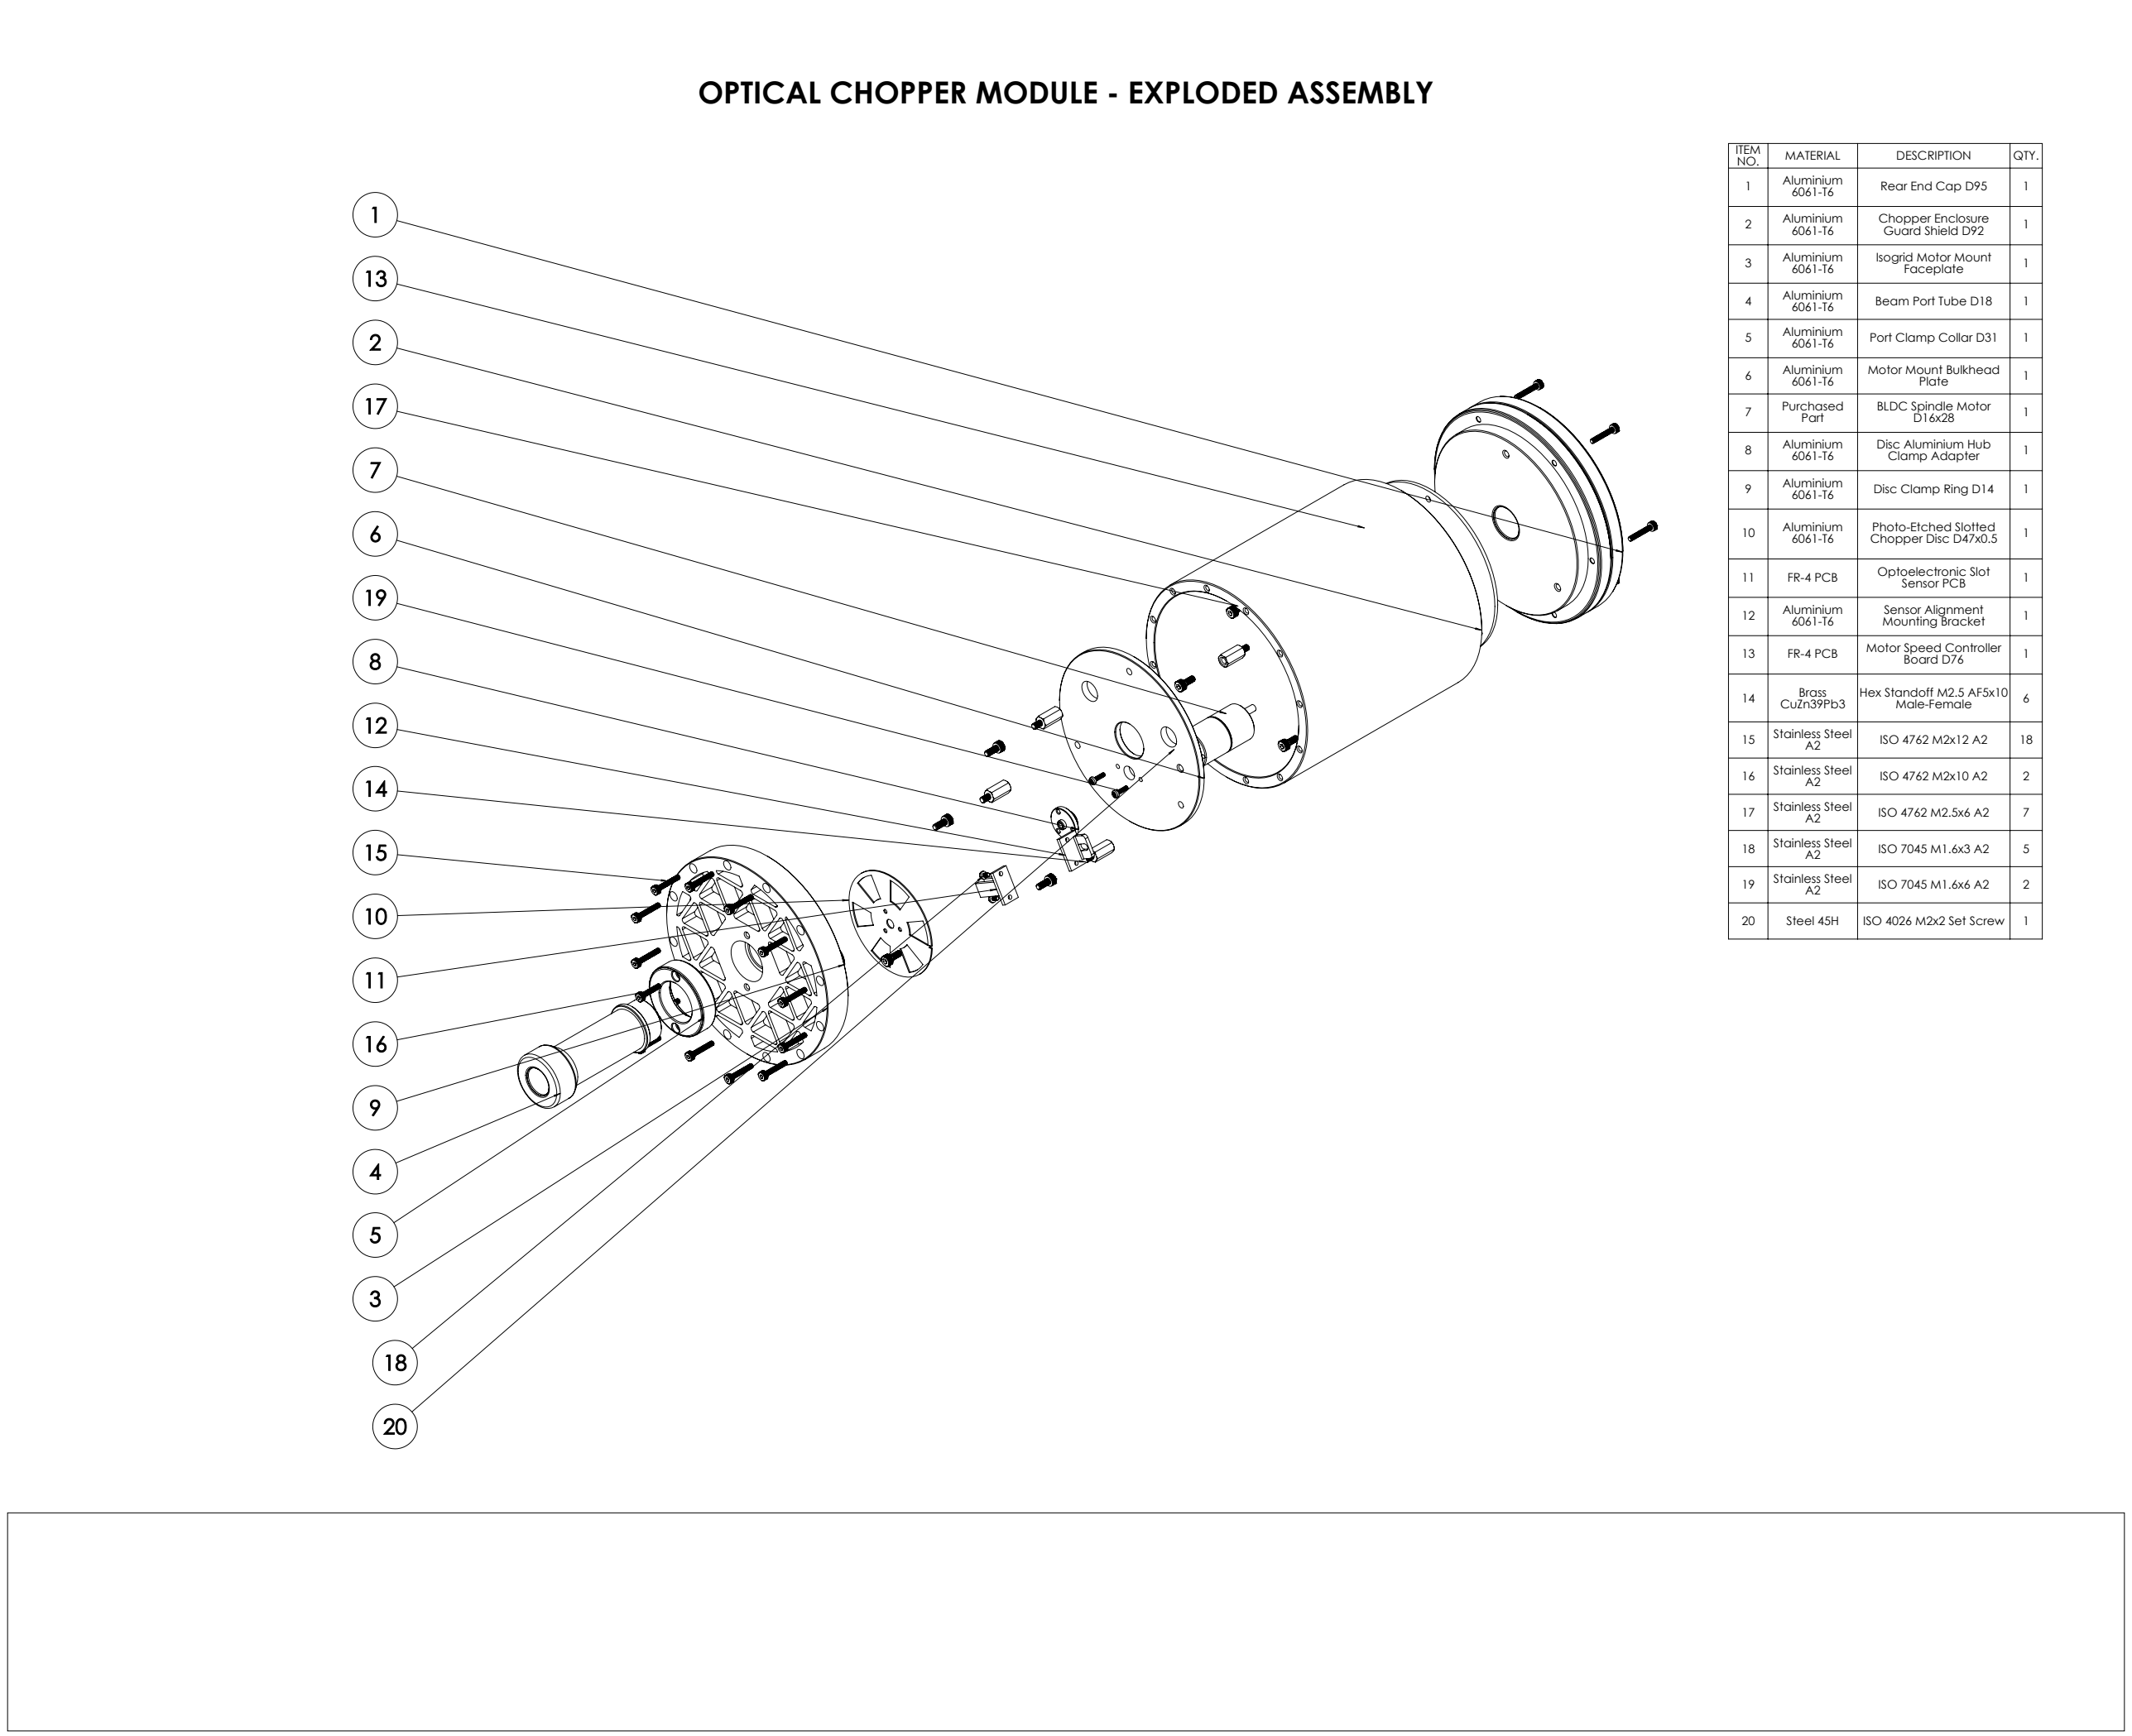
ISO-10303-21;
HEADER;
/* Generated by software containing ST-Developer
 * from STEP Tools, Inc. (www.steptools.com) 
 */

FILE_DESCRIPTION(
/* description */ (''),
/* implementation_level */ '2;1');

FILE_NAME(
/* name */ 'MAS-299',
/* time_stamp */ '2026-10-19T23:00:43-07:00',
/* author */ (''),
/* organization */ (''),
/* preprocessor_version */ 'ST-DEVELOPER v20.2',
/* originating_system */ 'Autodesk Translation Framework v15.15.0.0',
/* authorisation */ '');

FILE_SCHEMA (('AUTOMOTIVE_DESIGN { 1 0 10303 214 3 1 1 }'));
ENDSEC;

DATA;
#10=MECHANICAL_DESIGN_GEOMETRIC_PRESENTATION_REPRESENTATION('',(#996,#997,
#998,#999,#1000,#1001,#1002,#1003,#1004,#1005,#1006,#1007,#1008,#1009,#1010,
#1011,#1012,#1013,#1014,#1015),#55002);
#11=ITEM_DEFINED_TRANSFORMATION($,$,#24771,#27142);
#12=ITEM_DEFINED_TRANSFORMATION($,$,#24929,#27143);
#13=ITEM_DEFINED_TRANSFORMATION($,$,#25058,#27144);
#14=ITEM_DEFINED_TRANSFORMATION($,$,#25631,#27145);
#15=ITEM_DEFINED_TRANSFORMATION($,$,#25681,#27146);
#16=ITEM_DEFINED_TRANSFORMATION($,$,#25749,#27147);
#17=ITEM_DEFINED_TRANSFORMATION($,$,#25799,#27148);
#18=ITEM_DEFINED_TRANSFORMATION($,$,#25845,#27149);
#19=ITEM_DEFINED_TRANSFORMATION($,$,#25906,#27150);
#20=ITEM_DEFINED_TRANSFORMATION($,$,#25953,#27151);
#21=ITEM_DEFINED_TRANSFORMATION($,$,#26022,#27152);
#22=ITEM_DEFINED_TRANSFORMATION($,$,#26062,#27153);
#23=ITEM_DEFINED_TRANSFORMATION($,$,#26099,#27154);
#24=ITEM_DEFINED_TRANSFORMATION($,$,#26185,#27155);
#25=ITEM_DEFINED_TRANSFORMATION($,$,#26252,#27156);
#26=ITEM_DEFINED_TRANSFORMATION($,$,#26524,#27157);
#27=ITEM_DEFINED_TRANSFORMATION($,$,#26786,#27158);
#28=ITEM_DEFINED_TRANSFORMATION($,$,#27025,#27159);
#29=ITEM_DEFINED_TRANSFORMATION($,$,#27074,#27160);
#30=ITEM_DEFINED_TRANSFORMATION($,$,#26151,#27161);
#31=ITEM_DEFINED_TRANSFORMATION($,$,#26185,#27162);
#32=ITEM_DEFINED_TRANSFORMATION($,$,#26185,#27163);
#33=ITEM_DEFINED_TRANSFORMATION($,$,#26185,#27164);
#34=ITEM_DEFINED_TRANSFORMATION($,$,#26185,#27165);
#35=ITEM_DEFINED_TRANSFORMATION($,$,#26185,#27166);
#36=ITEM_DEFINED_TRANSFORMATION($,$,#26252,#27167);
#37=ITEM_DEFINED_TRANSFORMATION($,$,#26252,#27168);
#38=ITEM_DEFINED_TRANSFORMATION($,$,#26252,#27169);
#39=ITEM_DEFINED_TRANSFORMATION($,$,#26252,#27170);
#40=ITEM_DEFINED_TRANSFORMATION($,$,#26252,#27171);
#41=ITEM_DEFINED_TRANSFORMATION($,$,#26252,#27172);
#42=ITEM_DEFINED_TRANSFORMATION($,$,#26252,#27173);
#43=ITEM_DEFINED_TRANSFORMATION($,$,#26252,#27174);
#44=ITEM_DEFINED_TRANSFORMATION($,$,#26252,#27175);
#45=ITEM_DEFINED_TRANSFORMATION($,$,#26252,#27176);
#46=ITEM_DEFINED_TRANSFORMATION($,$,#26252,#27177);
#47=ITEM_DEFINED_TRANSFORMATION($,$,#26252,#27178);
#48=ITEM_DEFINED_TRANSFORMATION($,$,#26252,#27179);
#49=ITEM_DEFINED_TRANSFORMATION($,$,#26252,#27180);
#50=ITEM_DEFINED_TRANSFORMATION($,$,#26252,#27181);
#51=ITEM_DEFINED_TRANSFORMATION($,$,#26252,#27182);
#52=ITEM_DEFINED_TRANSFORMATION($,$,#26252,#27183);
#53=ITEM_DEFINED_TRANSFORMATION($,$,#26524,#27184);
#54=ITEM_DEFINED_TRANSFORMATION($,$,#26786,#27185);
#55=ITEM_DEFINED_TRANSFORMATION($,$,#26786,#27186);
#56=ITEM_DEFINED_TRANSFORMATION($,$,#26786,#27187);
#57=ITEM_DEFINED_TRANSFORMATION($,$,#26786,#27188);
#58=ITEM_DEFINED_TRANSFORMATION($,$,#26786,#27189);
#59=ITEM_DEFINED_TRANSFORMATION($,$,#26786,#27190);
#60=ITEM_DEFINED_TRANSFORMATION($,$,#27025,#27191);
#61=ITEM_DEFINED_TRANSFORMATION($,$,#27025,#27192);
#62=ITEM_DEFINED_TRANSFORMATION($,$,#27025,#27193);
#63=ITEM_DEFINED_TRANSFORMATION($,$,#27025,#27194);
#64=ITEM_DEFINED_TRANSFORMATION($,$,#27074,#27195);
#65=(
REPRESENTATION_RELATIONSHIP($,$,#55104,#55103)
REPRESENTATION_RELATIONSHIP_WITH_TRANSFORMATION(#11)
SHAPE_REPRESENTATION_RELATIONSHIP()
);
#66=(
REPRESENTATION_RELATIONSHIP($,$,#55105,#55103)
REPRESENTATION_RELATIONSHIP_WITH_TRANSFORMATION(#12)
SHAPE_REPRESENTATION_RELATIONSHIP()
);
#67=(
REPRESENTATION_RELATIONSHIP($,$,#55106,#55103)
REPRESENTATION_RELATIONSHIP_WITH_TRANSFORMATION(#13)
SHAPE_REPRESENTATION_RELATIONSHIP()
);
#68=(
REPRESENTATION_RELATIONSHIP($,$,#55107,#55103)
REPRESENTATION_RELATIONSHIP_WITH_TRANSFORMATION(#14)
SHAPE_REPRESENTATION_RELATIONSHIP()
);
#69=(
REPRESENTATION_RELATIONSHIP($,$,#55108,#55103)
REPRESENTATION_RELATIONSHIP_WITH_TRANSFORMATION(#15)
SHAPE_REPRESENTATION_RELATIONSHIP()
);
#70=(
REPRESENTATION_RELATIONSHIP($,$,#55109,#55103)
REPRESENTATION_RELATIONSHIP_WITH_TRANSFORMATION(#16)
SHAPE_REPRESENTATION_RELATIONSHIP()
);
#71=(
REPRESENTATION_RELATIONSHIP($,$,#55110,#55103)
REPRESENTATION_RELATIONSHIP_WITH_TRANSFORMATION(#17)
SHAPE_REPRESENTATION_RELATIONSHIP()
);
#72=(
REPRESENTATION_RELATIONSHIP($,$,#55111,#55103)
REPRESENTATION_RELATIONSHIP_WITH_TRANSFORMATION(#18)
SHAPE_REPRESENTATION_RELATIONSHIP()
);
#73=(
REPRESENTATION_RELATIONSHIP($,$,#55112,#55103)
REPRESENTATION_RELATIONSHIP_WITH_TRANSFORMATION(#19)
SHAPE_REPRESENTATION_RELATIONSHIP()
);
#74=(
REPRESENTATION_RELATIONSHIP($,$,#55113,#55103)
REPRESENTATION_RELATIONSHIP_WITH_TRANSFORMATION(#20)
SHAPE_REPRESENTATION_RELATIONSHIP()
);
#75=(
REPRESENTATION_RELATIONSHIP($,$,#55114,#55103)
REPRESENTATION_RELATIONSHIP_WITH_TRANSFORMATION(#21)
SHAPE_REPRESENTATION_RELATIONSHIP()
);
#76=(
REPRESENTATION_RELATIONSHIP($,$,#55115,#55103)
REPRESENTATION_RELATIONSHIP_WITH_TRANSFORMATION(#22)
SHAPE_REPRESENTATION_RELATIONSHIP()
);
#77=(
REPRESENTATION_RELATIONSHIP($,$,#55116,#55103)
REPRESENTATION_RELATIONSHIP_WITH_TRANSFORMATION(#23)
SHAPE_REPRESENTATION_RELATIONSHIP()
);
#78=(
REPRESENTATION_RELATIONSHIP($,$,#55118,#55103)
REPRESENTATION_RELATIONSHIP_WITH_TRANSFORMATION(#24)
SHAPE_REPRESENTATION_RELATIONSHIP()
);
#79=(
REPRESENTATION_RELATIONSHIP($,$,#55119,#55103)
REPRESENTATION_RELATIONSHIP_WITH_TRANSFORMATION(#25)
SHAPE_REPRESENTATION_RELATIONSHIP()
);
#80=(
REPRESENTATION_RELATIONSHIP($,$,#55120,#55103)
REPRESENTATION_RELATIONSHIP_WITH_TRANSFORMATION(#26)
SHAPE_REPRESENTATION_RELATIONSHIP()
);
#81=(
REPRESENTATION_RELATIONSHIP($,$,#55121,#55103)
REPRESENTATION_RELATIONSHIP_WITH_TRANSFORMATION(#27)
SHAPE_REPRESENTATION_RELATIONSHIP()
);
#82=(
REPRESENTATION_RELATIONSHIP($,$,#55122,#55103)
REPRESENTATION_RELATIONSHIP_WITH_TRANSFORMATION(#28)
SHAPE_REPRESENTATION_RELATIONSHIP()
);
#83=(
REPRESENTATION_RELATIONSHIP($,$,#55123,#55103)
REPRESENTATION_RELATIONSHIP_WITH_TRANSFORMATION(#29)
SHAPE_REPRESENTATION_RELATIONSHIP()
);
#84=(
REPRESENTATION_RELATIONSHIP($,$,#55117,#55103)
REPRESENTATION_RELATIONSHIP_WITH_TRANSFORMATION(#30)
SHAPE_REPRESENTATION_RELATIONSHIP()
);
#85=(
REPRESENTATION_RELATIONSHIP($,$,#55118,#55103)
REPRESENTATION_RELATIONSHIP_WITH_TRANSFORMATION(#31)
SHAPE_REPRESENTATION_RELATIONSHIP()
);
#86=(
REPRESENTATION_RELATIONSHIP($,$,#55118,#55103)
REPRESENTATION_RELATIONSHIP_WITH_TRANSFORMATION(#32)
SHAPE_REPRESENTATION_RELATIONSHIP()
);
#87=(
REPRESENTATION_RELATIONSHIP($,$,#55118,#55103)
REPRESENTATION_RELATIONSHIP_WITH_TRANSFORMATION(#33)
SHAPE_REPRESENTATION_RELATIONSHIP()
);
#88=(
REPRESENTATION_RELATIONSHIP($,$,#55118,#55103)
REPRESENTATION_RELATIONSHIP_WITH_TRANSFORMATION(#34)
SHAPE_REPRESENTATION_RELATIONSHIP()
);
#89=(
REPRESENTATION_RELATIONSHIP($,$,#55118,#55103)
REPRESENTATION_RELATIONSHIP_WITH_TRANSFORMATION(#35)
SHAPE_REPRESENTATION_RELATIONSHIP()
);
#90=(
REPRESENTATION_RELATIONSHIP($,$,#55119,#55103)
REPRESENTATION_RELATIONSHIP_WITH_TRANSFORMATION(#36)
SHAPE_REPRESENTATION_RELATIONSHIP()
);
#91=(
REPRESENTATION_RELATIONSHIP($,$,#55119,#55103)
REPRESENTATION_RELATIONSHIP_WITH_TRANSFORMATION(#37)
SHAPE_REPRESENTATION_RELATIONSHIP()
);
#92=(
REPRESENTATION_RELATIONSHIP($,$,#55119,#55103)
REPRESENTATION_RELATIONSHIP_WITH_TRANSFORMATION(#38)
SHAPE_REPRESENTATION_RELATIONSHIP()
);
#93=(
REPRESENTATION_RELATIONSHIP($,$,#55119,#55103)
REPRESENTATION_RELATIONSHIP_WITH_TRANSFORMATION(#39)
SHAPE_REPRESENTATION_RELATIONSHIP()
);
#94=(
REPRESENTATION_RELATIONSHIP($,$,#55119,#55103)
REPRESENTATION_RELATIONSHIP_WITH_TRANSFORMATION(#40)
SHAPE_REPRESENTATION_RELATIONSHIP()
);
#95=(
REPRESENTATION_RELATIONSHIP($,$,#55119,#55103)
REPRESENTATION_RELATIONSHIP_WITH_TRANSFORMATION(#41)
SHAPE_REPRESENTATION_RELATIONSHIP()
);
#96=(
REPRESENTATION_RELATIONSHIP($,$,#55119,#55103)
REPRESENTATION_RELATIONSHIP_WITH_TRANSFORMATION(#42)
SHAPE_REPRESENTATION_RELATIONSHIP()
);
#97=(
REPRESENTATION_RELATIONSHIP($,$,#55119,#55103)
REPRESENTATION_RELATIONSHIP_WITH_TRANSFORMATION(#43)
SHAPE_REPRESENTATION_RELATIONSHIP()
);
#98=(
REPRESENTATION_RELATIONSHIP($,$,#55119,#55103)
REPRESENTATION_RELATIONSHIP_WITH_TRANSFORMATION(#44)
SHAPE_REPRESENTATION_RELATIONSHIP()
);
#99=(
REPRESENTATION_RELATIONSHIP($,$,#55119,#55103)
REPRESENTATION_RELATIONSHIP_WITH_TRANSFORMATION(#45)
SHAPE_REPRESENTATION_RELATIONSHIP()
);
#100=(
REPRESENTATION_RELATIONSHIP($,$,#55119,#55103)
REPRESENTATION_RELATIONSHIP_WITH_TRANSFORMATION(#46)
SHAPE_REPRESENTATION_RELATIONSHIP()
);
#101=(
REPRESENTATION_RELATIONSHIP($,$,#55119,#55103)
REPRESENTATION_RELATIONSHIP_WITH_TRANSFORMATION(#47)
SHAPE_REPRESENTATION_RELATIONSHIP()
);
#102=(
REPRESENTATION_RELATIONSHIP($,$,#55119,#55103)
REPRESENTATION_RELATIONSHIP_WITH_TRANSFORMATION(#48)
SHAPE_REPRESENTATION_RELATIONSHIP()
);
#103=(
REPRESENTATION_RELATIONSHIP($,$,#55119,#55103)
REPRESENTATION_RELATIONSHIP_WITH_TRANSFORMATION(#49)
SHAPE_REPRESENTATION_RELATIONSHIP()
);
#104=(
REPRESENTATION_RELATIONSHIP($,$,#55119,#55103)
REPRESENTATION_RELATIONSHIP_WITH_TRANSFORMATION(#50)
SHAPE_REPRESENTATION_RELATIONSHIP()
);
#105=(
REPRESENTATION_RELATIONSHIP($,$,#55119,#55103)
REPRESENTATION_RELATIONSHIP_WITH_TRANSFORMATION(#51)
SHAPE_REPRESENTATION_RELATIONSHIP()
);
#106=(
REPRESENTATION_RELATIONSHIP($,$,#55119,#55103)
REPRESENTATION_RELATIONSHIP_WITH_TRANSFORMATION(#52)
SHAPE_REPRESENTATION_RELATIONSHIP()
);
#107=(
REPRESENTATION_RELATIONSHIP($,$,#55120,#55103)
REPRESENTATION_RELATIONSHIP_WITH_TRANSFORMATION(#53)
SHAPE_REPRESENTATION_RELATIONSHIP()
);
#108=(
REPRESENTATION_RELATIONSHIP($,$,#55121,#55103)
REPRESENTATION_RELATIONSHIP_WITH_TRANSFORMATION(#54)
SHAPE_REPRESENTATION_RELATIONSHIP()
);
#109=(
REPRESENTATION_RELATIONSHIP($,$,#55121,#55103)
REPRESENTATION_RELATIONSHIP_WITH_TRANSFORMATION(#55)
SHAPE_REPRESENTATION_RELATIONSHIP()
);
#110=(
REPRESENTATION_RELATIONSHIP($,$,#55121,#55103)
REPRESENTATION_RELATIONSHIP_WITH_TRANSFORMATION(#56)
SHAPE_REPRESENTATION_RELATIONSHIP()
);
#111=(
REPRESENTATION_RELATIONSHIP($,$,#55121,#55103)
REPRESENTATION_RELATIONSHIP_WITH_TRANSFORMATION(#57)
SHAPE_REPRESENTATION_RELATIONSHIP()
);
#112=(
REPRESENTATION_RELATIONSHIP($,$,#55121,#55103)
REPRESENTATION_RELATIONSHIP_WITH_TRANSFORMATION(#58)
SHAPE_REPRESENTATION_RELATIONSHIP()
);
#113=(
REPRESENTATION_RELATIONSHIP($,$,#55121,#55103)
REPRESENTATION_RELATIONSHIP_WITH_TRANSFORMATION(#59)
SHAPE_REPRESENTATION_RELATIONSHIP()
);
#114=(
REPRESENTATION_RELATIONSHIP($,$,#55122,#55103)
REPRESENTATION_RELATIONSHIP_WITH_TRANSFORMATION(#60)
SHAPE_REPRESENTATION_RELATIONSHIP()
);
#115=(
REPRESENTATION_RELATIONSHIP($,$,#55122,#55103)
REPRESENTATION_RELATIONSHIP_WITH_TRANSFORMATION(#61)
SHAPE_REPRESENTATION_RELATIONSHIP()
);
#116=(
REPRESENTATION_RELATIONSHIP($,$,#55122,#55103)
REPRESENTATION_RELATIONSHIP_WITH_TRANSFORMATION(#62)
SHAPE_REPRESENTATION_RELATIONSHIP()
);
#117=(
REPRESENTATION_RELATIONSHIP($,$,#55122,#55103)
REPRESENTATION_RELATIONSHIP_WITH_TRANSFORMATION(#63)
SHAPE_REPRESENTATION_RELATIONSHIP()
);
#118=(
REPRESENTATION_RELATIONSHIP($,$,#55123,#55103)
REPRESENTATION_RELATIONSHIP_WITH_TRANSFORMATION(#64)
SHAPE_REPRESENTATION_RELATIONSHIP()
);
#119=CONTEXT_DEPENDENT_SHAPE_REPRESENTATION(#65,#55049);
#120=CONTEXT_DEPENDENT_SHAPE_REPRESENTATION(#66,#55050);
#121=CONTEXT_DEPENDENT_SHAPE_REPRESENTATION(#67,#55051);
#122=CONTEXT_DEPENDENT_SHAPE_REPRESENTATION(#68,#55052);
#123=CONTEXT_DEPENDENT_SHAPE_REPRESENTATION(#69,#55053);
#124=CONTEXT_DEPENDENT_SHAPE_REPRESENTATION(#70,#55054);
#125=CONTEXT_DEPENDENT_SHAPE_REPRESENTATION(#71,#55055);
#126=CONTEXT_DEPENDENT_SHAPE_REPRESENTATION(#72,#55056);
#127=CONTEXT_DEPENDENT_SHAPE_REPRESENTATION(#73,#55057);
#128=CONTEXT_DEPENDENT_SHAPE_REPRESENTATION(#74,#55058);
#129=CONTEXT_DEPENDENT_SHAPE_REPRESENTATION(#75,#55059);
#130=CONTEXT_DEPENDENT_SHAPE_REPRESENTATION(#76,#55060);
#131=CONTEXT_DEPENDENT_SHAPE_REPRESENTATION(#77,#55061);
#132=CONTEXT_DEPENDENT_SHAPE_REPRESENTATION(#78,#55062);
#133=CONTEXT_DEPENDENT_SHAPE_REPRESENTATION(#79,#55063);
#134=CONTEXT_DEPENDENT_SHAPE_REPRESENTATION(#80,#55064);
#135=CONTEXT_DEPENDENT_SHAPE_REPRESENTATION(#81,#55065);
#136=CONTEXT_DEPENDENT_SHAPE_REPRESENTATION(#82,#55066);
#137=CONTEXT_DEPENDENT_SHAPE_REPRESENTATION(#83,#55067);
#138=CONTEXT_DEPENDENT_SHAPE_REPRESENTATION(#84,#55068);
#139=CONTEXT_DEPENDENT_SHAPE_REPRESENTATION(#85,#55069);
#140=CONTEXT_DEPENDENT_SHAPE_REPRESENTATION(#86,#55070);
#141=CONTEXT_DEPENDENT_SHAPE_REPRESENTATION(#87,#55071);
#142=CONTEXT_DEPENDENT_SHAPE_REPRESENTATION(#88,#55072);
#143=CONTEXT_DEPENDENT_SHAPE_REPRESENTATION(#89,#55073);
#144=CONTEXT_DEPENDENT_SHAPE_REPRESENTATION(#90,#55074);
#145=CONTEXT_DEPENDENT_SHAPE_REPRESENTATION(#91,#55075);
#146=CONTEXT_DEPENDENT_SHAPE_REPRESENTATION(#92,#55076);
#147=CONTEXT_DEPENDENT_SHAPE_REPRESENTATION(#93,#55077);
#148=CONTEXT_DEPENDENT_SHAPE_REPRESENTATION(#94,#55078);
#149=CONTEXT_DEPENDENT_SHAPE_REPRESENTATION(#95,#55079);
#150=CONTEXT_DEPENDENT_SHAPE_REPRESENTATION(#96,#55080);
#151=CONTEXT_DEPENDENT_SHAPE_REPRESENTATION(#97,#55081);
#152=CONTEXT_DEPENDENT_SHAPE_REPRESENTATION(#98,#55082);
#153=CONTEXT_DEPENDENT_SHAPE_REPRESENTATION(#99,#55083);
#154=CONTEXT_DEPENDENT_SHAPE_REPRESENTATION(#100,#55084);
#155=CONTEXT_DEPENDENT_SHAPE_REPRESENTATION(#101,#55085);
#156=CONTEXT_DEPENDENT_SHAPE_REPRESENTATION(#102,#55086);
#157=CONTEXT_DEPENDENT_SHAPE_REPRESENTATION(#103,#55087);
#158=CONTEXT_DEPENDENT_SHAPE_REPRESENTATION(#104,#55088);
#159=CONTEXT_DEPENDENT_SHAPE_REPRESENTATION(#105,#55089);
#160=CONTEXT_DEPENDENT_SHAPE_REPRESENTATION(#106,#55090);
#161=CONTEXT_DEPENDENT_SHAPE_REPRESENTATION(#107,#55091);
#162=CONTEXT_DEPENDENT_SHAPE_REPRESENTATION(#108,#55092);
#163=CONTEXT_DEPENDENT_SHAPE_REPRESENTATION(#109,#55093);
#164=CONTEXT_DEPENDENT_SHAPE_REPRESENTATION(#110,#55094);
#165=CONTEXT_DEPENDENT_SHAPE_REPRESENTATION(#111,#55095);
#166=CONTEXT_DEPENDENT_SHAPE_REPRESENTATION(#112,#55096);
#167=CONTEXT_DEPENDENT_SHAPE_REPRESENTATION(#113,#55097);
#168=CONTEXT_DEPENDENT_SHAPE_REPRESENTATION(#114,#55098);
#169=CONTEXT_DEPENDENT_SHAPE_REPRESENTATION(#115,#55099);
#170=CONTEXT_DEPENDENT_SHAPE_REPRESENTATION(#116,#55100);
#171=CONTEXT_DEPENDENT_SHAPE_REPRESENTATION(#117,#55101);
#172=CONTEXT_DEPENDENT_SHAPE_REPRESENTATION(#118,#55102);
#173=NEXT_ASSEMBLY_USAGE_OCCURRENCE('01_Rear_End_Cap_D95:1',
'01_Rear_End_Cap_D95:1','01_Rear_End_Cap_D95:1',#55125,#55126,
'01_Rear_End_Cap_D95:1');
#174=NEXT_ASSEMBLY_USAGE_OCCURRENCE(
'02_Chopper_Enclosure_Guard_Shield_D92:1',
'02_Chopper_Enclosure_Guard_Shield_D92:1',
'02_Chopper_Enclosure_Guard_Shield_D92:1',#55125,#55127,
'02_Chopper_Enclosure_Guard_Shield_D92:1');
#175=NEXT_ASSEMBLY_USAGE_OCCURRENCE(
'03_Isogrid_Motor_Mount_Faceplate:1',
'03_Isogrid_Motor_Mount_Faceplate:1',
'03_Isogrid_Motor_Mount_Faceplate:1',#55125,#55128,
'03_Isogrid_Motor_Mount_Faceplate:1');
#176=NEXT_ASSEMBLY_USAGE_OCCURRENCE('04_Beam_Port_Tube_D18:1',
'04_Beam_Port_Tube_D18:1','04_Beam_Port_Tube_D18:1',#55125,#55129,
'04_Beam_Port_Tube_D18:1');
#177=NEXT_ASSEMBLY_USAGE_OCCURRENCE('05_Port_Clamp_Collar_D31:1',
'05_Port_Clamp_Collar_D31:1','05_Port_Clamp_Collar_D31:1',#55125,#55130,
'05_Port_Clamp_Collar_D31:1');
#178=NEXT_ASSEMBLY_USAGE_OCCURRENCE('06_Motor_Mount_Bulkhead_Plate:1',
'06_Motor_Mount_Bulkhead_Plate:1','06_Motor_Mount_Bulkhead_Plate:1',#55125,
#55131,'06_Motor_Mount_Bulkhead_Plate:1');
#179=NEXT_ASSEMBLY_USAGE_OCCURRENCE('07_BLDC_Spindle_Motor_D16x28:1',
'07_BLDC_Spindle_Motor_D16x28:1','07_BLDC_Spindle_Motor_D16x28:1',#55125,
#55132,'07_BLDC_Spindle_Motor_D16x28:1');
#180=NEXT_ASSEMBLY_USAGE_OCCURRENCE(
'08_Disc_Aluminium_Hub_Clamp_Adapter:1',
'08_Disc_Aluminium_Hub_Clamp_Adapter:1',
'08_Disc_Aluminium_Hub_Clamp_Adapter:1',#55125,#55133,
'08_Disc_Aluminium_Hub_Clamp_Adapter:1');
#181=NEXT_ASSEMBLY_USAGE_OCCURRENCE('09_Disc_Clamp_Ring_D14:1',
'09_Disc_Clamp_Ring_D14:1','09_Disc_Clamp_Ring_D14:1',#55125,#55134,
'09_Disc_Clamp_Ring_D14:1');
#182=NEXT_ASSEMBLY_USAGE_OCCURRENCE(
'10_Photo-Etched_Slotted_Chopper_Disc_D47x0.5:1',
'10_Photo-Etched_Slotted_Chopper_Disc_D47x0.5:1',
'10_Photo-Etched_Slotted_Chopper_Disc_D47x0.5:1',#55125,#55135,
'10_Photo-Etched_Slotted_Chopper_Disc_D47x0.5:1');
#183=NEXT_ASSEMBLY_USAGE_OCCURRENCE(
'11_Optoelectronic_Slot_Sensor_PCB:1',
'11_Optoelectronic_Slot_Sensor_PCB:1',
'11_Optoelectronic_Slot_Sensor_PCB:1',#55125,#55136,
'11_Optoelectronic_Slot_Sensor_PCB:1');
#184=NEXT_ASSEMBLY_USAGE_OCCURRENCE(
'12_Sensor_Alignment_Mounting_Bracket:1',
'12_Sensor_Alignment_Mounting_Bracket:1',
'12_Sensor_Alignment_Mounting_Bracket:1',#55125,#55137,
'12_Sensor_Alignment_Mounting_Bracket:1');
#185=NEXT_ASSEMBLY_USAGE_OCCURRENCE(
'13_Motor_Speed_Controller_Board_D76:1',
'13_Motor_Speed_Controller_Board_D76:1',
'13_Motor_Speed_Controller_Board_D76:1',#55125,#55138,
'13_Motor_Speed_Controller_Board_D76:1');
#186=NEXT_ASSEMBLY_USAGE_OCCURRENCE(
'14_Hex_Standoff_M2.5_AF5x10_Male-Female:1',
'14_Hex_Standoff_M2.5_AF5x10_Male-Female:1',
'14_Hex_Standoff_M2.5_AF5x10_Male-Female:1',#55125,#55140,
'14_Hex_Standoff_M2.5_AF5x10_Male-Female:1');
#187=NEXT_ASSEMBLY_USAGE_OCCURRENCE('15_ISO_4762_M2x12_A2:1',
'15_ISO_4762_M2x12_A2:1','15_ISO_4762_M2x12_A2:1',#55125,#55141,
'15_ISO_4762_M2x12_A2:1');
#188=NEXT_ASSEMBLY_USAGE_OCCURRENCE('16_ISO_4762_M2x10_A2:1',
'16_ISO_4762_M2x10_A2:1','16_ISO_4762_M2x10_A2:1',#55125,#55142,
'16_ISO_4762_M2x10_A2:1');
#189=NEXT_ASSEMBLY_USAGE_OCCURRENCE('17_ISO_4762_M2.5x6_A2:1',
'17_ISO_4762_M2.5x6_A2:1','17_ISO_4762_M2.5x6_A2:1',#55125,#55143,
'17_ISO_4762_M2.5x6_A2:1');
#190=NEXT_ASSEMBLY_USAGE_OCCURRENCE('18_ISO_7045_M1.6x3_A2:1',
'18_ISO_7045_M1.6x3_A2:1','18_ISO_7045_M1.6x3_A2:1',#55125,#55144,
'18_ISO_7045_M1.6x3_A2:1');
#191=NEXT_ASSEMBLY_USAGE_OCCURRENCE('19_ISO_7045_M1.6x6_A2:1',
'19_ISO_7045_M1.6x6_A2:1','19_ISO_7045_M1.6x6_A2:1',#55125,#55145,
'19_ISO_7045_M1.6x6_A2:1');
#192=NEXT_ASSEMBLY_USAGE_OCCURRENCE('20_ISO_4026_M2x2_Set_Screw:1',
'20_ISO_4026_M2x2_Set_Screw:1','20_ISO_4026_M2x2_Set_Screw:1',#55125,#55139,
'20_ISO_4026_M2x2_Set_Screw:1');
#193=NEXT_ASSEMBLY_USAGE_OCCURRENCE(
'14_Hex_Standoff_M2.5_AF5x10_Male-Female:2',
'14_Hex_Standoff_M2.5_AF5x10_Male-Female:2',
'14_Hex_Standoff_M2.5_AF5x10_Male-Female:2',#55125,#55140,
'14_Hex_Standoff_M2.5_AF5x10_Male-Female:2');
#194=NEXT_ASSEMBLY_USAGE_OCCURRENCE(
'14_Hex_Standoff_M2.5_AF5x10_Male-Female:3',
'14_Hex_Standoff_M2.5_AF5x10_Male-Female:3',
'14_Hex_Standoff_M2.5_AF5x10_Male-Female:3',#55125,#55140,
'14_Hex_Standoff_M2.5_AF5x10_Male-Female:3');
#195=NEXT_ASSEMBLY_USAGE_OCCURRENCE(
'14_Hex_Standoff_M2.5_AF5x10_Male-Female:4',
'14_Hex_Standoff_M2.5_AF5x10_Male-Female:4',
'14_Hex_Standoff_M2.5_AF5x10_Male-Female:4',#55125,#55140,
'14_Hex_Standoff_M2.5_AF5x10_Male-Female:4');
#196=NEXT_ASSEMBLY_USAGE_OCCURRENCE(
'14_Hex_Standoff_M2.5_AF5x10_Male-Female:5',
'14_Hex_Standoff_M2.5_AF5x10_Male-Female:5',
'14_Hex_Standoff_M2.5_AF5x10_Male-Female:5',#55125,#55140,
'14_Hex_Standoff_M2.5_AF5x10_Male-Female:5');
#197=NEXT_ASSEMBLY_USAGE_OCCURRENCE(
'14_Hex_Standoff_M2.5_AF5x10_Male-Female:6',
'14_Hex_Standoff_M2.5_AF5x10_Male-Female:6',
'14_Hex_Standoff_M2.5_AF5x10_Male-Female:6',#55125,#55140,
'14_Hex_Standoff_M2.5_AF5x10_Male-Female:6');
#198=NEXT_ASSEMBLY_USAGE_OCCURRENCE('15_ISO_4762_M2x12_A2:2',
'15_ISO_4762_M2x12_A2:2','15_ISO_4762_M2x12_A2:2',#55125,#55141,
'15_ISO_4762_M2x12_A2:2');
#199=NEXT_ASSEMBLY_USAGE_OCCURRENCE('15_ISO_4762_M2x12_A2:3',
'15_ISO_4762_M2x12_A2:3','15_ISO_4762_M2x12_A2:3',#55125,#55141,
'15_ISO_4762_M2x12_A2:3');
#200=NEXT_ASSEMBLY_USAGE_OCCURRENCE('15_ISO_4762_M2x12_A2:4',
'15_ISO_4762_M2x12_A2:4','15_ISO_4762_M2x12_A2:4',#55125,#55141,
'15_ISO_4762_M2x12_A2:4');
#201=NEXT_ASSEMBLY_USAGE_OCCURRENCE('15_ISO_4762_M2x12_A2:5',
'15_ISO_4762_M2x12_A2:5','15_ISO_4762_M2x12_A2:5',#55125,#55141,
'15_ISO_4762_M2x12_A2:5');
#202=NEXT_ASSEMBLY_USAGE_OCCURRENCE('15_ISO_4762_M2x12_A2:6',
'15_ISO_4762_M2x12_A2:6','15_ISO_4762_M2x12_A2:6',#55125,#55141,
'15_ISO_4762_M2x12_A2:6');
#203=NEXT_ASSEMBLY_USAGE_OCCURRENCE('15_ISO_4762_M2x12_A2:7',
'15_ISO_4762_M2x12_A2:7','15_ISO_4762_M2x12_A2:7',#55125,#55141,
'15_ISO_4762_M2x12_A2:7');
#204=NEXT_ASSEMBLY_USAGE_OCCURRENCE('15_ISO_4762_M2x12_A2:8',
'15_ISO_4762_M2x12_A2:8','15_ISO_4762_M2x12_A2:8',#55125,#55141,
'15_ISO_4762_M2x12_A2:8');
#205=NEXT_ASSEMBLY_USAGE_OCCURRENCE('15_ISO_4762_M2x12_A2:9',
'15_ISO_4762_M2x12_A2:9','15_ISO_4762_M2x12_A2:9',#55125,#55141,
'15_ISO_4762_M2x12_A2:9');
#206=NEXT_ASSEMBLY_USAGE_OCCURRENCE('15_ISO_4762_M2x12_A2:10',
'15_ISO_4762_M2x12_A2:10','15_ISO_4762_M2x12_A2:10',#55125,#55141,
'15_ISO_4762_M2x12_A2:10');
#207=NEXT_ASSEMBLY_USAGE_OCCURRENCE('15_ISO_4762_M2x12_A2:11',
'15_ISO_4762_M2x12_A2:11','15_ISO_4762_M2x12_A2:11',#55125,#55141,
'15_ISO_4762_M2x12_A2:11');
#208=NEXT_ASSEMBLY_USAGE_OCCURRENCE('15_ISO_4762_M2x12_A2:12',
'15_ISO_4762_M2x12_A2:12','15_ISO_4762_M2x12_A2:12',#55125,#55141,
'15_ISO_4762_M2x12_A2:12');
#209=NEXT_ASSEMBLY_USAGE_OCCURRENCE('15_ISO_4762_M2x12_A2:13',
'15_ISO_4762_M2x12_A2:13','15_ISO_4762_M2x12_A2:13',#55125,#55141,
'15_ISO_4762_M2x12_A2:13');
#210=NEXT_ASSEMBLY_USAGE_OCCURRENCE('15_ISO_4762_M2x12_A2:14',
'15_ISO_4762_M2x12_A2:14','15_ISO_4762_M2x12_A2:14',#55125,#55141,
'15_ISO_4762_M2x12_A2:14');
#211=NEXT_ASSEMBLY_USAGE_OCCURRENCE('15_ISO_4762_M2x12_A2:15',
'15_ISO_4762_M2x12_A2:15','15_ISO_4762_M2x12_A2:15',#55125,#55141,
'15_ISO_4762_M2x12_A2:15');
#212=NEXT_ASSEMBLY_USAGE_OCCURRENCE('15_ISO_4762_M2x12_A2:16',
'15_ISO_4762_M2x12_A2:16','15_ISO_4762_M2x12_A2:16',#55125,#55141,
'15_ISO_4762_M2x12_A2:16');
#213=NEXT_ASSEMBLY_USAGE_OCCURRENCE('15_ISO_4762_M2x12_A2:17',
'15_ISO_4762_M2x12_A2:17','15_ISO_4762_M2x12_A2:17',#55125,#55141,
'15_ISO_4762_M2x12_A2:17');
#214=NEXT_ASSEMBLY_USAGE_OCCURRENCE('15_ISO_4762_M2x12_A2:18',
'15_ISO_4762_M2x12_A2:18','15_ISO_4762_M2x12_A2:18',#55125,#55141,
'15_ISO_4762_M2x12_A2:18');
#215=NEXT_ASSEMBLY_USAGE_OCCURRENCE('16_ISO_4762_M2x10_A2:2',
'16_ISO_4762_M2x10_A2:2','16_ISO_4762_M2x10_A2:2',#55125,#55142,
'16_ISO_4762_M2x10_A2:2');
#216=NEXT_ASSEMBLY_USAGE_OCCURRENCE('17_ISO_4762_M2.5x6_A2:2',
'17_ISO_4762_M2.5x6_A2:2','17_ISO_4762_M2.5x6_A2:2',#55125,#55143,
'17_ISO_4762_M2.5x6_A2:2');
#217=NEXT_ASSEMBLY_USAGE_OCCURRENCE('17_ISO_4762_M2.5x6_A2:3',
'17_ISO_4762_M2.5x6_A2:3','17_ISO_4762_M2.5x6_A2:3',#55125,#55143,
'17_ISO_4762_M2.5x6_A2:3');
#218=NEXT_ASSEMBLY_USAGE_OCCURRENCE('17_ISO_4762_M2.5x6_A2:4',
'17_ISO_4762_M2.5x6_A2:4','17_ISO_4762_M2.5x6_A2:4',#55125,#55143,
'17_ISO_4762_M2.5x6_A2:4');
#219=NEXT_ASSEMBLY_USAGE_OCCURRENCE('17_ISO_4762_M2.5x6_A2:5',
'17_ISO_4762_M2.5x6_A2:5','17_ISO_4762_M2.5x6_A2:5',#55125,#55143,
'17_ISO_4762_M2.5x6_A2:5');
#220=NEXT_ASSEMBLY_USAGE_OCCURRENCE('17_ISO_4762_M2.5x6_A2:6',
'17_ISO_4762_M2.5x6_A2:6','17_ISO_4762_M2.5x6_A2:6',#55125,#55143,
'17_ISO_4762_M2.5x6_A2:6');
#221=NEXT_ASSEMBLY_USAGE_OCCURRENCE('17_ISO_4762_M2.5x6_A2:7',
'17_ISO_4762_M2.5x6_A2:7','17_ISO_4762_M2.5x6_A2:7',#55125,#55143,
'17_ISO_4762_M2.5x6_A2:7');
#222=NEXT_ASSEMBLY_USAGE_OCCURRENCE('18_ISO_7045_M1.6x3_A2:2',
'18_ISO_7045_M1.6x3_A2:2','18_ISO_7045_M1.6x3_A2:2',#55125,#55144,
'18_ISO_7045_M1.6x3_A2:2');
#223=NEXT_ASSEMBLY_USAGE_OCCURRENCE('18_ISO_7045_M1.6x3_A2:3',
'18_ISO_7045_M1.6x3_A2:3','18_ISO_7045_M1.6x3_A2:3',#55125,#55144,
'18_ISO_7045_M1.6x3_A2:3');
#224=NEXT_ASSEMBLY_USAGE_OCCURRENCE('18_ISO_7045_M1.6x3_A2:4',
'18_ISO_7045_M1.6x3_A2:4','18_ISO_7045_M1.6x3_A2:4',#55125,#55144,
'18_ISO_7045_M1.6x3_A2:4');
#225=NEXT_ASSEMBLY_USAGE_OCCURRENCE('18_ISO_7045_M1.6x3_A2:5',
'18_ISO_7045_M1.6x3_A2:5','18_ISO_7045_M1.6x3_A2:5',#55125,#55144,
'18_ISO_7045_M1.6x3_A2:5');
#226=NEXT_ASSEMBLY_USAGE_OCCURRENCE('19_ISO_7045_M1.6x6_A2:2',
'19_ISO_7045_M1.6x6_A2:2','19_ISO_7045_M1.6x6_A2:2',#55125,#55145,
'19_ISO_7045_M1.6x6_A2:2');
#227=(
BOUNDED_CURVE()
B_SPLINE_CURVE(2,(#39814,#39815,#39816),.UNSPECIFIED.,.F.,.F.)
B_SPLINE_CURVE_WITH_KNOTS((3,3),(0.0560176289802603,0.163687850794567),
 .UNSPECIFIED.)
CURVE()
GEOMETRIC_REPRESENTATION_ITEM()
RATIONAL_B_SPLINE_CURVE((1.01603499393247,1.02342774714042,1.))
REPRESENTATION_ITEM('')
);
#228=(
BOUNDED_CURVE()
B_SPLINE_CURVE(2,(#39818,#39819,#39820),.UNSPECIFIED.,.F.,.F.)
B_SPLINE_CURVE_WITH_KNOTS((3,3),(0.,0.107670221814307),.UNSPECIFIED.)
CURVE()
GEOMETRIC_REPRESENTATION_ITEM()
RATIONAL_B_SPLINE_CURVE((1.,1.02342774714043,1.01603499393248))
REPRESENTATION_ITEM('')
);
#229=(
BOUNDED_CURVE()
B_SPLINE_CURVE(2,(#39825,#39826,#39827),.UNSPECIFIED.,.F.,.F.)
B_SPLINE_CURVE_WITH_KNOTS((3,3),(0.0560176289802603,0.163687850794567),
 .UNSPECIFIED.)
CURVE()
GEOMETRIC_REPRESENTATION_ITEM()
RATIONAL_B_SPLINE_CURVE((1.01603499393248,1.02342774714042,1.))
REPRESENTATION_ITEM('')
);
#230=(
BOUNDED_CURVE()
B_SPLINE_CURVE(2,(#39829,#39830,#39831),.UNSPECIFIED.,.F.,.F.)
B_SPLINE_CURVE_WITH_KNOTS((3,3),(0.,0.107670221814307),.UNSPECIFIED.)
CURVE()
GEOMETRIC_REPRESENTATION_ITEM()
RATIONAL_B_SPLINE_CURVE((1.,1.02342774714042,1.01603499393248))
REPRESENTATION_ITEM('')
);
#231=(
BOUNDED_CURVE()
B_SPLINE_CURVE(2,(#39836,#39837,#39838),.UNSPECIFIED.,.F.,.F.)
B_SPLINE_CURVE_WITH_KNOTS((3,3),(0.0560176289802603,0.163687850794567),
 .UNSPECIFIED.)
CURVE()
GEOMETRIC_REPRESENTATION_ITEM()
RATIONAL_B_SPLINE_CURVE((1.01603499393248,1.02342774714042,1.))
REPRESENTATION_ITEM('')
);
#232=(
BOUNDED_CURVE()
B_SPLINE_CURVE(2,(#39840,#39841,#39842),.UNSPECIFIED.,.F.,.F.)
B_SPLINE_CURVE_WITH_KNOTS((3,3),(0.,0.107670221814307),.UNSPECIFIED.)
CURVE()
GEOMETRIC_REPRESENTATION_ITEM()
RATIONAL_B_SPLINE_CURVE((1.,1.02342774714043,1.01603499393248))
REPRESENTATION_ITEM('')
);
#233=(
BOUNDED_CURVE()
B_SPLINE_CURVE(2,(#39847,#39848,#39849),.UNSPECIFIED.,.F.,.F.)
B_SPLINE_CURVE_WITH_KNOTS((3,3),(0.0560176289802605,0.163687850794567),
 .UNSPECIFIED.)
CURVE()
GEOMETRIC_REPRESENTATION_ITEM()
RATIONAL_B_SPLINE_CURVE((1.01603499393247,1.02342774714041,1.))
REPRESENTATION_ITEM('')
);
#234=(
BOUNDED_CURVE()
B_SPLINE_CURVE(2,(#39851,#39852,#39853),.UNSPECIFIED.,.F.,.F.)
B_SPLINE_CURVE_WITH_KNOTS((3,3),(0.,0.107670221814307),.UNSPECIFIED.)
CURVE()
GEOMETRIC_REPRESENTATION_ITEM()
RATIONAL_B_SPLINE_CURVE((1.,1.02342774714042,1.01603499393247))
REPRESENTATION_ITEM('')
);
#235=(
BOUNDED_CURVE()
B_SPLINE_CURVE(2,(#39858,#39859,#39860),.UNSPECIFIED.,.F.,.F.)
B_SPLINE_CURVE_WITH_KNOTS((3,3),(0.0560176289802603,0.163687850794567),
 .UNSPECIFIED.)
CURVE()
GEOMETRIC_REPRESENTATION_ITEM()
RATIONAL_B_SPLINE_CURVE((1.01603499393247,1.02342774714041,1.))
REPRESENTATION_ITEM('')
);
#236=(
BOUNDED_CURVE()
B_SPLINE_CURVE(2,(#39862,#39863,#39864),.UNSPECIFIED.,.F.,.F.)
B_SPLINE_CURVE_WITH_KNOTS((3,3),(0.,0.107670221814307),.UNSPECIFIED.)
CURVE()
GEOMETRIC_REPRESENTATION_ITEM()
RATIONAL_B_SPLINE_CURVE((1.,1.02342774714042,1.01603499393247))
REPRESENTATION_ITEM('')
);
#237=(
BOUNDED_CURVE()
B_SPLINE_CURVE(2,(#39869,#39870,#39871),.UNSPECIFIED.,.F.,.F.)
B_SPLINE_CURVE_WITH_KNOTS((3,3),(0.,0.107670221814307),.UNSPECIFIED.)
CURVE()
GEOMETRIC_REPRESENTATION_ITEM()
RATIONAL_B_SPLINE_CURVE((1.,1.02342774714043,1.01603499393248))
REPRESENTATION_ITEM('')
);
#238=(
BOUNDED_CURVE()
B_SPLINE_CURVE(2,(#39874,#39875,#39876),.UNSPECIFIED.,.F.,.F.)
B_SPLINE_CURVE_WITH_KNOTS((3,3),(0.0560176289802603,0.163687850794567),
 .UNSPECIFIED.)
CURVE()
GEOMETRIC_REPRESENTATION_ITEM()
RATIONAL_B_SPLINE_CURVE((1.01603499393247,1.02342774714042,1.))
REPRESENTATION_ITEM('')
);
#239=(
BOUNDED_CURVE()
B_SPLINE_CURVE(2,(#39881,#39882,#39883),.UNSPECIFIED.,.F.,.F.)
B_SPLINE_CURVE_WITH_KNOTS((3,3),(0.0560176289802605,0.163687850794567),
 .UNSPECIFIED.)
CURVE()
GEOMETRIC_REPRESENTATION_ITEM()
RATIONAL_B_SPLINE_CURVE((1.01603499393247,1.02342774714041,1.))
REPRESENTATION_ITEM('')
);
#240=(
BOUNDED_CURVE()
B_SPLINE_CURVE(2,(#39887,#39888,#39889),.UNSPECIFIED.,.F.,.F.)
B_SPLINE_CURVE_WITH_KNOTS((3,3),(0.,0.107670221814307),.UNSPECIFIED.)
CURVE()
GEOMETRIC_REPRESENTATION_ITEM()
RATIONAL_B_SPLINE_CURVE((1.,1.02342774714041,1.01603499393247))
REPRESENTATION_ITEM('')
);
#241=(
BOUNDED_CURVE()
B_SPLINE_CURVE(2,(#39894,#39895,#39896),.UNSPECIFIED.,.F.,.F.)
B_SPLINE_CURVE_WITH_KNOTS((3,3),(0.0560176289802601,0.163687850794567),
 .UNSPECIFIED.)
CURVE()
GEOMETRIC_REPRESENTATION_ITEM()
RATIONAL_B_SPLINE_CURVE((1.01603499393247,1.02342774714041,1.))
REPRESENTATION_ITEM('')
);
#242=(
BOUNDED_CURVE()
B_SPLINE_CURVE(2,(#39900,#39901,#39902),.UNSPECIFIED.,.F.,.F.)
B_SPLINE_CURVE_WITH_KNOTS((3,3),(0.,0.107670221814307),.UNSPECIFIED.)
CURVE()
GEOMETRIC_REPRESENTATION_ITEM()
RATIONAL_B_SPLINE_CURVE((1.,1.02342774714041,1.01603499393247))
REPRESENTATION_ITEM('')
);
#243=(
BOUNDED_CURVE()
B_SPLINE_CURVE(2,(#39907,#39908,#39909),.UNSPECIFIED.,.F.,.F.)
B_SPLINE_CURVE_WITH_KNOTS((3,3),(0.0560176289802598,0.163687850794567),
 .UNSPECIFIED.)
CURVE()
GEOMETRIC_REPRESENTATION_ITEM()
RATIONAL_B_SPLINE_CURVE((1.01603499393248,1.02342774714042,1.))
REPRESENTATION_ITEM('')
);
#244=(
BOUNDED_CURVE()
B_SPLINE_CURVE(2,(#39913,#39914,#39915),.UNSPECIFIED.,.F.,.F.)
B_SPLINE_CURVE_WITH_KNOTS((3,3),(0.,0.107670221814307),.UNSPECIFIED.)
CURVE()
GEOMETRIC_REPRESENTATION_ITEM()
RATIONAL_B_SPLINE_CURVE((1.,1.02342774714041,1.01603499393247))
REPRESENTATION_ITEM('')
);
#245=(
BOUNDED_CURVE()
B_SPLINE_CURVE(2,(#39924,#39925,#39926),.UNSPECIFIED.,.F.,.F.)
B_SPLINE_CURVE_WITH_KNOTS((3,3),(0.0560176289802602,0.163687850794567),
 .UNSPECIFIED.)
CURVE()
GEOMETRIC_REPRESENTATION_ITEM()
RATIONAL_B_SPLINE_CURVE((1.01603499393248,1.02342774714042,1.))
REPRESENTATION_ITEM('')
);
#246=(
BOUNDED_CURVE()
B_SPLINE_CURVE(2,(#39930,#39931,#39932),.UNSPECIFIED.,.F.,.F.)
B_SPLINE_CURVE_WITH_KNOTS((3,3),(0.,0.107670221814307),.UNSPECIFIED.)
CURVE()
GEOMETRIC_REPRESENTATION_ITEM()
RATIONAL_B_SPLINE_CURVE((1.,1.02342774714041,1.01603499393247))
REPRESENTATION_ITEM('')
);
#247=(
BOUNDED_CURVE()
B_SPLINE_CURVE(2,(#39937,#39938,#39939),.UNSPECIFIED.,.F.,.F.)
B_SPLINE_CURVE_WITH_KNOTS((3,3),(0.,0.107670221814307),.UNSPECIFIED.)
CURVE()
GEOMETRIC_REPRESENTATION_ITEM()
RATIONAL_B_SPLINE_CURVE((1.,1.02342774714041,1.01603499393247))
REPRESENTATION_ITEM('')
);
#248=(
BOUNDED_CURVE()
B_SPLINE_CURVE(2,(#39942,#39943,#39944),.UNSPECIFIED.,.F.,.F.)
B_SPLINE_CURVE_WITH_KNOTS((3,3),(0.0560176289802595,0.163687850794568),
 .UNSPECIFIED.)
CURVE()
GEOMETRIC_REPRESENTATION_ITEM()
RATIONAL_B_SPLINE_CURVE((1.01603499393248,1.02342774714043,1.))
REPRESENTATION_ITEM('')
);
#249=(
BOUNDED_CURVE()
B_SPLINE_CURVE(2,(#39948,#39949,#39950),.UNSPECIFIED.,.F.,.F.)
B_SPLINE_CURVE_WITH_KNOTS((3,3),(0.05601762898026,0.163687850794567),
 .UNSPECIFIED.)
CURVE()
GEOMETRIC_REPRESENTATION_ITEM()
RATIONAL_B_SPLINE_CURVE((1.01603499393247,1.02342774714041,1.))
REPRESENTATION_ITEM('')
);
#250=(
BOUNDED_CURVE()
B_SPLINE_CURVE(2,(#39959,#39960,#39961),.UNSPECIFIED.,.F.,.F.)
B_SPLINE_CURVE_WITH_KNOTS((3,3),(0.,0.107670221814308),.UNSPECIFIED.)
CURVE()
GEOMETRIC_REPRESENTATION_ITEM()
RATIONAL_B_SPLINE_CURVE((1.,1.02342774714044,1.01603499393249))
REPRESENTATION_ITEM('')
);
#251=(
BOUNDED_CURVE()
B_SPLINE_CURVE(2,(#43783,#43784,#43785),.UNSPECIFIED.,.F.,.F.)
B_SPLINE_CURVE_WITH_KNOTS((3,3),(0.,0.00841282944278042),.UNSPECIFIED.)
CURVE()
GEOMETRIC_REPRESENTATION_ITEM()
RATIONAL_B_SPLINE_CURVE((1.,1.00035365746955,1.00043184882983))
REPRESENTATION_ITEM('')
);
#252=(
BOUNDED_CURVE()
B_SPLINE_CURVE(2,(#43789,#43790,#43791),.UNSPECIFIED.,.F.,.F.)
B_SPLINE_CURVE_WITH_KNOTS((3,3),(0.0131888113576721,0.0216016408002996),
 .UNSPECIFIED.)
CURVE()
GEOMETRIC_REPRESENTATION_ITEM()
RATIONAL_B_SPLINE_CURVE((1.00043184882948,1.00035365746926,1.))
REPRESENTATION_ITEM('')
);
#253=(
BOUNDED_CURVE()
B_SPLINE_CURVE(2,(#43804,#43805,#43806),.UNSPECIFIED.,.F.,.F.)
B_SPLINE_CURVE_WITH_KNOTS((3,3),(0.,0.0084128294426201),.UNSPECIFIED.)
CURVE()
GEOMETRIC_REPRESENTATION_ITEM()
RATIONAL_B_SPLINE_CURVE((1.,1.00035365746986,1.00043184883023))
REPRESENTATION_ITEM('')
);
#254=(
BOUNDED_CURVE()
B_SPLINE_CURVE(2,(#43810,#43811,#43812),.UNSPECIFIED.,.F.,.F.)
B_SPLINE_CURVE_WITH_KNOTS((3,3),(0.0131888113575809,0.0216016408002996),
 .UNSPECIFIED.)
CURVE()
GEOMETRIC_REPRESENTATION_ITEM()
RATIONAL_B_SPLINE_CURVE((1.00043184883059,1.00035365747017,1.))
REPRESENTATION_ITEM('')
);
#255=(
BOUNDED_CURVE()
B_SPLINE_CURVE(2,(#43825,#43826,#43827),.UNSPECIFIED.,.F.,.F.)
B_SPLINE_CURVE_WITH_KNOTS((3,3),(0.,0.00841282944278058),.UNSPECIFIED.)
CURVE()
GEOMETRIC_REPRESENTATION_ITEM()
RATIONAL_B_SPLINE_CURVE((1.,1.00035365746906,1.00043184882924))
REPRESENTATION_ITEM('')
);
#256=(
BOUNDED_CURVE()
B_SPLINE_CURVE(2,(#43831,#43832,#43833),.UNSPECIFIED.,.F.,.F.)
B_SPLINE_CURVE_WITH_KNOTS((3,3),(0.0131888113576548,0.0216016408002996),
 .UNSPECIFIED.)
CURVE()
GEOMETRIC_REPRESENTATION_ITEM()
RATIONAL_B_SPLINE_CURVE((1.00043184882846,1.00035365746842,1.))
REPRESENTATION_ITEM('')
);
#257=(
BOUNDED_CURVE()
B_SPLINE_CURVE(2,(#43846,#43847,#43848),.UNSPECIFIED.,.F.,.F.)
B_SPLINE_CURVE_WITH_KNOTS((3,3),(0.,0.00841282944280584),.UNSPECIFIED.)
CURVE()
GEOMETRIC_REPRESENTATION_ITEM()
RATIONAL_B_SPLINE_CURVE((1.,1.00035365746775,1.00043184882763))
REPRESENTATION_ITEM('')
);
#258=(
BOUNDED_CURVE()
B_SPLINE_CURVE(2,(#43852,#43853,#43854),.UNSPECIFIED.,.F.,.F.)
B_SPLINE_CURVE_WITH_KNOTS((3,3),(0.0131888113576015,0.0216016408002996),
 .UNSPECIFIED.)
CURVE()
GEOMETRIC_REPRESENTATION_ITEM()
RATIONAL_B_SPLINE_CURVE((1.00043184882681,1.00035365746707,1.))
REPRESENTATION_ITEM('')
);
#259=(
BOUNDED_CURVE()
B_SPLINE_CURVE(2,(#43867,#43868,#43869),.UNSPECIFIED.,.F.,.F.)
B_SPLINE_CURVE_WITH_KNOTS((3,3),(0.,0.00841282944278488),.UNSPECIFIED.)
CURVE()
GEOMETRIC_REPRESENTATION_ITEM()
RATIONAL_B_SPLINE_CURVE((1.,1.0003536574676,1.00043184882745))
REPRESENTATION_ITEM('')
);
#260=(
BOUNDED_CURVE()
B_SPLINE_CURVE(2,(#43873,#43874,#43875),.UNSPECIFIED.,.F.,.F.)
B_SPLINE_CURVE_WITH_KNOTS((3,3),(0.0131888113575949,0.0216016408002996),
 .UNSPECIFIED.)
CURVE()
GEOMETRIC_REPRESENTATION_ITEM()
RATIONAL_B_SPLINE_CURVE((1.000431848828,1.00035365746804,1.))
REPRESENTATION_ITEM('')
);
#261=(
BOUNDED_CURVE()
B_SPLINE_CURVE(2,(#43888,#43889,#43890),.UNSPECIFIED.,.F.,.F.)
B_SPLINE_CURVE_WITH_KNOTS((3,3),(0.,0.00841282944265237),.UNSPECIFIED.)
CURVE()
GEOMETRIC_REPRESENTATION_ITEM()
RATIONAL_B_SPLINE_CURVE((1.,1.00035365746874,1.00043184882885))
REPRESENTATION_ITEM('')
);
#262=(
BOUNDED_CURVE()
B_SPLINE_CURVE(2,(#43894,#43895,#43896),.UNSPECIFIED.,.F.,.F.)
B_SPLINE_CURVE_WITH_KNOTS((3,3),(0.0131888113575151,0.0216016408002996),
 .UNSPECIFIED.)
CURVE()
GEOMETRIC_REPRESENTATION_ITEM()
RATIONAL_B_SPLINE_CURVE((1.00043184882745,1.0003536574676,1.))
REPRESENTATION_ITEM('')
);
#263=(
BOUNDED_CURVE()
B_SPLINE_CURVE(2,(#43909,#43910,#43911),.UNSPECIFIED.,.F.,.F.)
B_SPLINE_CURVE_WITH_KNOTS((3,3),(0.,0.00841282944265245),.UNSPECIFIED.)
CURVE()
GEOMETRIC_REPRESENTATION_ITEM()
RATIONAL_B_SPLINE_CURVE((1.,1.00035365746621,1.00043184882576))
REPRESENTATION_ITEM('')
);
#264=(
BOUNDED_CURVE()
B_SPLINE_CURVE(2,(#43915,#43916,#43917),.UNSPECIFIED.,.F.,.F.)
B_SPLINE_CURVE_WITH_KNOTS((3,3),(0.013188811357676,0.0216016408002996),
 .UNSPECIFIED.)
CURVE()
GEOMETRIC_REPRESENTATION_ITEM()
RATIONAL_B_SPLINE_CURVE((1.00043184882966,1.0003536574694,1.))
REPRESENTATION_ITEM('')
);
#265=(
BOUNDED_CURVE()
B_SPLINE_CURVE(2,(#43930,#43931,#43932),.UNSPECIFIED.,.F.,.F.)
B_SPLINE_CURVE_WITH_KNOTS((3,3),(0.,0.00841282944263587),.UNSPECIFIED.)
CURVE()
GEOMETRIC_REPRESENTATION_ITEM()
RATIONAL_B_SPLINE_CURVE((1.,1.00035365746699,1.00043184882672))
REPRESENTATION_ITEM('')
);
#266=(
BOUNDED_CURVE()
B_SPLINE_CURVE(2,(#43936,#43937,#43938),.UNSPECIFIED.,.F.,.F.)
B_SPLINE_CURVE_WITH_KNOTS((3,3),(0.0131888113575321,0.0216016408002996),
 .UNSPECIFIED.)
CURVE()
GEOMETRIC_REPRESENTATION_ITEM()
RATIONAL_B_SPLINE_CURVE((1.00043184883015,1.00035365746981,1.))
REPRESENTATION_ITEM('')
);
#267=(
BOUNDED_CURVE()
B_SPLINE_CURVE(2,(#43951,#43952,#43953),.UNSPECIFIED.,.F.,.F.)
B_SPLINE_CURVE_WITH_KNOTS((3,3),(0.,0.00841282944268715),.UNSPECIFIED.)
CURVE()
GEOMETRIC_REPRESENTATION_ITEM()
RATIONAL_B_SPLINE_CURVE((1.,1.00035365746714,1.0004318488269))
REPRESENTATION_ITEM('')
);
#268=(
BOUNDED_CURVE()
B_SPLINE_CURVE(2,(#43957,#43958,#43959),.UNSPECIFIED.,.F.,.F.)
B_SPLINE_CURVE_WITH_KNOTS((3,3),(0.0131888113576173,0.0216016408002996),
 .UNSPECIFIED.)
CURVE()
GEOMETRIC_REPRESENTATION_ITEM()
RATIONAL_B_SPLINE_CURVE((1.00043184882651,1.00035365746683,1.))
REPRESENTATION_ITEM('')
);
#269=(
BOUNDED_CURVE()
B_SPLINE_CURVE(2,(#43972,#43973,#43974),.UNSPECIFIED.,.F.,.F.)
B_SPLINE_CURVE_WITH_KNOTS((3,3),(0.,0.00841282944268232),.UNSPECIFIED.)
CURVE()
GEOMETRIC_REPRESENTATION_ITEM()
RATIONAL_B_SPLINE_CURVE((1.,1.00035365746714,1.0004318488269))
REPRESENTATION_ITEM('')
);
#270=(
BOUNDED_CURVE()
B_SPLINE_CURVE(2,(#43978,#43979,#43980),.UNSPECIFIED.,.F.,.F.)
B_SPLINE_CURVE_WITH_KNOTS((3,3),(0.0131888113576523,0.0216016408002997),
 .UNSPECIFIED.)
CURVE()
GEOMETRIC_REPRESENTATION_ITEM()
RATIONAL_B_SPLINE_CURVE((1.00043184882641,1.00035365746674,1.))
REPRESENTATION_ITEM('')
);
#271=(
BOUNDED_CURVE()
B_SPLINE_CURVE(2,(#43993,#43994,#43995),.UNSPECIFIED.,.F.,.F.)
B_SPLINE_CURVE_WITH_KNOTS((3,3),(0.,0.00841282944262782),.UNSPECIFIED.)
CURVE()
GEOMETRIC_REPRESENTATION_ITEM()
RATIONAL_B_SPLINE_CURVE((1.,1.00035365747069,1.00043184883123))
REPRESENTATION_ITEM('')
);
#272=(
BOUNDED_CURVE()
B_SPLINE_CURVE(2,(#43999,#44000,#44001),.UNSPECIFIED.,.F.,.F.)
B_SPLINE_CURVE_WITH_KNOTS((3,3),(0.0131888113575803,0.0216016408002996),
 .UNSPECIFIED.)
CURVE()
GEOMETRIC_REPRESENTATION_ITEM()
RATIONAL_B_SPLINE_CURVE((1.00043184883154,1.00035365747094,1.))
REPRESENTATION_ITEM('')
);
#273=(
BOUNDED_CURVE()
B_SPLINE_CURVE(2,(#44014,#44015,#44016),.UNSPECIFIED.,.F.,.F.)
B_SPLINE_CURVE_WITH_KNOTS((3,3),(0.,0.00841282944278058),.UNSPECIFIED.)
CURVE()
GEOMETRIC_REPRESENTATION_ITEM()
RATIONAL_B_SPLINE_CURVE((1.,1.00035365746906,1.00043184882924))
REPRESENTATION_ITEM('')
);
#274=(
BOUNDED_CURVE()
B_SPLINE_CURVE(2,(#44020,#44021,#44022),.UNSPECIFIED.,.F.,.F.)
B_SPLINE_CURVE_WITH_KNOTS((3,3),(0.0131888113576548,0.0216016408002996),
 .UNSPECIFIED.)
CURVE()
GEOMETRIC_REPRESENTATION_ITEM()
RATIONAL_B_SPLINE_CURVE((1.00043184882846,1.00035365746842,1.))
REPRESENTATION_ITEM('')
);
#275=(
BOUNDED_CURVE()
B_SPLINE_CURVE(2,(#44035,#44036,#44037),.UNSPECIFIED.,.F.,.F.)
B_SPLINE_CURVE_WITH_KNOTS((3,3),(0.,0.00841282944280138),.UNSPECIFIED.)
CURVE()
GEOMETRIC_REPRESENTATION_ITEM()
RATIONAL_B_SPLINE_CURVE((1.,1.00035365746471,1.00043184882392))
REPRESENTATION_ITEM('')
);
#276=(
BOUNDED_CURVE()
B_SPLINE_CURVE(2,(#44041,#44042,#44043),.UNSPECIFIED.,.F.,.F.)
B_SPLINE_CURVE_WITH_KNOTS((3,3),(0.0131888113575931,0.0216016408002996),
 .UNSPECIFIED.)
CURVE()
GEOMETRIC_REPRESENTATION_ITEM()
RATIONAL_B_SPLINE_CURVE((1.00043184882494,1.00035365746554,1.))
REPRESENTATION_ITEM('')
);
#277=(
BOUNDED_CURVE()
B_SPLINE_CURVE(2,(#44056,#44057,#44058),.UNSPECIFIED.,.F.,.F.)
B_SPLINE_CURVE_WITH_KNOTS((3,3),(0.,0.00841282944261464),.UNSPECIFIED.)
CURVE()
GEOMETRIC_REPRESENTATION_ITEM()
RATIONAL_B_SPLINE_CURVE((1.,1.00035365746679,1.00043184882648))
REPRESENTATION_ITEM('')
);
#278=(
BOUNDED_CURVE()
B_SPLINE_CURVE(2,(#44062,#44063,#44064),.UNSPECIFIED.,.F.,.F.)
B_SPLINE_CURVE_WITH_KNOTS((3,3),(0.0131888113575887,0.0216016408002996),
 .UNSPECIFIED.)
CURVE()
GEOMETRIC_REPRESENTATION_ITEM()
RATIONAL_B_SPLINE_CURVE((1.00043184882758,1.0003536574677,1.))
REPRESENTATION_ITEM('')
);
#279=(
BOUNDED_CURVE()
B_SPLINE_CURVE(2,(#44077,#44078,#44079),.UNSPECIFIED.,.F.,.F.)
B_SPLINE_CURVE_WITH_KNOTS((3,3),(0.,0.00841282944265251),.UNSPECIFIED.)
CURVE()
GEOMETRIC_REPRESENTATION_ITEM()
RATIONAL_B_SPLINE_CURVE((1.,1.00035365746762,1.00043184882748))
REPRESENTATION_ITEM('')
);
#280=(
BOUNDED_CURVE()
B_SPLINE_CURVE(2,(#44083,#44084,#44085),.UNSPECIFIED.,.F.,.F.)
B_SPLINE_CURVE_WITH_KNOTS((3,3),(0.0131888113576473,0.0216016408002996),
 .UNSPECIFIED.)
CURVE()
GEOMETRIC_REPRESENTATION_ITEM()
RATIONAL_B_SPLINE_CURVE((1.00043184883165,1.00035365747103,1.))
REPRESENTATION_ITEM('')
);
#281=(
BOUNDED_CURVE()
B_SPLINE_CURVE(2,(#44098,#44099,#44100),.UNSPECIFIED.,.F.,.F.)
B_SPLINE_CURVE_WITH_KNOTS((3,3),(0.,0.00841282944262983),.UNSPECIFIED.)
CURVE()
GEOMETRIC_REPRESENTATION_ITEM()
RATIONAL_B_SPLINE_CURVE((1.,1.00035365747139,1.00043184883209))
REPRESENTATION_ITEM('')
);
#282=(
BOUNDED_CURVE()
B_SPLINE_CURVE(2,(#44104,#44105,#44106),.UNSPECIFIED.,.F.,.F.)
B_SPLINE_CURVE_WITH_KNOTS((3,3),(0.0131888113576388,0.0216016408002996),
 .UNSPECIFIED.)
CURVE()
GEOMETRIC_REPRESENTATION_ITEM()
RATIONAL_B_SPLINE_CURVE((1.00043184882737,1.00035365746753,1.))
REPRESENTATION_ITEM('')
);
#283=(
BOUNDED_CURVE()
B_SPLINE_CURVE(2,(#44119,#44120,#44121),.UNSPECIFIED.,.F.,.F.)
B_SPLINE_CURVE_WITH_KNOTS((3,3),(0.,0.00841282944261306),.UNSPECIFIED.)
CURVE()
GEOMETRIC_REPRESENTATION_ITEM()
RATIONAL_B_SPLINE_CURVE((1.,1.00035365747318,1.00043184883428))
REPRESENTATION_ITEM('')
);
#284=(
BOUNDED_CURVE()
B_SPLINE_CURVE(2,(#44125,#44126,#44127),.UNSPECIFIED.,.F.,.F.)
B_SPLINE_CURVE_WITH_KNOTS((3,3),(0.0131888113575341,0.0216016408002996),
 .UNSPECIFIED.)
CURVE()
GEOMETRIC_REPRESENTATION_ITEM()
RATIONAL_B_SPLINE_CURVE((1.00043184882813,1.00035365746816,1.))
REPRESENTATION_ITEM('')
);
#285=(
BOUNDED_CURVE()
B_SPLINE_CURVE(2,(#44142,#44143,#44144),.UNSPECIFIED.,.F.,.F.)
B_SPLINE_CURVE_WITH_KNOTS((3,3),(0.,0.00841282944268199),.UNSPECIFIED.)
CURVE()
GEOMETRIC_REPRESENTATION_ITEM()
RATIONAL_B_SPLINE_CURVE((1.,1.00035365746877,1.00043184882888))
REPRESENTATION_ITEM('')
);
#286=(
BOUNDED_CURVE()
B_SPLINE_CURVE(2,(#44148,#44149,#44150),.UNSPECIFIED.,.F.,.F.)
B_SPLINE_CURVE_WITH_KNOTS((3,3),(0.0131888113576103,0.0216016408002996),
 .UNSPECIFIED.)
CURVE()
GEOMETRIC_REPRESENTATION_ITEM()
RATIONAL_B_SPLINE_CURVE((1.00043184882915,1.00035365746898,1.))
REPRESENTATION_ITEM('')
);
#287=(
BOUNDED_CURVE()
B_SPLINE_CURVE(2,(#44163,#44164,#44165),.UNSPECIFIED.,.F.,.F.)
B_SPLINE_CURVE_WITH_KNOTS((3,3),(0.,0.00841282944276111),.UNSPECIFIED.)
CURVE()
GEOMETRIC_REPRESENTATION_ITEM()
RATIONAL_B_SPLINE_CURVE((1.,1.00035365746789,1.00043184882782))
REPRESENTATION_ITEM('')
);
#288=(
BOUNDED_CURVE()
B_SPLINE_CURVE(2,(#44169,#44170,#44171),.UNSPECIFIED.,.F.,.F.)
B_SPLINE_CURVE_WITH_KNOTS((3,3),(0.013188811357663,0.0216016408002997),
 .UNSPECIFIED.)
CURVE()
GEOMETRIC_REPRESENTATION_ITEM()
RATIONAL_B_SPLINE_CURVE((1.00043184882852,1.00035365746847,1.))
REPRESENTATION_ITEM('')
);
#289=(
BOUNDED_CURVE()
B_SPLINE_CURVE(2,(#44184,#44185,#44186),.UNSPECIFIED.,.F.,.F.)
B_SPLINE_CURVE_WITH_KNOTS((3,3),(0.,0.00841282944263208),.UNSPECIFIED.)
CURVE()
GEOMETRIC_REPRESENTATION_ITEM()
RATIONAL_B_SPLINE_CURVE((1.,1.00035365746816,1.00043184882815))
REPRESENTATION_ITEM('')
);
#290=(
BOUNDED_CURVE()
B_SPLINE_CURVE(2,(#44190,#44191,#44192),.UNSPECIFIED.,.F.,.F.)
B_SPLINE_CURVE_WITH_KNOTS((3,3),(0.013188811357748,0.0216016408002996),
 .UNSPECIFIED.)
CURVE()
GEOMETRIC_REPRESENTATION_ITEM()
RATIONAL_B_SPLINE_CURVE((1.00043184883132,1.00035365747076,1.))
REPRESENTATION_ITEM('')
);
#291=(
BOUNDED_CURVE()
B_SPLINE_CURVE(2,(#44205,#44206,#44207),.UNSPECIFIED.,.F.,.F.)
B_SPLINE_CURVE_WITH_KNOTS((3,3),(0.,0.00841282944264326),.UNSPECIFIED.)
CURVE()
GEOMETRIC_REPRESENTATION_ITEM()
RATIONAL_B_SPLINE_CURVE((1.,1.00035365746759,1.00043184882744))
REPRESENTATION_ITEM('')
);
#292=(
BOUNDED_CURVE()
B_SPLINE_CURVE(2,(#44211,#44212,#44213),.UNSPECIFIED.,.F.,.F.)
B_SPLINE_CURVE_WITH_KNOTS((3,3),(0.0131888113575487,0.0216016408002996),
 .UNSPECIFIED.)
CURVE()
GEOMETRIC_REPRESENTATION_ITEM()
RATIONAL_B_SPLINE_CURVE((1.0004318488259,1.00035365746632,1.))
REPRESENTATION_ITEM('')
);
#293=(
BOUNDED_CURVE()
B_SPLINE_CURVE(2,(#44226,#44227,#44228),.UNSPECIFIED.,.F.,.F.)
B_SPLINE_CURVE_WITH_KNOTS((3,3),(0.,0.00841282944280138),.UNSPECIFIED.)
CURVE()
GEOMETRIC_REPRESENTATION_ITEM()
RATIONAL_B_SPLINE_CURVE((1.,1.00035365746471,1.00043184882392))
REPRESENTATION_ITEM('')
);
#294=(
BOUNDED_CURVE()
B_SPLINE_CURVE(2,(#44232,#44233,#44234),.UNSPECIFIED.,.F.,.F.)
B_SPLINE_CURVE_WITH_KNOTS((3,3),(0.0131888113575931,0.0216016408002996),
 .UNSPECIFIED.)
CURVE()
GEOMETRIC_REPRESENTATION_ITEM()
RATIONAL_B_SPLINE_CURVE((1.00043184882494,1.00035365746554,1.))
REPRESENTATION_ITEM('')
);
#295=(
BOUNDED_CURVE()
B_SPLINE_CURVE(2,(#44247,#44248,#44249),.UNSPECIFIED.,.F.,.F.)
B_SPLINE_CURVE_WITH_KNOTS((3,3),(0.,0.00841282944270105),.UNSPECIFIED.)
CURVE()
GEOMETRIC_REPRESENTATION_ITEM()
RATIONAL_B_SPLINE_CURVE((1.,1.000353657467,1.00043184882673))
REPRESENTATION_ITEM('')
);
#296=(
BOUNDED_CURVE()
B_SPLINE_CURVE(2,(#44253,#44254,#44255),.UNSPECIFIED.,.F.,.F.)
B_SPLINE_CURVE_WITH_KNOTS((3,3),(0.0131888113574971,0.0216016408002996),
 .UNSPECIFIED.)
CURVE()
GEOMETRIC_REPRESENTATION_ITEM()
RATIONAL_B_SPLINE_CURVE((1.00043184882773,1.00035365746783,1.))
REPRESENTATION_ITEM('')
);
#297=(
BOUNDED_CURVE()
B_SPLINE_CURVE(2,(#44268,#44269,#44270),.UNSPECIFIED.,.F.,.F.)
B_SPLINE_CURVE_WITH_KNOTS((3,3),(0.,0.00841282944264652),.UNSPECIFIED.)
CURVE()
GEOMETRIC_REPRESENTATION_ITEM()
RATIONAL_B_SPLINE_CURVE((1.,1.00035365746972,1.00043184883004))
REPRESENTATION_ITEM('')
);
#298=(
BOUNDED_CURVE()
B_SPLINE_CURVE(2,(#44274,#44275,#44276),.UNSPECIFIED.,.F.,.F.)
B_SPLINE_CURVE_WITH_KNOTS((3,3),(0.0131888113576371,0.0216016408002996),
 .UNSPECIFIED.)
CURVE()
GEOMETRIC_REPRESENTATION_ITEM()
RATIONAL_B_SPLINE_CURVE((1.00043184882659,1.00035365746689,1.))
REPRESENTATION_ITEM('')
);
#299=(
BOUNDED_CURVE()
B_SPLINE_CURVE(2,(#44289,#44290,#44291),.UNSPECIFIED.,.F.,.F.)
B_SPLINE_CURVE_WITH_KNOTS((3,3),(0.,0.00841282944262983),.UNSPECIFIED.)
CURVE()
GEOMETRIC_REPRESENTATION_ITEM()
RATIONAL_B_SPLINE_CURVE((1.,1.00035365747139,1.00043184883209))
REPRESENTATION_ITEM('')
);
#300=(
BOUNDED_CURVE()
B_SPLINE_CURVE(2,(#44295,#44296,#44297),.UNSPECIFIED.,.F.,.F.)
B_SPLINE_CURVE_WITH_KNOTS((3,3),(0.0131888113576388,0.0216016408002996),
 .UNSPECIFIED.)
CURVE()
GEOMETRIC_REPRESENTATION_ITEM()
RATIONAL_B_SPLINE_CURVE((1.00043184882737,1.00035365746753,1.))
REPRESENTATION_ITEM('')
);
#301=(
BOUNDED_CURVE()
B_SPLINE_CURVE(2,(#44310,#44311,#44312),.UNSPECIFIED.,.F.,.F.)
B_SPLINE_CURVE_WITH_KNOTS((3,3),(0.,0.00841282944264003),.UNSPECIFIED.)
CURVE()
GEOMETRIC_REPRESENTATION_ITEM()
RATIONAL_B_SPLINE_CURVE((1.,1.0003536574673,1.00043184882709))
REPRESENTATION_ITEM('')
);
#302=(
BOUNDED_CURVE()
B_SPLINE_CURVE(2,(#44316,#44317,#44318),.UNSPECIFIED.,.F.,.F.)
B_SPLINE_CURVE_WITH_KNOTS((3,3),(0.0131888113576155,0.0216016408002996),
 .UNSPECIFIED.)
CURVE()
GEOMETRIC_REPRESENTATION_ITEM()
RATIONAL_B_SPLINE_CURVE((1.00043184882608,1.00035365746647,1.))
REPRESENTATION_ITEM('')
);
#303=(
BOUNDED_CURVE()
B_SPLINE_CURVE(2,(#44331,#44332,#44333),.UNSPECIFIED.,.F.,.F.)
B_SPLINE_CURVE_WITH_KNOTS((3,3),(0.,0.00841282944269557),.UNSPECIFIED.)
CURVE()
GEOMETRIC_REPRESENTATION_ITEM()
RATIONAL_B_SPLINE_CURVE((1.,1.00035365746722,1.000431848827))
REPRESENTATION_ITEM('')
);
#304=(
BOUNDED_CURVE()
B_SPLINE_CURVE(2,(#44337,#44338,#44339),.UNSPECIFIED.,.F.,.F.)
B_SPLINE_CURVE_WITH_KNOTS((3,3),(0.0131888113576143,0.0216016408002996),
 .UNSPECIFIED.)
CURVE()
GEOMETRIC_REPRESENTATION_ITEM()
RATIONAL_B_SPLINE_CURVE((1.00043184882947,1.00035365746925,1.))
REPRESENTATION_ITEM('')
);
#305=(
BOUNDED_CURVE()
B_SPLINE_CURVE(2,(#44352,#44353,#44354),.UNSPECIFIED.,.F.,.F.)
B_SPLINE_CURVE_WITH_KNOTS((3,3),(0.,0.00841282944278065),.UNSPECIFIED.)
CURVE()
GEOMETRIC_REPRESENTATION_ITEM()
RATIONAL_B_SPLINE_CURVE((1.,1.00035365746947,1.00043184882974))
REPRESENTATION_ITEM('')
);
#306=(
BOUNDED_CURVE()
B_SPLINE_CURVE(2,(#44358,#44359,#44360),.UNSPECIFIED.,.F.,.F.)
B_SPLINE_CURVE_WITH_KNOTS((3,3),(0.0131888113576697,0.0216016408002996),
 .UNSPECIFIED.)
CURVE()
GEOMETRIC_REPRESENTATION_ITEM()
RATIONAL_B_SPLINE_CURVE((1.00043184882899,1.00035365746886,1.))
REPRESENTATION_ITEM('')
);
#307=(
BOUNDED_CURVE()
B_SPLINE_CURVE(2,(#44373,#44374,#44375),.UNSPECIFIED.,.F.,.F.)
B_SPLINE_CURVE_WITH_KNOTS((3,3),(0.,0.00841282944263208),.UNSPECIFIED.)
CURVE()
GEOMETRIC_REPRESENTATION_ITEM()
RATIONAL_B_SPLINE_CURVE((1.,1.00035365746816,1.00043184882815))
REPRESENTATION_ITEM('')
);
#308=(
BOUNDED_CURVE()
B_SPLINE_CURVE(2,(#44379,#44380,#44381),.UNSPECIFIED.,.F.,.F.)
B_SPLINE_CURVE_WITH_KNOTS((3,3),(0.013188811357748,0.0216016408002996),
 .UNSPECIFIED.)
CURVE()
GEOMETRIC_REPRESENTATION_ITEM()
RATIONAL_B_SPLINE_CURVE((1.00043184883132,1.00035365747076,1.))
REPRESENTATION_ITEM('')
);
#309=(
BOUNDED_CURVE()
B_SPLINE_CURVE(2,(#44394,#44395,#44396),.UNSPECIFIED.,.F.,.F.)
B_SPLINE_CURVE_WITH_KNOTS((3,3),(0.,0.00841282944273455),.UNSPECIFIED.)
CURVE()
GEOMETRIC_REPRESENTATION_ITEM()
RATIONAL_B_SPLINE_CURVE((1.,1.00035365746539,1.00043184882476))
REPRESENTATION_ITEM('')
);
#310=(
BOUNDED_CURVE()
B_SPLINE_CURVE(2,(#44400,#44401,#44402),.UNSPECIFIED.,.F.,.F.)
B_SPLINE_CURVE_WITH_KNOTS((3,3),(0.0131888113576539,0.0216016408002996),
 .UNSPECIFIED.)
CURVE()
GEOMETRIC_REPRESENTATION_ITEM()
RATIONAL_B_SPLINE_CURVE((1.00043184882929,1.0003536574691,1.))
REPRESENTATION_ITEM('')
);
#311=(
BOUNDED_CURVE()
B_SPLINE_CURVE(2,(#44415,#44416,#44417),.UNSPECIFIED.,.F.,.F.)
B_SPLINE_CURVE_WITH_KNOTS((3,3),(0.,0.00841282944270133),.UNSPECIFIED.)
CURVE()
GEOMETRIC_REPRESENTATION_ITEM()
RATIONAL_B_SPLINE_CURVE((1.,1.00035365747008,1.00043184883048))
REPRESENTATION_ITEM('')
);
#312=(
BOUNDED_CURVE()
B_SPLINE_CURVE(2,(#44421,#44422,#44423),.UNSPECIFIED.,.F.,.F.)
B_SPLINE_CURVE_WITH_KNOTS((3,3),(0.0131888113576197,0.0216016408002996),
 .UNSPECIFIED.)
CURVE()
GEOMETRIC_REPRESENTATION_ITEM()
RATIONAL_B_SPLINE_CURVE((1.00043184882798,1.00035365746803,1.))
REPRESENTATION_ITEM('')
);
#313=(
BOUNDED_CURVE()
B_SPLINE_CURVE(2,(#44436,#44437,#44438),.UNSPECIFIED.,.F.,.F.)
B_SPLINE_CURVE_WITH_KNOTS((3,3),(0.,0.00841282944261464),.UNSPECIFIED.)
CURVE()
GEOMETRIC_REPRESENTATION_ITEM()
RATIONAL_B_SPLINE_CURVE((1.,1.00035365746679,1.00043184882648))
REPRESENTATION_ITEM('')
);
#314=(
BOUNDED_CURVE()
B_SPLINE_CURVE(2,(#44442,#44443,#44444),.UNSPECIFIED.,.F.,.F.)
B_SPLINE_CURVE_WITH_KNOTS((3,3),(0.0131888113575887,0.0216016408002996),
 .UNSPECIFIED.)
CURVE()
GEOMETRIC_REPRESENTATION_ITEM()
RATIONAL_B_SPLINE_CURVE((1.00043184882758,1.0003536574677,1.))
REPRESENTATION_ITEM('')
);
#315=(
BOUNDED_CURVE()
B_SPLINE_CURVE(2,(#44457,#44458,#44459),.UNSPECIFIED.,.F.,.F.)
B_SPLINE_CURVE_WITH_KNOTS((3,3),(0.,0.00841282944264924),.UNSPECIFIED.)
CURVE()
GEOMETRIC_REPRESENTATION_ITEM()
RATIONAL_B_SPLINE_CURVE((1.,1.00035365746952,1.00043184882981))
REPRESENTATION_ITEM('')
);
#316=(
BOUNDED_CURVE()
B_SPLINE_CURVE(2,(#44463,#44464,#44465),.UNSPECIFIED.,.F.,.F.)
B_SPLINE_CURVE_WITH_KNOTS((3,3),(0.0131888113576407,0.0216016408002996),
 .UNSPECIFIED.)
CURVE()
GEOMETRIC_REPRESENTATION_ITEM()
RATIONAL_B_SPLINE_CURVE((1.00043184882821,1.00035365746821,1.))
REPRESENTATION_ITEM('')
);
#317=(
BOUNDED_CURVE()
B_SPLINE_CURVE(2,(#44478,#44479,#44480),.UNSPECIFIED.,.F.,.F.)
B_SPLINE_CURVE_WITH_KNOTS((3,3),(0.,0.00841282944262983),.UNSPECIFIED.)
CURVE()
GEOMETRIC_REPRESENTATION_ITEM()
RATIONAL_B_SPLINE_CURVE((1.,1.00035365747139,1.00043184883209))
REPRESENTATION_ITEM('')
);
#318=(
BOUNDED_CURVE()
B_SPLINE_CURVE(2,(#44484,#44485,#44486),.UNSPECIFIED.,.F.,.F.)
B_SPLINE_CURVE_WITH_KNOTS((3,3),(0.0131888113576388,0.0216016408002996),
 .UNSPECIFIED.)
CURVE()
GEOMETRIC_REPRESENTATION_ITEM()
RATIONAL_B_SPLINE_CURVE((1.00043184882737,1.00035365746753,1.))
REPRESENTATION_ITEM('')
);
#319=(
BOUNDED_CURVE()
B_SPLINE_CURVE(2,(#44499,#44500,#44501),.UNSPECIFIED.,.F.,.F.)
B_SPLINE_CURVE_WITH_KNOTS((3,3),(0.,0.0084128294426321),.UNSPECIFIED.)
CURVE()
GEOMETRIC_REPRESENTATION_ITEM()
RATIONAL_B_SPLINE_CURVE((1.,1.00035365746883,1.00043184882896))
REPRESENTATION_ITEM('')
);
#320=(
BOUNDED_CURVE()
B_SPLINE_CURVE(2,(#44505,#44506,#44507),.UNSPECIFIED.,.F.,.F.)
B_SPLINE_CURVE_WITH_KNOTS((3,3),(0.0131888113575073,0.0216016408002996),
 .UNSPECIFIED.)
CURVE()
GEOMETRIC_REPRESENTATION_ITEM()
RATIONAL_B_SPLINE_CURVE((1.00043184882395,1.00035365746473,1.))
REPRESENTATION_ITEM('')
);
#321=(
BOUNDED_CURVE()
B_SPLINE_CURVE(2,(#44560,#44561,#44562),.UNSPECIFIED.,.F.,.F.)
B_SPLINE_CURVE_WITH_KNOTS((3,3),(0.,0.00841282944285724),.UNSPECIFIED.)
CURVE()
GEOMETRIC_REPRESENTATION_ITEM()
RATIONAL_B_SPLINE_CURVE((1.,1.00035365746964,1.00043184882994))
REPRESENTATION_ITEM('')
);
#322=(
BOUNDED_CURVE()
B_SPLINE_CURVE(2,(#44564,#44565,#44566),.UNSPECIFIED.,.F.,.F.)
B_SPLINE_CURVE_WITH_KNOTS((3,3),(0.0131888113574265,0.0216016408002996),
 .UNSPECIFIED.)
CURVE()
GEOMETRIC_REPRESENTATION_ITEM()
RATIONAL_B_SPLINE_CURVE((1.00043184882266,1.00035365746368,1.))
REPRESENTATION_ITEM('')
);
#323=(
BOUNDED_CURVE()
B_SPLINE_CURVE(2,(#47824,#47825,#47826),.UNSPECIFIED.,.F.,.F.)
B_SPLINE_CURVE_WITH_KNOTS((3,3),(0.,0.00841282944278042),.UNSPECIFIED.)
CURVE()
GEOMETRIC_REPRESENTATION_ITEM()
RATIONAL_B_SPLINE_CURVE((1.,1.00035365746955,1.00043184882983))
REPRESENTATION_ITEM('')
);
#324=(
BOUNDED_CURVE()
B_SPLINE_CURVE(2,(#47830,#47831,#47832),.UNSPECIFIED.,.F.,.F.)
B_SPLINE_CURVE_WITH_KNOTS((3,3),(0.0131888113576721,0.0216016408002996),
 .UNSPECIFIED.)
CURVE()
GEOMETRIC_REPRESENTATION_ITEM()
RATIONAL_B_SPLINE_CURVE((1.00043184882948,1.00035365746926,1.))
REPRESENTATION_ITEM('')
);
#325=(
BOUNDED_CURVE()
B_SPLINE_CURVE(2,(#47845,#47846,#47847),.UNSPECIFIED.,.F.,.F.)
B_SPLINE_CURVE_WITH_KNOTS((3,3),(0.,0.0084128294426201),.UNSPECIFIED.)
CURVE()
GEOMETRIC_REPRESENTATION_ITEM()
RATIONAL_B_SPLINE_CURVE((1.,1.00035365746986,1.00043184883023))
REPRESENTATION_ITEM('')
);
#326=(
BOUNDED_CURVE()
B_SPLINE_CURVE(2,(#47851,#47852,#47853),.UNSPECIFIED.,.F.,.F.)
B_SPLINE_CURVE_WITH_KNOTS((3,3),(0.0131888113575809,0.0216016408002996),
 .UNSPECIFIED.)
CURVE()
GEOMETRIC_REPRESENTATION_ITEM()
RATIONAL_B_SPLINE_CURVE((1.00043184883059,1.00035365747017,1.))
REPRESENTATION_ITEM('')
);
#327=(
BOUNDED_CURVE()
B_SPLINE_CURVE(2,(#47866,#47867,#47868),.UNSPECIFIED.,.F.,.F.)
B_SPLINE_CURVE_WITH_KNOTS((3,3),(0.,0.00841282944278058),.UNSPECIFIED.)
CURVE()
GEOMETRIC_REPRESENTATION_ITEM()
RATIONAL_B_SPLINE_CURVE((1.,1.00035365746906,1.00043184882924))
REPRESENTATION_ITEM('')
);
#328=(
BOUNDED_CURVE()
B_SPLINE_CURVE(2,(#47872,#47873,#47874),.UNSPECIFIED.,.F.,.F.)
B_SPLINE_CURVE_WITH_KNOTS((3,3),(0.0131888113576548,0.0216016408002996),
 .UNSPECIFIED.)
CURVE()
GEOMETRIC_REPRESENTATION_ITEM()
RATIONAL_B_SPLINE_CURVE((1.00043184882846,1.00035365746842,1.))
REPRESENTATION_ITEM('')
);
#329=(
BOUNDED_CURVE()
B_SPLINE_CURVE(2,(#47887,#47888,#47889),.UNSPECIFIED.,.F.,.F.)
B_SPLINE_CURVE_WITH_KNOTS((3,3),(0.,0.00841282944280584),.UNSPECIFIED.)
CURVE()
GEOMETRIC_REPRESENTATION_ITEM()
RATIONAL_B_SPLINE_CURVE((1.,1.00035365746775,1.00043184882763))
REPRESENTATION_ITEM('')
);
#330=(
BOUNDED_CURVE()
B_SPLINE_CURVE(2,(#47893,#47894,#47895),.UNSPECIFIED.,.F.,.F.)
B_SPLINE_CURVE_WITH_KNOTS((3,3),(0.0131888113576015,0.0216016408002996),
 .UNSPECIFIED.)
CURVE()
GEOMETRIC_REPRESENTATION_ITEM()
RATIONAL_B_SPLINE_CURVE((1.00043184882681,1.00035365746707,1.))
REPRESENTATION_ITEM('')
);
#331=(
BOUNDED_CURVE()
B_SPLINE_CURVE(2,(#47908,#47909,#47910),.UNSPECIFIED.,.F.,.F.)
B_SPLINE_CURVE_WITH_KNOTS((3,3),(0.,0.00841282944278488),.UNSPECIFIED.)
CURVE()
GEOMETRIC_REPRESENTATION_ITEM()
RATIONAL_B_SPLINE_CURVE((1.,1.0003536574676,1.00043184882745))
REPRESENTATION_ITEM('')
);
#332=(
BOUNDED_CURVE()
B_SPLINE_CURVE(2,(#47914,#47915,#47916),.UNSPECIFIED.,.F.,.F.)
B_SPLINE_CURVE_WITH_KNOTS((3,3),(0.0131888113575949,0.0216016408002996),
 .UNSPECIFIED.)
CURVE()
GEOMETRIC_REPRESENTATION_ITEM()
RATIONAL_B_SPLINE_CURVE((1.000431848828,1.00035365746804,1.))
REPRESENTATION_ITEM('')
);
#333=(
BOUNDED_CURVE()
B_SPLINE_CURVE(2,(#47929,#47930,#47931),.UNSPECIFIED.,.F.,.F.)
B_SPLINE_CURVE_WITH_KNOTS((3,3),(0.,0.00841282944265237),.UNSPECIFIED.)
CURVE()
GEOMETRIC_REPRESENTATION_ITEM()
RATIONAL_B_SPLINE_CURVE((1.,1.00035365746874,1.00043184882885))
REPRESENTATION_ITEM('')
);
#334=(
BOUNDED_CURVE()
B_SPLINE_CURVE(2,(#47935,#47936,#47937),.UNSPECIFIED.,.F.,.F.)
B_SPLINE_CURVE_WITH_KNOTS((3,3),(0.0131888113575151,0.0216016408002996),
 .UNSPECIFIED.)
CURVE()
GEOMETRIC_REPRESENTATION_ITEM()
RATIONAL_B_SPLINE_CURVE((1.00043184882745,1.0003536574676,1.))
REPRESENTATION_ITEM('')
);
#335=(
BOUNDED_CURVE()
B_SPLINE_CURVE(2,(#47950,#47951,#47952),.UNSPECIFIED.,.F.,.F.)
B_SPLINE_CURVE_WITH_KNOTS((3,3),(0.,0.00841282944265245),.UNSPECIFIED.)
CURVE()
GEOMETRIC_REPRESENTATION_ITEM()
RATIONAL_B_SPLINE_CURVE((1.,1.00035365746621,1.00043184882576))
REPRESENTATION_ITEM('')
);
#336=(
BOUNDED_CURVE()
B_SPLINE_CURVE(2,(#47956,#47957,#47958),.UNSPECIFIED.,.F.,.F.)
B_SPLINE_CURVE_WITH_KNOTS((3,3),(0.013188811357676,0.0216016408002996),
 .UNSPECIFIED.)
CURVE()
GEOMETRIC_REPRESENTATION_ITEM()
RATIONAL_B_SPLINE_CURVE((1.00043184882966,1.0003536574694,1.))
REPRESENTATION_ITEM('')
);
#337=(
BOUNDED_CURVE()
B_SPLINE_CURVE(2,(#47971,#47972,#47973),.UNSPECIFIED.,.F.,.F.)
B_SPLINE_CURVE_WITH_KNOTS((3,3),(0.,0.00841282944263587),.UNSPECIFIED.)
CURVE()
GEOMETRIC_REPRESENTATION_ITEM()
RATIONAL_B_SPLINE_CURVE((1.,1.00035365746699,1.00043184882672))
REPRESENTATION_ITEM('')
);
#338=(
BOUNDED_CURVE()
B_SPLINE_CURVE(2,(#47977,#47978,#47979),.UNSPECIFIED.,.F.,.F.)
B_SPLINE_CURVE_WITH_KNOTS((3,3),(0.0131888113575321,0.0216016408002996),
 .UNSPECIFIED.)
CURVE()
GEOMETRIC_REPRESENTATION_ITEM()
RATIONAL_B_SPLINE_CURVE((1.00043184883015,1.00035365746981,1.))
REPRESENTATION_ITEM('')
);
#339=(
BOUNDED_CURVE()
B_SPLINE_CURVE(2,(#47992,#47993,#47994),.UNSPECIFIED.,.F.,.F.)
B_SPLINE_CURVE_WITH_KNOTS((3,3),(0.,0.00841282944268715),.UNSPECIFIED.)
CURVE()
GEOMETRIC_REPRESENTATION_ITEM()
RATIONAL_B_SPLINE_CURVE((1.,1.00035365746714,1.0004318488269))
REPRESENTATION_ITEM('')
);
#340=(
BOUNDED_CURVE()
B_SPLINE_CURVE(2,(#47998,#47999,#48000),.UNSPECIFIED.,.F.,.F.)
B_SPLINE_CURVE_WITH_KNOTS((3,3),(0.0131888113576173,0.0216016408002996),
 .UNSPECIFIED.)
CURVE()
GEOMETRIC_REPRESENTATION_ITEM()
RATIONAL_B_SPLINE_CURVE((1.00043184882651,1.00035365746683,1.))
REPRESENTATION_ITEM('')
);
#341=(
BOUNDED_CURVE()
B_SPLINE_CURVE(2,(#48013,#48014,#48015),.UNSPECIFIED.,.F.,.F.)
B_SPLINE_CURVE_WITH_KNOTS((3,3),(0.,0.00841282944268232),.UNSPECIFIED.)
CURVE()
GEOMETRIC_REPRESENTATION_ITEM()
RATIONAL_B_SPLINE_CURVE((1.,1.00035365746714,1.0004318488269))
REPRESENTATION_ITEM('')
);
#342=(
BOUNDED_CURVE()
B_SPLINE_CURVE(2,(#48019,#48020,#48021),.UNSPECIFIED.,.F.,.F.)
B_SPLINE_CURVE_WITH_KNOTS((3,3),(0.0131888113576523,0.0216016408002997),
 .UNSPECIFIED.)
CURVE()
GEOMETRIC_REPRESENTATION_ITEM()
RATIONAL_B_SPLINE_CURVE((1.00043184882641,1.00035365746674,1.))
REPRESENTATION_ITEM('')
);
#343=(
BOUNDED_CURVE()
B_SPLINE_CURVE(2,(#48034,#48035,#48036),.UNSPECIFIED.,.F.,.F.)
B_SPLINE_CURVE_WITH_KNOTS((3,3),(0.,0.00841282944262782),.UNSPECIFIED.)
CURVE()
GEOMETRIC_REPRESENTATION_ITEM()
RATIONAL_B_SPLINE_CURVE((1.,1.00035365747069,1.00043184883123))
REPRESENTATION_ITEM('')
);
#344=(
BOUNDED_CURVE()
B_SPLINE_CURVE(2,(#48040,#48041,#48042),.UNSPECIFIED.,.F.,.F.)
B_SPLINE_CURVE_WITH_KNOTS((3,3),(0.0131888113575803,0.0216016408002996),
 .UNSPECIFIED.)
CURVE()
GEOMETRIC_REPRESENTATION_ITEM()
RATIONAL_B_SPLINE_CURVE((1.00043184883154,1.00035365747094,1.))
REPRESENTATION_ITEM('')
);
#345=(
BOUNDED_CURVE()
B_SPLINE_CURVE(2,(#48055,#48056,#48057),.UNSPECIFIED.,.F.,.F.)
B_SPLINE_CURVE_WITH_KNOTS((3,3),(0.,0.00841282944278058),.UNSPECIFIED.)
CURVE()
GEOMETRIC_REPRESENTATION_ITEM()
RATIONAL_B_SPLINE_CURVE((1.,1.00035365746906,1.00043184882924))
REPRESENTATION_ITEM('')
);
#346=(
BOUNDED_CURVE()
B_SPLINE_CURVE(2,(#48061,#48062,#48063),.UNSPECIFIED.,.F.,.F.)
B_SPLINE_CURVE_WITH_KNOTS((3,3),(0.0131888113576548,0.0216016408002996),
 .UNSPECIFIED.)
CURVE()
GEOMETRIC_REPRESENTATION_ITEM()
RATIONAL_B_SPLINE_CURVE((1.00043184882846,1.00035365746842,1.))
REPRESENTATION_ITEM('')
);
#347=(
BOUNDED_CURVE()
B_SPLINE_CURVE(2,(#48076,#48077,#48078),.UNSPECIFIED.,.F.,.F.)
B_SPLINE_CURVE_WITH_KNOTS((3,3),(0.,0.00841282944280138),.UNSPECIFIED.)
CURVE()
GEOMETRIC_REPRESENTATION_ITEM()
RATIONAL_B_SPLINE_CURVE((1.,1.00035365746471,1.00043184882392))
REPRESENTATION_ITEM('')
);
#348=(
BOUNDED_CURVE()
B_SPLINE_CURVE(2,(#48082,#48083,#48084),.UNSPECIFIED.,.F.,.F.)
B_SPLINE_CURVE_WITH_KNOTS((3,3),(0.0131888113575931,0.0216016408002996),
 .UNSPECIFIED.)
CURVE()
GEOMETRIC_REPRESENTATION_ITEM()
RATIONAL_B_SPLINE_CURVE((1.00043184882494,1.00035365746554,1.))
REPRESENTATION_ITEM('')
);
#349=(
BOUNDED_CURVE()
B_SPLINE_CURVE(2,(#48097,#48098,#48099),.UNSPECIFIED.,.F.,.F.)
B_SPLINE_CURVE_WITH_KNOTS((3,3),(0.,0.00841282944261464),.UNSPECIFIED.)
CURVE()
GEOMETRIC_REPRESENTATION_ITEM()
RATIONAL_B_SPLINE_CURVE((1.,1.00035365746679,1.00043184882648))
REPRESENTATION_ITEM('')
);
#350=(
BOUNDED_CURVE()
B_SPLINE_CURVE(2,(#48103,#48104,#48105),.UNSPECIFIED.,.F.,.F.)
B_SPLINE_CURVE_WITH_KNOTS((3,3),(0.0131888113575887,0.0216016408002996),
 .UNSPECIFIED.)
CURVE()
GEOMETRIC_REPRESENTATION_ITEM()
RATIONAL_B_SPLINE_CURVE((1.00043184882758,1.0003536574677,1.))
REPRESENTATION_ITEM('')
);
#351=(
BOUNDED_CURVE()
B_SPLINE_CURVE(2,(#48118,#48119,#48120),.UNSPECIFIED.,.F.,.F.)
B_SPLINE_CURVE_WITH_KNOTS((3,3),(0.,0.00841282944265251),.UNSPECIFIED.)
CURVE()
GEOMETRIC_REPRESENTATION_ITEM()
RATIONAL_B_SPLINE_CURVE((1.,1.00035365746762,1.00043184882748))
REPRESENTATION_ITEM('')
);
#352=(
BOUNDED_CURVE()
B_SPLINE_CURVE(2,(#48124,#48125,#48126),.UNSPECIFIED.,.F.,.F.)
B_SPLINE_CURVE_WITH_KNOTS((3,3),(0.0131888113576473,0.0216016408002996),
 .UNSPECIFIED.)
CURVE()
GEOMETRIC_REPRESENTATION_ITEM()
RATIONAL_B_SPLINE_CURVE((1.00043184883165,1.00035365747103,1.))
REPRESENTATION_ITEM('')
);
#353=(
BOUNDED_CURVE()
B_SPLINE_CURVE(2,(#48139,#48140,#48141),.UNSPECIFIED.,.F.,.F.)
B_SPLINE_CURVE_WITH_KNOTS((3,3),(0.,0.00841282944262983),.UNSPECIFIED.)
CURVE()
GEOMETRIC_REPRESENTATION_ITEM()
RATIONAL_B_SPLINE_CURVE((1.,1.00035365747139,1.00043184883209))
REPRESENTATION_ITEM('')
);
#354=(
BOUNDED_CURVE()
B_SPLINE_CURVE(2,(#48145,#48146,#48147),.UNSPECIFIED.,.F.,.F.)
B_SPLINE_CURVE_WITH_KNOTS((3,3),(0.0131888113576388,0.0216016408002996),
 .UNSPECIFIED.)
CURVE()
GEOMETRIC_REPRESENTATION_ITEM()
RATIONAL_B_SPLINE_CURVE((1.00043184882737,1.00035365746753,1.))
REPRESENTATION_ITEM('')
);
#355=(
BOUNDED_CURVE()
B_SPLINE_CURVE(2,(#48160,#48161,#48162),.UNSPECIFIED.,.F.,.F.)
B_SPLINE_CURVE_WITH_KNOTS((3,3),(0.,0.00841282944261306),.UNSPECIFIED.)
CURVE()
GEOMETRIC_REPRESENTATION_ITEM()
RATIONAL_B_SPLINE_CURVE((1.,1.00035365747318,1.00043184883428))
REPRESENTATION_ITEM('')
);
#356=(
BOUNDED_CURVE()
B_SPLINE_CURVE(2,(#48166,#48167,#48168),.UNSPECIFIED.,.F.,.F.)
B_SPLINE_CURVE_WITH_KNOTS((3,3),(0.0131888113575341,0.0216016408002996),
 .UNSPECIFIED.)
CURVE()
GEOMETRIC_REPRESENTATION_ITEM()
RATIONAL_B_SPLINE_CURVE((1.00043184882813,1.00035365746816,1.))
REPRESENTATION_ITEM('')
);
#357=(
BOUNDED_CURVE()
B_SPLINE_CURVE(2,(#48183,#48184,#48185),.UNSPECIFIED.,.F.,.F.)
B_SPLINE_CURVE_WITH_KNOTS((3,3),(0.,0.00841282944268199),.UNSPECIFIED.)
CURVE()
GEOMETRIC_REPRESENTATION_ITEM()
RATIONAL_B_SPLINE_CURVE((1.,1.00035365746877,1.00043184882888))
REPRESENTATION_ITEM('')
);
#358=(
BOUNDED_CURVE()
B_SPLINE_CURVE(2,(#48189,#48190,#48191),.UNSPECIFIED.,.F.,.F.)
B_SPLINE_CURVE_WITH_KNOTS((3,3),(0.0131888113576103,0.0216016408002996),
 .UNSPECIFIED.)
CURVE()
GEOMETRIC_REPRESENTATION_ITEM()
RATIONAL_B_SPLINE_CURVE((1.00043184882915,1.00035365746898,1.))
REPRESENTATION_ITEM('')
);
#359=(
BOUNDED_CURVE()
B_SPLINE_CURVE(2,(#48204,#48205,#48206),.UNSPECIFIED.,.F.,.F.)
B_SPLINE_CURVE_WITH_KNOTS((3,3),(0.,0.00841282944276111),.UNSPECIFIED.)
CURVE()
GEOMETRIC_REPRESENTATION_ITEM()
RATIONAL_B_SPLINE_CURVE((1.,1.00035365746789,1.00043184882782))
REPRESENTATION_ITEM('')
);
#360=(
BOUNDED_CURVE()
B_SPLINE_CURVE(2,(#48210,#48211,#48212),.UNSPECIFIED.,.F.,.F.)
B_SPLINE_CURVE_WITH_KNOTS((3,3),(0.013188811357663,0.0216016408002997),
 .UNSPECIFIED.)
CURVE()
GEOMETRIC_REPRESENTATION_ITEM()
RATIONAL_B_SPLINE_CURVE((1.00043184882852,1.00035365746847,1.))
REPRESENTATION_ITEM('')
);
#361=(
BOUNDED_CURVE()
B_SPLINE_CURVE(2,(#48225,#48226,#48227),.UNSPECIFIED.,.F.,.F.)
B_SPLINE_CURVE_WITH_KNOTS((3,3),(0.,0.00841282944263208),.UNSPECIFIED.)
CURVE()
GEOMETRIC_REPRESENTATION_ITEM()
RATIONAL_B_SPLINE_CURVE((1.,1.00035365746816,1.00043184882815))
REPRESENTATION_ITEM('')
);
#362=(
BOUNDED_CURVE()
B_SPLINE_CURVE(2,(#48231,#48232,#48233),.UNSPECIFIED.,.F.,.F.)
B_SPLINE_CURVE_WITH_KNOTS((3,3),(0.013188811357748,0.0216016408002996),
 .UNSPECIFIED.)
CURVE()
GEOMETRIC_REPRESENTATION_ITEM()
RATIONAL_B_SPLINE_CURVE((1.00043184883132,1.00035365747076,1.))
REPRESENTATION_ITEM('')
);
#363=(
BOUNDED_CURVE()
B_SPLINE_CURVE(2,(#48246,#48247,#48248),.UNSPECIFIED.,.F.,.F.)
B_SPLINE_CURVE_WITH_KNOTS((3,3),(0.,0.00841282944264326),.UNSPECIFIED.)
CURVE()
GEOMETRIC_REPRESENTATION_ITEM()
RATIONAL_B_SPLINE_CURVE((1.,1.00035365746759,1.00043184882744))
REPRESENTATION_ITEM('')
);
#364=(
BOUNDED_CURVE()
B_SPLINE_CURVE(2,(#48252,#48253,#48254),.UNSPECIFIED.,.F.,.F.)
B_SPLINE_CURVE_WITH_KNOTS((3,3),(0.0131888113575487,0.0216016408002996),
 .UNSPECIFIED.)
CURVE()
GEOMETRIC_REPRESENTATION_ITEM()
RATIONAL_B_SPLINE_CURVE((1.0004318488259,1.00035365746632,1.))
REPRESENTATION_ITEM('')
);
#365=(
BOUNDED_CURVE()
B_SPLINE_CURVE(2,(#48267,#48268,#48269),.UNSPECIFIED.,.F.,.F.)
B_SPLINE_CURVE_WITH_KNOTS((3,3),(0.,0.00841282944280138),.UNSPECIFIED.)
CURVE()
GEOMETRIC_REPRESENTATION_ITEM()
RATIONAL_B_SPLINE_CURVE((1.,1.00035365746471,1.00043184882392))
REPRESENTATION_ITEM('')
);
#366=(
BOUNDED_CURVE()
B_SPLINE_CURVE(2,(#48273,#48274,#48275),.UNSPECIFIED.,.F.,.F.)
B_SPLINE_CURVE_WITH_KNOTS((3,3),(0.0131888113575931,0.0216016408002996),
 .UNSPECIFIED.)
CURVE()
GEOMETRIC_REPRESENTATION_ITEM()
RATIONAL_B_SPLINE_CURVE((1.00043184882494,1.00035365746554,1.))
REPRESENTATION_ITEM('')
);
#367=(
BOUNDED_CURVE()
B_SPLINE_CURVE(2,(#48288,#48289,#48290),.UNSPECIFIED.,.F.,.F.)
B_SPLINE_CURVE_WITH_KNOTS((3,3),(0.,0.00841282944270105),.UNSPECIFIED.)
CURVE()
GEOMETRIC_REPRESENTATION_ITEM()
RATIONAL_B_SPLINE_CURVE((1.,1.000353657467,1.00043184882673))
REPRESENTATION_ITEM('')
);
#368=(
BOUNDED_CURVE()
B_SPLINE_CURVE(2,(#48294,#48295,#48296),.UNSPECIFIED.,.F.,.F.)
B_SPLINE_CURVE_WITH_KNOTS((3,3),(0.0131888113574971,0.0216016408002996),
 .UNSPECIFIED.)
CURVE()
GEOMETRIC_REPRESENTATION_ITEM()
RATIONAL_B_SPLINE_CURVE((1.00043184882773,1.00035365746783,1.))
REPRESENTATION_ITEM('')
);
#369=(
BOUNDED_CURVE()
B_SPLINE_CURVE(2,(#48309,#48310,#48311),.UNSPECIFIED.,.F.,.F.)
B_SPLINE_CURVE_WITH_KNOTS((3,3),(0.,0.00841282944264652),.UNSPECIFIED.)
CURVE()
GEOMETRIC_REPRESENTATION_ITEM()
RATIONAL_B_SPLINE_CURVE((1.,1.00035365746972,1.00043184883004))
REPRESENTATION_ITEM('')
);
#370=(
BOUNDED_CURVE()
B_SPLINE_CURVE(2,(#48315,#48316,#48317),.UNSPECIFIED.,.F.,.F.)
B_SPLINE_CURVE_WITH_KNOTS((3,3),(0.0131888113576371,0.0216016408002996),
 .UNSPECIFIED.)
CURVE()
GEOMETRIC_REPRESENTATION_ITEM()
RATIONAL_B_SPLINE_CURVE((1.00043184882659,1.00035365746689,1.))
REPRESENTATION_ITEM('')
);
#371=(
BOUNDED_CURVE()
B_SPLINE_CURVE(2,(#48330,#48331,#48332),.UNSPECIFIED.,.F.,.F.)
B_SPLINE_CURVE_WITH_KNOTS((3,3),(0.,0.00841282944262983),.UNSPECIFIED.)
CURVE()
GEOMETRIC_REPRESENTATION_ITEM()
RATIONAL_B_SPLINE_CURVE((1.,1.00035365747139,1.00043184883209))
REPRESENTATION_ITEM('')
);
#372=(
BOUNDED_CURVE()
B_SPLINE_CURVE(2,(#48336,#48337,#48338),.UNSPECIFIED.,.F.,.F.)
B_SPLINE_CURVE_WITH_KNOTS((3,3),(0.0131888113576388,0.0216016408002996),
 .UNSPECIFIED.)
CURVE()
GEOMETRIC_REPRESENTATION_ITEM()
RATIONAL_B_SPLINE_CURVE((1.00043184882737,1.00035365746753,1.))
REPRESENTATION_ITEM('')
);
#373=(
BOUNDED_CURVE()
B_SPLINE_CURVE(2,(#48351,#48352,#48353),.UNSPECIFIED.,.F.,.F.)
B_SPLINE_CURVE_WITH_KNOTS((3,3),(0.,0.00841282944264003),.UNSPECIFIED.)
CURVE()
GEOMETRIC_REPRESENTATION_ITEM()
RATIONAL_B_SPLINE_CURVE((1.,1.0003536574673,1.00043184882709))
REPRESENTATION_ITEM('')
);
#374=(
BOUNDED_CURVE()
B_SPLINE_CURVE(2,(#48357,#48358,#48359),.UNSPECIFIED.,.F.,.F.)
B_SPLINE_CURVE_WITH_KNOTS((3,3),(0.0131888113576155,0.0216016408002996),
 .UNSPECIFIED.)
CURVE()
GEOMETRIC_REPRESENTATION_ITEM()
RATIONAL_B_SPLINE_CURVE((1.00043184882608,1.00035365746647,1.))
REPRESENTATION_ITEM('')
);
#375=(
BOUNDED_CURVE()
B_SPLINE_CURVE(2,(#48372,#48373,#48374),.UNSPECIFIED.,.F.,.F.)
B_SPLINE_CURVE_WITH_KNOTS((3,3),(0.,0.00841282944269557),.UNSPECIFIED.)
CURVE()
GEOMETRIC_REPRESENTATION_ITEM()
RATIONAL_B_SPLINE_CURVE((1.,1.00035365746722,1.000431848827))
REPRESENTATION_ITEM('')
);
#376=(
BOUNDED_CURVE()
B_SPLINE_CURVE(2,(#48378,#48379,#48380),.UNSPECIFIED.,.F.,.F.)
B_SPLINE_CURVE_WITH_KNOTS((3,3),(0.0131888113576143,0.0216016408002996),
 .UNSPECIFIED.)
CURVE()
GEOMETRIC_REPRESENTATION_ITEM()
RATIONAL_B_SPLINE_CURVE((1.00043184882947,1.00035365746925,1.))
REPRESENTATION_ITEM('')
);
#377=(
BOUNDED_CURVE()
B_SPLINE_CURVE(2,(#48393,#48394,#48395),.UNSPECIFIED.,.F.,.F.)
B_SPLINE_CURVE_WITH_KNOTS((3,3),(0.,0.00841282944278065),.UNSPECIFIED.)
CURVE()
GEOMETRIC_REPRESENTATION_ITEM()
RATIONAL_B_SPLINE_CURVE((1.,1.00035365746947,1.00043184882974))
REPRESENTATION_ITEM('')
);
#378=(
BOUNDED_CURVE()
B_SPLINE_CURVE(2,(#48399,#48400,#48401),.UNSPECIFIED.,.F.,.F.)
B_SPLINE_CURVE_WITH_KNOTS((3,3),(0.0131888113576697,0.0216016408002996),
 .UNSPECIFIED.)
CURVE()
GEOMETRIC_REPRESENTATION_ITEM()
RATIONAL_B_SPLINE_CURVE((1.00043184882899,1.00035365746886,1.))
REPRESENTATION_ITEM('')
);
#379=(
BOUNDED_CURVE()
B_SPLINE_CURVE(2,(#48414,#48415,#48416),.UNSPECIFIED.,.F.,.F.)
B_SPLINE_CURVE_WITH_KNOTS((3,3),(0.,0.00841282944263208),.UNSPECIFIED.)
CURVE()
GEOMETRIC_REPRESENTATION_ITEM()
RATIONAL_B_SPLINE_CURVE((1.,1.00035365746816,1.00043184882815))
REPRESENTATION_ITEM('')
);
#380=(
BOUNDED_CURVE()
B_SPLINE_CURVE(2,(#48420,#48421,#48422),.UNSPECIFIED.,.F.,.F.)
B_SPLINE_CURVE_WITH_KNOTS((3,3),(0.013188811357748,0.0216016408002996),
 .UNSPECIFIED.)
CURVE()
GEOMETRIC_REPRESENTATION_ITEM()
RATIONAL_B_SPLINE_CURVE((1.00043184883132,1.00035365747076,1.))
REPRESENTATION_ITEM('')
);
#381=(
BOUNDED_CURVE()
B_SPLINE_CURVE(2,(#48435,#48436,#48437),.UNSPECIFIED.,.F.,.F.)
B_SPLINE_CURVE_WITH_KNOTS((3,3),(0.,0.00841282944273455),.UNSPECIFIED.)
CURVE()
GEOMETRIC_REPRESENTATION_ITEM()
RATIONAL_B_SPLINE_CURVE((1.,1.00035365746539,1.00043184882476))
REPRESENTATION_ITEM('')
);
#382=(
BOUNDED_CURVE()
B_SPLINE_CURVE(2,(#48441,#48442,#48443),.UNSPECIFIED.,.F.,.F.)
B_SPLINE_CURVE_WITH_KNOTS((3,3),(0.0131888113576539,0.0216016408002996),
 .UNSPECIFIED.)
CURVE()
GEOMETRIC_REPRESENTATION_ITEM()
RATIONAL_B_SPLINE_CURVE((1.00043184882929,1.0003536574691,1.))
REPRESENTATION_ITEM('')
);
#383=(
BOUNDED_CURVE()
B_SPLINE_CURVE(2,(#48456,#48457,#48458),.UNSPECIFIED.,.F.,.F.)
B_SPLINE_CURVE_WITH_KNOTS((3,3),(0.,0.00841282944270133),.UNSPECIFIED.)
CURVE()
GEOMETRIC_REPRESENTATION_ITEM()
RATIONAL_B_SPLINE_CURVE((1.,1.00035365747008,1.00043184883048))
REPRESENTATION_ITEM('')
);
#384=(
BOUNDED_CURVE()
B_SPLINE_CURVE(2,(#48462,#48463,#48464),.UNSPECIFIED.,.F.,.F.)
B_SPLINE_CURVE_WITH_KNOTS((3,3),(0.0131888113576197,0.0216016408002996),
 .UNSPECIFIED.)
CURVE()
GEOMETRIC_REPRESENTATION_ITEM()
RATIONAL_B_SPLINE_CURVE((1.00043184882798,1.00035365746803,1.))
REPRESENTATION_ITEM('')
);
#385=(
BOUNDED_CURVE()
B_SPLINE_CURVE(2,(#48477,#48478,#48479),.UNSPECIFIED.,.F.,.F.)
B_SPLINE_CURVE_WITH_KNOTS((3,3),(0.,0.00841282944261464),.UNSPECIFIED.)
CURVE()
GEOMETRIC_REPRESENTATION_ITEM()
RATIONAL_B_SPLINE_CURVE((1.,1.00035365746679,1.00043184882648))
REPRESENTATION_ITEM('')
);
#386=(
BOUNDED_CURVE()
B_SPLINE_CURVE(2,(#48483,#48484,#48485),.UNSPECIFIED.,.F.,.F.)
B_SPLINE_CURVE_WITH_KNOTS((3,3),(0.0131888113575887,0.0216016408002996),
 .UNSPECIFIED.)
CURVE()
GEOMETRIC_REPRESENTATION_ITEM()
RATIONAL_B_SPLINE_CURVE((1.00043184882758,1.0003536574677,1.))
REPRESENTATION_ITEM('')
);
#387=(
BOUNDED_CURVE()
B_SPLINE_CURVE(2,(#48498,#48499,#48500),.UNSPECIFIED.,.F.,.F.)
B_SPLINE_CURVE_WITH_KNOTS((3,3),(0.,0.00841282944264924),.UNSPECIFIED.)
CURVE()
GEOMETRIC_REPRESENTATION_ITEM()
RATIONAL_B_SPLINE_CURVE((1.,1.00035365746952,1.00043184882981))
REPRESENTATION_ITEM('')
);
#388=(
BOUNDED_CURVE()
B_SPLINE_CURVE(2,(#48504,#48505,#48506),.UNSPECIFIED.,.F.,.F.)
B_SPLINE_CURVE_WITH_KNOTS((3,3),(0.0131888113576407,0.0216016408002996),
 .UNSPECIFIED.)
CURVE()
GEOMETRIC_REPRESENTATION_ITEM()
RATIONAL_B_SPLINE_CURVE((1.00043184882821,1.00035365746821,1.))
REPRESENTATION_ITEM('')
);
#389=(
BOUNDED_CURVE()
B_SPLINE_CURVE(2,(#48519,#48520,#48521),.UNSPECIFIED.,.F.,.F.)
B_SPLINE_CURVE_WITH_KNOTS((3,3),(0.,0.00841282944262983),.UNSPECIFIED.)
CURVE()
GEOMETRIC_REPRESENTATION_ITEM()
RATIONAL_B_SPLINE_CURVE((1.,1.00035365747139,1.00043184883209))
REPRESENTATION_ITEM('')
);
#390=(
BOUNDED_CURVE()
B_SPLINE_CURVE(2,(#48525,#48526,#48527),.UNSPECIFIED.,.F.,.F.)
B_SPLINE_CURVE_WITH_KNOTS((3,3),(0.0131888113576388,0.0216016408002996),
 .UNSPECIFIED.)
CURVE()
GEOMETRIC_REPRESENTATION_ITEM()
RATIONAL_B_SPLINE_CURVE((1.00043184882737,1.00035365746753,1.))
REPRESENTATION_ITEM('')
);
#391=(
BOUNDED_CURVE()
B_SPLINE_CURVE(2,(#48540,#48541,#48542),.UNSPECIFIED.,.F.,.F.)
B_SPLINE_CURVE_WITH_KNOTS((3,3),(0.,0.0084128294426321),.UNSPECIFIED.)
CURVE()
GEOMETRIC_REPRESENTATION_ITEM()
RATIONAL_B_SPLINE_CURVE((1.,1.00035365746883,1.00043184882896))
REPRESENTATION_ITEM('')
);
#392=(
BOUNDED_CURVE()
B_SPLINE_CURVE(2,(#48546,#48547,#48548),.UNSPECIFIED.,.F.,.F.)
B_SPLINE_CURVE_WITH_KNOTS((3,3),(0.0131888113575073,0.0216016408002996),
 .UNSPECIFIED.)
CURVE()
GEOMETRIC_REPRESENTATION_ITEM()
RATIONAL_B_SPLINE_CURVE((1.00043184882395,1.00035365746473,1.))
REPRESENTATION_ITEM('')
);
#393=(
BOUNDED_CURVE()
B_SPLINE_CURVE(2,(#48601,#48602,#48603),.UNSPECIFIED.,.F.,.F.)
B_SPLINE_CURVE_WITH_KNOTS((3,3),(0.,0.00841282944285724),.UNSPECIFIED.)
CURVE()
GEOMETRIC_REPRESENTATION_ITEM()
RATIONAL_B_SPLINE_CURVE((1.,1.00035365746964,1.00043184882994))
REPRESENTATION_ITEM('')
);
#394=(
BOUNDED_CURVE()
B_SPLINE_CURVE(2,(#48605,#48606,#48607),.UNSPECIFIED.,.F.,.F.)
B_SPLINE_CURVE_WITH_KNOTS((3,3),(0.0131888113574265,0.0216016408002996),
 .UNSPECIFIED.)
CURVE()
GEOMETRIC_REPRESENTATION_ITEM()
RATIONAL_B_SPLINE_CURVE((1.00043184882266,1.00035365746368,1.))
REPRESENTATION_ITEM('')
);
#395=(
BOUNDED_CURVE()
B_SPLINE_CURVE(2,(#50435,#50436,#50437),.UNSPECIFIED.,.F.,.F.)
B_SPLINE_CURVE_WITH_KNOTS((3,3),(0.,0.00844890352465847),.UNSPECIFIED.)
CURVE()
GEOMETRIC_REPRESENTATION_ITEM()
RATIONAL_B_SPLINE_CURVE((1.,1.00024991829741,1.0003043270601))
REPRESENTATION_ITEM('')
);
#396=(
BOUNDED_CURVE()
B_SPLINE_CURVE(2,(#50441,#50442,#50443),.UNSPECIFIED.,.F.,.F.)
B_SPLINE_CURVE_WITH_KNOTS((3,3),(0.0131514300538184,0.0216003335786744),
 .UNSPECIFIED.)
CURVE()
GEOMETRIC_REPRESENTATION_ITEM()
RATIONAL_B_SPLINE_CURVE((1.00030432705462,1.00024991829291,1.))
REPRESENTATION_ITEM('')
);
#397=(
BOUNDED_CURVE()
B_SPLINE_CURVE(2,(#50456,#50457,#50458),.UNSPECIFIED.,.F.,.F.)
B_SPLINE_CURVE_WITH_KNOTS((3,3),(0.,0.00844890352461359),.UNSPECIFIED.)
CURVE()
GEOMETRIC_REPRESENTATION_ITEM()
RATIONAL_B_SPLINE_CURVE((1.,1.00024991829433,1.00030432705636))
REPRESENTATION_ITEM('')
);
#398=(
BOUNDED_CURVE()
B_SPLINE_CURVE(2,(#50462,#50463,#50464),.UNSPECIFIED.,.F.,.F.)
B_SPLINE_CURVE_WITH_KNOTS((3,3),(0.0131514300539352,0.0216003335786744),
 .UNSPECIFIED.)
CURVE()
GEOMETRIC_REPRESENTATION_ITEM()
RATIONAL_B_SPLINE_CURVE((1.0003043270645,1.00024991830102,1.))
REPRESENTATION_ITEM('')
);
#399=(
BOUNDED_CURVE()
B_SPLINE_CURVE(2,(#50477,#50478,#50479),.UNSPECIFIED.,.F.,.F.)
B_SPLINE_CURVE_WITH_KNOTS((3,3),(0.,0.00844890352451554),.UNSPECIFIED.)
CURVE()
GEOMETRIC_REPRESENTATION_ITEM()
RATIONAL_B_SPLINE_CURVE((1.,1.00024991829624,1.00030432705868))
REPRESENTATION_ITEM('')
);
#400=(
BOUNDED_CURVE()
B_SPLINE_CURVE(2,(#50483,#50484,#50485),.UNSPECIFIED.,.F.,.F.)
B_SPLINE_CURVE_WITH_KNOTS((3,3),(0.0131514300537974,0.0216003335786744),
 .UNSPECIFIED.)
CURVE()
GEOMETRIC_REPRESENTATION_ITEM()
RATIONAL_B_SPLINE_CURVE((1.00030432705135,1.00024991829022,1.))
REPRESENTATION_ITEM('')
);
#401=(
BOUNDED_CURVE()
B_SPLINE_CURVE(2,(#50498,#50499,#50500),.UNSPECIFIED.,.F.,.F.)
B_SPLINE_CURVE_WITH_KNOTS((3,3),(0.,0.00844890352473773),.UNSPECIFIED.)
CURVE()
GEOMETRIC_REPRESENTATION_ITEM()
RATIONAL_B_SPLINE_CURVE((1.,1.00024991829766,1.0003043270604))
REPRESENTATION_ITEM('')
);
#402=(
BOUNDED_CURVE()
B_SPLINE_CURVE(2,(#50504,#50505,#50506),.UNSPECIFIED.,.F.,.F.)
B_SPLINE_CURVE_WITH_KNOTS((3,3),(0.0131514300540393,0.0216003335786744),
 .UNSPECIFIED.)
CURVE()
GEOMETRIC_REPRESENTATION_ITEM()
RATIONAL_B_SPLINE_CURVE((1.00030432705889,1.00024991829642,1.))
REPRESENTATION_ITEM('')
);
#403=(
BOUNDED_CURVE()
B_SPLINE_CURVE(2,(#50519,#50520,#50521),.UNSPECIFIED.,.F.,.F.)
B_SPLINE_CURVE_WITH_KNOTS((3,3),(0.,0.00844890352488385),.UNSPECIFIED.)
CURVE()
GEOMETRIC_REPRESENTATION_ITEM()
RATIONAL_B_SPLINE_CURVE((1.,1.00024991830158,1.00030432706517))
REPRESENTATION_ITEM('')
);
#404=(
BOUNDED_CURVE()
B_SPLINE_CURVE(2,(#50525,#50526,#50527),.UNSPECIFIED.,.F.,.F.)
B_SPLINE_CURVE_WITH_KNOTS((3,3),(0.0131514300539214,0.0216003335786743),
 .UNSPECIFIED.)
CURVE()
GEOMETRIC_REPRESENTATION_ITEM()
RATIONAL_B_SPLINE_CURVE((1.00030432705957,1.00024991829698,1.))
REPRESENTATION_ITEM('')
);
#405=(
BOUNDED_CURVE()
B_SPLINE_CURVE(2,(#50540,#50541,#50542),.UNSPECIFIED.,.F.,.F.)
B_SPLINE_CURVE_WITH_KNOTS((3,3),(0.,0.00844890352469842),.UNSPECIFIED.)
CURVE()
GEOMETRIC_REPRESENTATION_ITEM()
RATIONAL_B_SPLINE_CURVE((1.,1.00024991830078,1.00030432706421))
REPRESENTATION_ITEM('')
);
#406=(
BOUNDED_CURVE()
B_SPLINE_CURVE(2,(#50546,#50547,#50548),.UNSPECIFIED.,.F.,.F.)
B_SPLINE_CURVE_WITH_KNOTS((3,3),(0.0131514300540325,0.0216003335786744),
 .UNSPECIFIED.)
CURVE()
GEOMETRIC_REPRESENTATION_ITEM()
RATIONAL_B_SPLINE_CURVE((1.00030432705744,1.00024991829522,1.))
REPRESENTATION_ITEM('')
);
#407=(
BOUNDED_CURVE()
B_SPLINE_CURVE(2,(#50561,#50562,#50563),.UNSPECIFIED.,.F.,.F.)
B_SPLINE_CURVE_WITH_KNOTS((3,3),(0.,0.00844890352489384),.UNSPECIFIED.)
CURVE()
GEOMETRIC_REPRESENTATION_ITEM()
RATIONAL_B_SPLINE_CURVE((1.,1.0002499182915,1.0003043270529))
REPRESENTATION_ITEM('')
);
#408=(
BOUNDED_CURVE()
B_SPLINE_CURVE(2,(#50567,#50568,#50569),.UNSPECIFIED.,.F.,.F.)
B_SPLINE_CURVE_WITH_KNOTS((3,3),(0.0131514300537262,0.0216003335786744),
 .UNSPECIFIED.)
CURVE()
GEOMETRIC_REPRESENTATION_ITEM()
RATIONAL_B_SPLINE_CURVE((1.00030432705672,1.00024991829464,1.))
REPRESENTATION_ITEM('')
);
#409=(
BOUNDED_CURVE()
B_SPLINE_CURVE(2,(#50582,#50583,#50584),.UNSPECIFIED.,.F.,.F.)
B_SPLINE_CURVE_WITH_KNOTS((3,3),(0.,0.00844890352459677),.UNSPECIFIED.)
CURVE()
GEOMETRIC_REPRESENTATION_ITEM()
RATIONAL_B_SPLINE_CURVE((1.,1.00024991829595,1.00030432705833))
REPRESENTATION_ITEM('')
);
#410=(
BOUNDED_CURVE()
B_SPLINE_CURVE(2,(#50588,#50589,#50590),.UNSPECIFIED.,.F.,.F.)
B_SPLINE_CURVE_WITH_KNOTS((3,3),(0.0131514300537522,0.0216003335786743),
 .UNSPECIFIED.)
CURVE()
GEOMETRIC_REPRESENTATION_ITEM()
RATIONAL_B_SPLINE_CURVE((1.00030432705926,1.00024991829673,1.))
REPRESENTATION_ITEM('')
);
#411=(
BOUNDED_CURVE()
B_SPLINE_CURVE(2,(#50603,#50604,#50605),.UNSPECIFIED.,.F.,.F.)
B_SPLINE_CURVE_WITH_KNOTS((3,3),(0.,0.00844890352497871),.UNSPECIFIED.)
CURVE()
GEOMETRIC_REPRESENTATION_ITEM()
RATIONAL_B_SPLINE_CURVE((1.,1.00024991829262,1.00030432705426))
REPRESENTATION_ITEM('')
);
#412=(
BOUNDED_CURVE()
B_SPLINE_CURVE(2,(#50609,#50610,#50611),.UNSPECIFIED.,.F.,.F.)
B_SPLINE_CURVE_WITH_KNOTS((3,3),(0.013151430053846,0.0216003335786743),
 .UNSPECIFIED.)
CURVE()
GEOMETRIC_REPRESENTATION_ITEM()
RATIONAL_B_SPLINE_CURVE((1.00030432705891,1.00024991829644,1.))
REPRESENTATION_ITEM('')
);
#413=(
BOUNDED_CURVE()
B_SPLINE_CURVE(2,(#50624,#50625,#50626),.UNSPECIFIED.,.F.,.F.)
B_SPLINE_CURVE_WITH_KNOTS((3,3),(0.,0.0084489035249234),.UNSPECIFIED.)
CURVE()
GEOMETRIC_REPRESENTATION_ITEM()
RATIONAL_B_SPLINE_CURVE((1.,1.00024991829376,1.00030432705565))
REPRESENTATION_ITEM('')
);
#414=(
BOUNDED_CURVE()
B_SPLINE_CURVE(2,(#50630,#50631,#50632),.UNSPECIFIED.,.F.,.F.)
B_SPLINE_CURVE_WITH_KNOTS((3,3),(0.0131514300540803,0.0216003335786743),
 .UNSPECIFIED.)
CURVE()
GEOMETRIC_REPRESENTATION_ITEM()
RATIONAL_B_SPLINE_CURVE((1.00030432705876,1.00024991829631,1.))
REPRESENTATION_ITEM('')
);
#415=(
BOUNDED_CURVE()
B_SPLINE_CURVE(2,(#50645,#50646,#50647),.UNSPECIFIED.,.F.,.F.)
B_SPLINE_CURVE_WITH_KNOTS((3,3),(0.,0.00844890352494163),.UNSPECIFIED.)
CURVE()
GEOMETRIC_REPRESENTATION_ITEM()
RATIONAL_B_SPLINE_CURVE((1.,1.00024991829715,1.00030432705978))
REPRESENTATION_ITEM('')
);
#416=(
BOUNDED_CURVE()
B_SPLINE_CURVE(2,(#50651,#50652,#50653),.UNSPECIFIED.,.F.,.F.)
B_SPLINE_CURVE_WITH_KNOTS((3,3),(0.0131514300539219,0.0216003335786744),
 .UNSPECIFIED.)
CURVE()
GEOMETRIC_REPRESENTATION_ITEM()
RATIONAL_B_SPLINE_CURVE((1.00030432706217,1.00024991829911,1.))
REPRESENTATION_ITEM('')
);
#417=(
BOUNDED_CURVE()
B_SPLINE_CURVE(2,(#50666,#50667,#50668),.UNSPECIFIED.,.F.,.F.)
B_SPLINE_CURVE_WITH_KNOTS((3,3),(0.,0.00844890352451554),.UNSPECIFIED.)
CURVE()
GEOMETRIC_REPRESENTATION_ITEM()
RATIONAL_B_SPLINE_CURVE((1.,1.00024991829624,1.00030432705868))
REPRESENTATION_ITEM('')
);
#418=(
BOUNDED_CURVE()
B_SPLINE_CURVE(2,(#50672,#50673,#50674),.UNSPECIFIED.,.F.,.F.)
B_SPLINE_CURVE_WITH_KNOTS((3,3),(0.0131514300537974,0.0216003335786744),
 .UNSPECIFIED.)
CURVE()
GEOMETRIC_REPRESENTATION_ITEM()
RATIONAL_B_SPLINE_CURVE((1.00030432705135,1.00024991829022,1.))
REPRESENTATION_ITEM('')
);
#419=(
BOUNDED_CURVE()
B_SPLINE_CURVE(2,(#50687,#50688,#50689),.UNSPECIFIED.,.F.,.F.)
B_SPLINE_CURVE_WITH_KNOTS((3,3),(0.,0.00844890352463462),.UNSPECIFIED.)
CURVE()
GEOMETRIC_REPRESENTATION_ITEM()
RATIONAL_B_SPLINE_CURVE((1.,1.00024991830016,1.00030432706346))
REPRESENTATION_ITEM('')
);
#420=(
BOUNDED_CURVE()
B_SPLINE_CURVE(2,(#50693,#50694,#50695),.UNSPECIFIED.,.F.,.F.)
B_SPLINE_CURVE_WITH_KNOTS((3,3),(0.0131514300541893,0.0216003335786744),
 .UNSPECIFIED.)
CURVE()
GEOMETRIC_REPRESENTATION_ITEM()
RATIONAL_B_SPLINE_CURVE((1.00030432706113,1.00024991829825,1.))
REPRESENTATION_ITEM('')
);
#421=(
BOUNDED_CURVE()
B_SPLINE_CURVE(2,(#50708,#50709,#50710),.UNSPECIFIED.,.F.,.F.)
B_SPLINE_CURVE_WITH_KNOTS((3,3),(0.,0.00844890352460222),.UNSPECIFIED.)
CURVE()
GEOMETRIC_REPRESENTATION_ITEM()
RATIONAL_B_SPLINE_CURVE((1.,1.00024991829658,1.00030432705909))
REPRESENTATION_ITEM('')
);
#422=(
BOUNDED_CURVE()
B_SPLINE_CURVE(2,(#50714,#50715,#50716),.UNSPECIFIED.,.F.,.F.)
B_SPLINE_CURVE_WITH_KNOTS((3,3),(0.0131514300537623,0.0216003335786744),
 .UNSPECIFIED.)
CURVE()
GEOMETRIC_REPRESENTATION_ITEM()
RATIONAL_B_SPLINE_CURVE((1.00030432705572,1.00024991829381,1.))
REPRESENTATION_ITEM('')
);
#423=(
BOUNDED_CURVE()
B_SPLINE_CURVE(2,(#50729,#50730,#50731),.UNSPECIFIED.,.F.,.F.)
B_SPLINE_CURVE_WITH_KNOTS((3,3),(0.,0.00844890352469488),.UNSPECIFIED.)
CURVE()
GEOMETRIC_REPRESENTATION_ITEM()
RATIONAL_B_SPLINE_CURVE((1.,1.00024991830183,1.00030432706549))
REPRESENTATION_ITEM('')
);
#424=(
BOUNDED_CURVE()
B_SPLINE_CURVE(2,(#50735,#50736,#50737),.UNSPECIFIED.,.F.,.F.)
B_SPLINE_CURVE_WITH_KNOTS((3,3),(0.0131514300540722,0.0216003335786744),
 .UNSPECIFIED.)
CURVE()
GEOMETRIC_REPRESENTATION_ITEM()
RATIONAL_B_SPLINE_CURVE((1.00030432706317,1.00024991829993,1.))
REPRESENTATION_ITEM('')
);
#425=(
BOUNDED_CURVE()
B_SPLINE_CURVE(2,(#50750,#50751,#50752),.UNSPECIFIED.,.F.,.F.)
B_SPLINE_CURVE_WITH_KNOTS((3,3),(0.,0.00844890352449406),.UNSPECIFIED.)
CURVE()
GEOMETRIC_REPRESENTATION_ITEM()
RATIONAL_B_SPLINE_CURVE((1.,1.00024991829771,1.00030432706047))
REPRESENTATION_ITEM('')
);
#426=(
BOUNDED_CURVE()
B_SPLINE_CURVE(2,(#50756,#50757,#50758),.UNSPECIFIED.,.F.,.F.)
B_SPLINE_CURVE_WITH_KNOTS((3,3),(0.0131514300538891,0.0216003335786743),
 .UNSPECIFIED.)
CURVE()
GEOMETRIC_REPRESENTATION_ITEM()
RATIONAL_B_SPLINE_CURVE((1.00030432705489,1.00024991829313,1.))
REPRESENTATION_ITEM('')
);
#427=(
BOUNDED_CURVE()
B_SPLINE_CURVE(2,(#50771,#50772,#50773),.UNSPECIFIED.,.F.,.F.)
B_SPLINE_CURVE_WITH_KNOTS((3,3),(0.,0.0084489035245959),.UNSPECIFIED.)
CURVE()
GEOMETRIC_REPRESENTATION_ITEM()
RATIONAL_B_SPLINE_CURVE((1.,1.00024991829567,1.00030432705798))
REPRESENTATION_ITEM('')
);
#428=(
BOUNDED_CURVE()
B_SPLINE_CURVE(2,(#50777,#50778,#50779),.UNSPECIFIED.,.F.,.F.)
B_SPLINE_CURVE_WITH_KNOTS((3,3),(0.0131514300537466,0.0216003335786743),
 .UNSPECIFIED.)
CURVE()
GEOMETRIC_REPRESENTATION_ITEM()
RATIONAL_B_SPLINE_CURVE((1.00030432705734,1.00024991829515,1.))
REPRESENTATION_ITEM('')
);
#429=(
BOUNDED_CURVE()
B_SPLINE_CURVE(2,(#50794,#50795,#50796),.UNSPECIFIED.,.F.,.F.)
B_SPLINE_CURVE_WITH_KNOTS((3,3),(0.,0.00844890352496291),.UNSPECIFIED.)
CURVE()
GEOMETRIC_REPRESENTATION_ITEM()
RATIONAL_B_SPLINE_CURVE((1.,1.00024991829663,1.00030432705914))
REPRESENTATION_ITEM('')
);
#430=(
BOUNDED_CURVE()
B_SPLINE_CURVE(2,(#50800,#50801,#50802),.UNSPECIFIED.,.F.,.F.)
B_SPLINE_CURVE_WITH_KNOTS((3,3),(0.0131514300540908,0.0216003335786744),
 .UNSPECIFIED.)
CURVE()
GEOMETRIC_REPRESENTATION_ITEM()
RATIONAL_B_SPLINE_CURVE((1.00030432705721,1.00024991829503,1.))
REPRESENTATION_ITEM('')
);
#431=(
BOUNDED_CURVE()
B_SPLINE_CURVE(2,(#50815,#50816,#50817),.UNSPECIFIED.,.F.,.F.)
B_SPLINE_CURVE_WITH_KNOTS((3,3),(0.,0.00844890352464343),.UNSPECIFIED.)
CURVE()
GEOMETRIC_REPRESENTATION_ITEM()
RATIONAL_B_SPLINE_CURVE((1.,1.00024991829906,1.00030432706212))
REPRESENTATION_ITEM('')
);
#432=(
BOUNDED_CURVE()
B_SPLINE_CURVE(2,(#50821,#50822,#50823),.UNSPECIFIED.,.F.,.F.)
B_SPLINE_CURVE_WITH_KNOTS((3,3),(0.0131514300538374,0.0216003335786744),
 .UNSPECIFIED.)
CURVE()
GEOMETRIC_REPRESENTATION_ITEM()
RATIONAL_B_SPLINE_CURVE((1.00030432706069,1.0002499182979,1.))
REPRESENTATION_ITEM('')
);
#433=(
BOUNDED_CURVE()
B_SPLINE_CURVE(2,(#50836,#50837,#50838),.UNSPECIFIED.,.F.,.F.)
B_SPLINE_CURVE_WITH_KNOTS((3,3),(0.,0.00844890352478188),.UNSPECIFIED.)
CURVE()
GEOMETRIC_REPRESENTATION_ITEM()
RATIONAL_B_SPLINE_CURVE((1.,1.00024991829664,1.00030432705917))
REPRESENTATION_ITEM('')
);
#434=(
BOUNDED_CURVE()
B_SPLINE_CURVE(2,(#50842,#50843,#50844),.UNSPECIFIED.,.F.,.F.)
B_SPLINE_CURVE_WITH_KNOTS((3,3),(0.0131514300539186,0.0216003335786744),
 .UNSPECIFIED.)
CURVE()
GEOMETRIC_REPRESENTATION_ITEM()
RATIONAL_B_SPLINE_CURVE((1.00030432706174,1.00024991829875,1.))
REPRESENTATION_ITEM('')
);
#435=(
BOUNDED_CURVE()
B_SPLINE_CURVE(2,(#50857,#50858,#50859),.UNSPECIFIED.,.F.,.F.)
B_SPLINE_CURVE_WITH_KNOTS((3,3),(0.,0.00844890352473528),.UNSPECIFIED.)
CURVE()
GEOMETRIC_REPRESENTATION_ITEM()
RATIONAL_B_SPLINE_CURVE((1.,1.00024991829715,1.00030432705979))
REPRESENTATION_ITEM('')
);
#436=(
BOUNDED_CURVE()
B_SPLINE_CURVE(2,(#50863,#50864,#50865),.UNSPECIFIED.,.F.,.F.)
B_SPLINE_CURVE_WITH_KNOTS((3,3),(0.0131514300540877,0.0216003335786744),
 .UNSPECIFIED.)
CURVE()
GEOMETRIC_REPRESENTATION_ITEM()
RATIONAL_B_SPLINE_CURVE((1.00030432705704,1.0002499182949,1.))
REPRESENTATION_ITEM('')
);
#437=(
BOUNDED_CURVE()
B_SPLINE_CURVE(2,(#50878,#50879,#50880),.UNSPECIFIED.,.F.,.F.)
B_SPLINE_CURVE_WITH_KNOTS((3,3),(0.,0.00844890352463462),.UNSPECIFIED.)
CURVE()
GEOMETRIC_REPRESENTATION_ITEM()
RATIONAL_B_SPLINE_CURVE((1.,1.00024991830016,1.00030432706346))
REPRESENTATION_ITEM('')
);
#438=(
BOUNDED_CURVE()
B_SPLINE_CURVE(2,(#50884,#50885,#50886),.UNSPECIFIED.,.F.,.F.)
B_SPLINE_CURVE_WITH_KNOTS((3,3),(0.0131514300541893,0.0216003335786744),
 .UNSPECIFIED.)
CURVE()
GEOMETRIC_REPRESENTATION_ITEM()
RATIONAL_B_SPLINE_CURVE((1.00030432706113,1.00024991829825,1.))
REPRESENTATION_ITEM('')
);
#439=(
BOUNDED_CURVE()
B_SPLINE_CURVE(2,(#50899,#50900,#50901),.UNSPECIFIED.,.F.,.F.)
B_SPLINE_CURVE_WITH_KNOTS((3,3),(0.,0.00844890352448517),.UNSPECIFIED.)
CURVE()
GEOMETRIC_REPRESENTATION_ITEM()
RATIONAL_B_SPLINE_CURVE((1.,1.00024991829772,1.00030432706048))
REPRESENTATION_ITEM('')
);
#440=(
BOUNDED_CURVE()
B_SPLINE_CURVE(2,(#50905,#50906,#50907),.UNSPECIFIED.,.F.,.F.)
B_SPLINE_CURVE_WITH_KNOTS((3,3),(0.0131514300541692,0.0216003335786743),
 .UNSPECIFIED.)
CURVE()
GEOMETRIC_REPRESENTATION_ITEM()
RATIONAL_B_SPLINE_CURVE((1.00030432705767,1.00024991829541,1.))
REPRESENTATION_ITEM('')
);
#441=(
BOUNDED_CURVE()
B_SPLINE_CURVE(2,(#50920,#50921,#50922),.UNSPECIFIED.,.F.,.F.)
B_SPLINE_CURVE_WITH_KNOTS((3,3),(0.,0.00844890352459986),.UNSPECIFIED.)
CURVE()
GEOMETRIC_REPRESENTATION_ITEM()
RATIONAL_B_SPLINE_CURVE((1.,1.00024991829621,1.00030432705864))
REPRESENTATION_ITEM('')
);
#442=(
BOUNDED_CURVE()
B_SPLINE_CURVE(2,(#50926,#50927,#50928),.UNSPECIFIED.,.F.,.F.)
B_SPLINE_CURVE_WITH_KNOTS((3,3),(0.0131514300539527,0.0216003335786744),
 .UNSPECIFIED.)
CURVE()
GEOMETRIC_REPRESENTATION_ITEM()
RATIONAL_B_SPLINE_CURVE((1.0003043270617,1.00024991829873,1.))
REPRESENTATION_ITEM('')
);
#443=(
BOUNDED_CURVE()
B_SPLINE_CURVE(2,(#50941,#50942,#50943),.UNSPECIFIED.,.F.,.F.)
B_SPLINE_CURVE_WITH_KNOTS((3,3),(0.,0.00844890352449406),.UNSPECIFIED.)
CURVE()
GEOMETRIC_REPRESENTATION_ITEM()
RATIONAL_B_SPLINE_CURVE((1.,1.00024991829771,1.00030432706047))
REPRESENTATION_ITEM('')
);
#444=(
BOUNDED_CURVE()
B_SPLINE_CURVE(2,(#50947,#50948,#50949),.UNSPECIFIED.,.F.,.F.)
B_SPLINE_CURVE_WITH_KNOTS((3,3),(0.0131514300538891,0.0216003335786743),
 .UNSPECIFIED.)
CURVE()
GEOMETRIC_REPRESENTATION_ITEM()
RATIONAL_B_SPLINE_CURVE((1.00030432705489,1.00024991829313,1.))
REPRESENTATION_ITEM('')
);
#445=(
BOUNDED_CURVE()
B_SPLINE_CURVE(2,(#50962,#50963,#50964),.UNSPECIFIED.,.F.,.F.)
B_SPLINE_CURVE_WITH_KNOTS((3,3),(0.,0.00844890352485641),.UNSPECIFIED.)
CURVE()
GEOMETRIC_REPRESENTATION_ITEM()
RATIONAL_B_SPLINE_CURVE((1.,1.00024991829199,1.0003043270535))
REPRESENTATION_ITEM('')
);
#446=(
BOUNDED_CURVE()
B_SPLINE_CURVE(2,(#50968,#50969,#50970),.UNSPECIFIED.,.F.,.F.)
B_SPLINE_CURVE_WITH_KNOTS((3,3),(0.0131514300537428,0.0216003335786744),
 .UNSPECIFIED.)
CURVE()
GEOMETRIC_REPRESENTATION_ITEM()
RATIONAL_B_SPLINE_CURVE((1.00030432705361,1.00024991829208,1.))
REPRESENTATION_ITEM('')
);
#447=(
BOUNDED_CURVE()
B_SPLINE_CURVE(2,(#50983,#50984,#50985),.UNSPECIFIED.,.F.,.F.)
B_SPLINE_CURVE_WITH_KNOTS((3,3),(0.,0.00844890352496226),.UNSPECIFIED.)
CURVE()
GEOMETRIC_REPRESENTATION_ITEM()
RATIONAL_B_SPLINE_CURVE((1.,1.00024991829658,1.00030432705909))
REPRESENTATION_ITEM('')
);
#448=(
BOUNDED_CURVE()
B_SPLINE_CURVE(2,(#50989,#50990,#50991),.UNSPECIFIED.,.F.,.F.)
B_SPLINE_CURVE_WITH_KNOTS((3,3),(0.013151430054111,0.0216003335786744),
 .UNSPECIFIED.)
CURVE()
GEOMETRIC_REPRESENTATION_ITEM()
RATIONAL_B_SPLINE_CURVE((1.00030432706545,1.0002499183018,1.))
REPRESENTATION_ITEM('')
);
#449=(
BOUNDED_CURVE()
B_SPLINE_CURVE(2,(#51004,#51005,#51006),.UNSPECIFIED.,.F.,.F.)
B_SPLINE_CURVE_WITH_KNOTS((3,3),(0.,0.00844890352465218),.UNSPECIFIED.)
CURVE()
GEOMETRIC_REPRESENTATION_ITEM()
RATIONAL_B_SPLINE_CURVE((1.,1.0002499182964,1.00030432705887))
REPRESENTATION_ITEM('')
);
#450=(
BOUNDED_CURVE()
B_SPLINE_CURVE(2,(#51010,#51011,#51012),.UNSPECIFIED.,.F.,.F.)
B_SPLINE_CURVE_WITH_KNOTS((3,3),(0.0131514300538194,0.0216003335786744),
 .UNSPECIFIED.)
CURVE()
GEOMETRIC_REPRESENTATION_ITEM()
RATIONAL_B_SPLINE_CURVE((1.00030432705442,1.00024991829275,1.))
REPRESENTATION_ITEM('')
);
#451=(
BOUNDED_CURVE()
B_SPLINE_CURVE(2,(#51025,#51026,#51027),.UNSPECIFIED.,.F.,.F.)
B_SPLINE_CURVE_WITH_KNOTS((3,3),(0.,0.00844890352478188),.UNSPECIFIED.)
CURVE()
GEOMETRIC_REPRESENTATION_ITEM()
RATIONAL_B_SPLINE_CURVE((1.,1.00024991829664,1.00030432705917))
REPRESENTATION_ITEM('')
);
#452=(
BOUNDED_CURVE()
B_SPLINE_CURVE(2,(#51031,#51032,#51033),.UNSPECIFIED.,.F.,.F.)
B_SPLINE_CURVE_WITH_KNOTS((3,3),(0.0131514300539186,0.0216003335786744),
 .UNSPECIFIED.)
CURVE()
GEOMETRIC_REPRESENTATION_ITEM()
RATIONAL_B_SPLINE_CURVE((1.00030432706174,1.00024991829875,1.))
REPRESENTATION_ITEM('')
);
#453=(
BOUNDED_CURVE()
B_SPLINE_CURVE(2,(#51046,#51047,#51048),.UNSPECIFIED.,.F.,.F.)
B_SPLINE_CURVE_WITH_KNOTS((3,3),(0.,0.00844890352442994),.UNSPECIFIED.)
CURVE()
GEOMETRIC_REPRESENTATION_ITEM()
RATIONAL_B_SPLINE_CURVE((1.,1.00024991829785,1.00030432706064))
REPRESENTATION_ITEM('')
);
#454=(
BOUNDED_CURVE()
B_SPLINE_CURVE(2,(#51052,#51053,#51054),.UNSPECIFIED.,.F.,.F.)
B_SPLINE_CURVE_WITH_KNOTS((3,3),(0.0131514300540965,0.0216003335786744),
 .UNSPECIFIED.)
CURVE()
GEOMETRIC_REPRESENTATION_ITEM()
RATIONAL_B_SPLINE_CURVE((1.00030432706039,1.00024991829765,1.))
REPRESENTATION_ITEM('')
);
#455=(
BOUNDED_CURVE()
B_SPLINE_CURVE(2,(#51067,#51068,#51069),.UNSPECIFIED.,.F.,.F.)
B_SPLINE_CURVE_WITH_KNOTS((3,3),(0.,0.00844890352481575),.UNSPECIFIED.)
CURVE()
GEOMETRIC_REPRESENTATION_ITEM()
RATIONAL_B_SPLINE_CURVE((1.,1.00024991829544,1.00030432705769))
REPRESENTATION_ITEM('')
);
#456=(
BOUNDED_CURVE()
B_SPLINE_CURVE(2,(#51073,#51074,#51075),.UNSPECIFIED.,.F.,.F.)
B_SPLINE_CURVE_WITH_KNOTS((3,3),(0.0131514300539347,0.0216003335786744),
 .UNSPECIFIED.)
CURVE()
GEOMETRIC_REPRESENTATION_ITEM()
RATIONAL_B_SPLINE_CURVE((1.0003043270581,1.00024991829577,1.))
REPRESENTATION_ITEM('')
);
#457=(
BOUNDED_CURVE()
B_SPLINE_CURVE(2,(#51088,#51089,#51090),.UNSPECIFIED.,.F.,.F.)
B_SPLINE_CURVE_WITH_KNOTS((3,3),(0.,0.00844890352460222),.UNSPECIFIED.)
CURVE()
GEOMETRIC_REPRESENTATION_ITEM()
RATIONAL_B_SPLINE_CURVE((1.,1.00024991829658,1.00030432705909))
REPRESENTATION_ITEM('')
);
#458=(
BOUNDED_CURVE()
B_SPLINE_CURVE(2,(#51094,#51095,#51096),.UNSPECIFIED.,.F.,.F.)
B_SPLINE_CURVE_WITH_KNOTS((3,3),(0.0131514300537623,0.0216003335786744),
 .UNSPECIFIED.)
CURVE()
GEOMETRIC_REPRESENTATION_ITEM()
RATIONAL_B_SPLINE_CURVE((1.00030432705572,1.00024991829381,1.))
REPRESENTATION_ITEM('')
);
#459=(
BOUNDED_CURVE()
B_SPLINE_CURVE(2,(#51109,#51110,#51111),.UNSPECIFIED.,.F.,.F.)
B_SPLINE_CURVE_WITH_KNOTS((3,3),(0.,0.00844890352458545),.UNSPECIFIED.)
CURVE()
GEOMETRIC_REPRESENTATION_ITEM()
RATIONAL_B_SPLINE_CURVE((1.,1.00024991829762,1.00030432706036))
REPRESENTATION_ITEM('')
);
#460=(
BOUNDED_CURVE()
B_SPLINE_CURVE(2,(#51115,#51116,#51117),.UNSPECIFIED.,.F.,.F.)
B_SPLINE_CURVE_WITH_KNOTS((3,3),(0.0131514300540622,0.0216003335786744),
 .UNSPECIFIED.)
CURVE()
GEOMETRIC_REPRESENTATION_ITEM()
RATIONAL_B_SPLINE_CURVE((1.0003043270597,1.00024991829708,1.))
REPRESENTATION_ITEM('')
);
#461=(
BOUNDED_CURVE()
B_SPLINE_CURVE(2,(#51130,#51131,#51132),.UNSPECIFIED.,.F.,.F.)
B_SPLINE_CURVE_WITH_KNOTS((3,3),(0.,0.00844890352449406),.UNSPECIFIED.)
CURVE()
GEOMETRIC_REPRESENTATION_ITEM()
RATIONAL_B_SPLINE_CURVE((1.,1.00024991829771,1.00030432706047))
REPRESENTATION_ITEM('')
);
#462=(
BOUNDED_CURVE()
B_SPLINE_CURVE(2,(#51136,#51137,#51138),.UNSPECIFIED.,.F.,.F.)
B_SPLINE_CURVE_WITH_KNOTS((3,3),(0.0131514300538891,0.0216003335786743),
 .UNSPECIFIED.)
CURVE()
GEOMETRIC_REPRESENTATION_ITEM()
RATIONAL_B_SPLINE_CURVE((1.00030432705489,1.00024991829313,1.))
REPRESENTATION_ITEM('')
);
#463=(
BOUNDED_CURVE()
B_SPLINE_CURVE(2,(#51151,#51152,#51153),.UNSPECIFIED.,.F.,.F.)
B_SPLINE_CURVE_WITH_KNOTS((3,3),(0.,0.00844890352472574),.UNSPECIFIED.)
CURVE()
GEOMETRIC_REPRESENTATION_ITEM()
RATIONAL_B_SPLINE_CURVE((1.,1.00024991829962,1.00030432706279))
REPRESENTATION_ITEM('')
);
#464=(
BOUNDED_CURVE()
B_SPLINE_CURVE(2,(#51157,#51158,#51159),.UNSPECIFIED.,.F.,.F.)
B_SPLINE_CURVE_WITH_KNOTS((3,3),(0.0131514300538617,0.0216003335786744),
 .UNSPECIFIED.)
CURVE()
GEOMETRIC_REPRESENTATION_ITEM()
RATIONAL_B_SPLINE_CURVE((1.00030432705112,1.00024991829003,1.))
REPRESENTATION_ITEM('')
);
#465=(
BOUNDED_CURVE()
B_SPLINE_CURVE(2,(#51212,#51213,#51214),.UNSPECIFIED.,.F.,.F.)
B_SPLINE_CURVE_WITH_KNOTS((3,3),(0.,0.00844890352456175),.UNSPECIFIED.)
CURVE()
GEOMETRIC_REPRESENTATION_ITEM()
RATIONAL_B_SPLINE_CURVE((1.,1.00024991829887,1.00030432706188))
REPRESENTATION_ITEM('')
);
#466=(
BOUNDED_CURVE()
B_SPLINE_CURVE(2,(#51216,#51217,#51218),.UNSPECIFIED.,.F.,.F.)
B_SPLINE_CURVE_WITH_KNOTS((3,3),(0.0131514300541029,0.0216003335786743),
 .UNSPECIFIED.)
CURVE()
GEOMETRIC_REPRESENTATION_ITEM()
RATIONAL_B_SPLINE_CURVE((1.00030432705952,1.00024991829693,1.))
REPRESENTATION_ITEM('')
);
#467=B_SPLINE_SURFACE_WITH_KNOTS('',3,3,((#36405,#36406,#36407,#36408,#36409,
#36410,#36411,#36412,#36413,#36414,#36415,#36416,#36417,#36418,#36419,#36420,
#36421),(#36422,#36423,#36424,#36425,#36426,#36427,#36428,#36429,#36430,
#36431,#36432,#36433,#36434,#36435,#36436,#36437,#36438),(#36439,#36440,
#36441,#36442,#36443,#36444,#36445,#36446,#36447,#36448,#36449,#36450,#36451,
#36452,#36453,#36454,#36455),(#36456,#36457,#36458,#36459,#36460,#36461,
#36462,#36463,#36464,#36465,#36466,#36467,#36468,#36469,#36470,#36471,#36472)),
 .UNSPECIFIED.,.F.,.F.,.F.,(4,4),(4,2,2,2,1,2,2,2,4),(0.,1.),(0.0282690113416936,
0.0484109685685348,0.093261745053174,0.134172257639861,0.175082770226548,
0.215993282813234,0.256903795399921,0.30175457188456,0.321896529111401),
 .UNSPECIFIED.);
#468=B_SPLINE_SURFACE_WITH_KNOTS('',3,3,((#36507,#36508,#36509,#36510,#36511,
#36512,#36513,#36514,#36515,#36516,#36517,#36518,#36519,#36520,#36521,#36522,
#36523,#36524,#36525,#36526,#36527,#36528,#36529,#36530,#36531,#36532,#36533,
#36534,#36535,#36536,#36537,#36538,#36539,#36540),(#36541,#36542,#36543,
#36544,#36545,#36546,#36547,#36548,#36549,#36550,#36551,#36552,#36553,#36554,
#36555,#36556,#36557,#36558,#36559,#36560,#36561,#36562,#36563,#36564,#36565,
#36566,#36567,#36568,#36569,#36570,#36571,#36572,#36573,#36574),(#36575,
#36576,#36577,#36578,#36579,#36580,#36581,#36582,#36583,#36584,#36585,#36586,
#36587,#36588,#36589,#36590,#36591,#36592,#36593,#36594,#36595,#36596,#36597,
#36598,#36599,#36600,#36601,#36602,#36603,#36604,#36605,#36606,#36607,#36608),
(#36609,#36610,#36611,#36612,#36613,#36614,#36615,#36616,#36617,#36618,
#36619,#36620,#36621,#36622,#36623,#36624,#36625,#36626,#36627,#36628,#36629,
#36630,#36631,#36632,#36633,#36634,#36635,#36636,#36637,#36638,#36639,#36640,
#36641,#36642)),.UNSPECIFIED.,.F.,.T.,.F.,(4,4),(4,2,2,2,2,2,2,2,2,2,2,
2,2,2,2,2,4),(0.,1.),(0.,0.0397570154954407,0.0795140309908814,0.119264247282177,
0.159014463573472,0.198764679864768,0.238514896156063,0.278271911651504,
0.318028927146944,0.357785942642385,0.397542958137826,0.437293174429121,
0.477043390720416,0.516793607011712,0.556543823303007,0.596300838798448,
0.636057854293889),.UNSPECIFIED.);
#469=B_SPLINE_SURFACE_WITH_KNOTS('',3,3,((#36833,#36834,#36835,#36836,#36837,
#36838,#36839,#36840,#36841,#36842,#36843,#36844,#36845,#36846,#36847,#36848,
#36849),(#36850,#36851,#36852,#36853,#36854,#36855,#36856,#36857,#36858,
#36859,#36860,#36861,#36862,#36863,#36864,#36865,#36866),(#36867,#36868,
#36869,#36870,#36871,#36872,#36873,#36874,#36875,#36876,#36877,#36878,#36879,
#36880,#36881,#36882,#36883),(#36884,#36885,#36886,#36887,#36888,#36889,
#36890,#36891,#36892,#36893,#36894,#36895,#36896,#36897,#36898,#36899,#36900)),
 .UNSPECIFIED.,.F.,.F.,.F.,(4,4),(4,2,2,2,1,2,2,2,4),(0.,1.),(0.378434551794792,
0.39857650902163,0.443427285506269,0.484337798092956,0.525248310679643,
0.566158823266329,0.607069335853016,0.651920112337657,0.672062069564494),
 .UNSPECIFIED.);
#470=B_SPLINE_SURFACE_WITH_KNOTS('',3,3,((#38097,#38098,#38099,#38100,#38101,
#38102,#38103,#38104,#38105,#38106,#38107,#38108,#38109,#38110,#38111,#38112,
#38113,#38114,#38115,#38116,#38117,#38118,#38119,#38120,#38121,#38122,#38123,
#38124,#38125),(#38126,#38127,#38128,#38129,#38130,#38131,#38132,#38133,
#38134,#38135,#38136,#38137,#38138,#38139,#38140,#38141,#38142,#38143,#38144,
#38145,#38146,#38147,#38148,#38149,#38150,#38151,#38152,#38153,#38154),
(#38155,#38156,#38157,#38158,#38159,#38160,#38161,#38162,#38163,#38164,
#38165,#38166,#38167,#38168,#38169,#38170,#38171,#38172,#38173,#38174,#38175,
#38176,#38177,#38178,#38179,#38180,#38181,#38182,#38183),(#38184,#38185,
#38186,#38187,#38188,#38189,#38190,#38191,#38192,#38193,#38194,#38195,#38196,
#38197,#38198,#38199,#38200,#38201,#38202,#38203,#38204,#38205,#38206,#38207,
#38208,#38209,#38210,#38211,#38212)),.UNSPECIFIED.,.F.,.F.,.F.,(4,4),(4,
1,1,1,1,1,1,1,1,1,1,1,1,1,1,1,1,1,1,1,1,1,1,1,1,1,4),(0.,0.0262983047615875),
(10.0522207760382,11.0378903501899,12.0235599243416,13.0092294984934,13.9948990726451,
14.9805686467968,15.9662382209486,16.9519077951003,17.937577369252,18.9232469434038,
19.9089165175555,20.8945860917073,21.880255665859,22.8659252400107,23.8515948141625,
24.8372643883142,25.8229339624659,26.8086035366177,27.7942731107694,28.7799426849212,
29.7656122590729,30.7512818332246,31.7369514073764,32.7226209815281,33.7082905556798,
34.6939601298316,35.6796297039833),.UNSPECIFIED.);
#471=B_SPLINE_SURFACE_WITH_KNOTS('',3,3,((#38342,#38343,#38344,#38345,#38346,
#38347,#38348,#38349,#38350,#38351,#38352,#38353,#38354,#38355,#38356,#38357,
#38358,#38359,#38360,#38361,#38362,#38363,#38364,#38365,#38366,#38367,#38368,
#38369,#38370),(#38371,#38372,#38373,#38374,#38375,#38376,#38377,#38378,
#38379,#38380,#38381,#38382,#38383,#38384,#38385,#38386,#38387,#38388,#38389,
#38390,#38391,#38392,#38393,#38394,#38395,#38396,#38397,#38398,#38399),
(#38400,#38401,#38402,#38403,#38404,#38405,#38406,#38407,#38408,#38409,
#38410,#38411,#38412,#38413,#38414,#38415,#38416,#38417,#38418,#38419,#38420,
#38421,#38422,#38423,#38424,#38425,#38426,#38427,#38428),(#38429,#38430,
#38431,#38432,#38433,#38434,#38435,#38436,#38437,#38438,#38439,#38440,#38441,
#38442,#38443,#38444,#38445,#38446,#38447,#38448,#38449,#38450,#38451,#38452,
#38453,#38454,#38455,#38456,#38457)),.UNSPECIFIED.,.F.,.F.,.F.,(4,4),(4,
1,1,1,1,1,1,1,1,1,1,1,1,1,1,1,1,1,1,1,1,1,1,1,1,1,4),(0.,0.0262983047615875),
(13.3593226216143,14.3449921957661,15.3306617699178,16.3163313440695,17.3020009182213,
18.287670492373,19.2733400665247,20.2590096406765,21.2446792148282,22.23034878898,
23.2160183631317,24.2016879372834,25.1873575114352,26.1730270855869,27.1586966597386,
28.1443662338904,29.1300358080421,30.1157053821939,31.1013749563456,32.0870445304973,
33.0727141046491,34.0583836788008,35.0440532529525,36.0297228271043,37.015392401256,
38.0010619754078,38.9867315495595),.UNSPECIFIED.);
#472=B_SPLINE_SURFACE_WITH_KNOTS('',3,3,((#39118,#39119,#39120,#39121,#39122,
#39123,#39124,#39125,#39126,#39127,#39128,#39129,#39130,#39131,#39132,#39133,
#39134,#39135,#39136,#39137,#39138,#39139,#39140,#39141,#39142,#39143,#39144,
#39145,#39146,#39147,#39148,#39149,#39150,#39151,#39152,#39153,#39154,#39155,
#39156,#39157,#39158,#39159,#39160,#39161,#39162,#39163,#39164,#39165,#39166,
#39167,#39168,#39169,#39170,#39171,#39172,#39173),(#39174,#39175,#39176,
#39177,#39178,#39179,#39180,#39181,#39182,#39183,#39184,#39185,#39186,#39187,
#39188,#39189,#39190,#39191,#39192,#39193,#39194,#39195,#39196,#39197,#39198,
#39199,#39200,#39201,#39202,#39203,#39204,#39205,#39206,#39207,#39208,#39209,
#39210,#39211,#39212,#39213,#39214,#39215,#39216,#39217,#39218,#39219,#39220,
#39221,#39222,#39223,#39224,#39225,#39226,#39227,#39228,#39229),(#39230,
#39231,#39232,#39233,#39234,#39235,#39236,#39237,#39238,#39239,#39240,#39241,
#39242,#39243,#39244,#39245,#39246,#39247,#39248,#39249,#39250,#39251,#39252,
#39253,#39254,#39255,#39256,#39257,#39258,#39259,#39260,#39261,#39262,#39263,
#39264,#39265,#39266,#39267,#39268,#39269,#39270,#39271,#39272,#39273,#39274,
#39275,#39276,#39277,#39278,#39279,#39280,#39281,#39282,#39283,#39284,#39285),
(#39286,#39287,#39288,#39289,#39290,#39291,#39292,#39293,#39294,#39295,
#39296,#39297,#39298,#39299,#39300,#39301,#39302,#39303,#39304,#39305,#39306,
#39307,#39308,#39309,#39310,#39311,#39312,#39313,#39314,#39315,#39316,#39317,
#39318,#39319,#39320,#39321,#39322,#39323,#39324,#39325,#39326,#39327,#39328,
#39329,#39330,#39331,#39332,#39333,#39334,#39335,#39336,#39337,#39338,#39339,
#39340,#39341)),.UNSPECIFIED.,.F.,.F.,.F.,(4,4),(4,1,1,1,1,1,1,1,1,1,1,
1,1,1,1,1,1,1,1,1,1,1,1,1,1,1,1,1,1,1,1,1,1,1,1,1,1,1,1,1,1,1,1,1,1,1,1,
1,1,1,1,1,1,4),(0.,0.0296469363228873),(11.5874873465742,12.5749444987495,
13.5624016509248,14.5498588031001,15.5373159552754,16.5247731074507,17.512230259626,
18.4996874118013,19.4871445639766,20.4746017161519,21.4620588683272,22.4495160205025,
23.4369731726778,24.4244303248531,25.4118874770284,26.3993446292037,27.386801781379,
28.3742589335543,29.3617160857296,30.3491732379048,31.3366303900801,32.3240875422554,
33.3115446944307,34.299001846606,35.2864589987813,36.2739161509566,37.2613733031319,
38.2488304553072,39.2362876074825,40.2237447596578,41.2112019118331,42.1986590640084,
43.1861162161837,44.173573368359,45.1610305205343,46.1484876727096,47.1359448248849,
48.1234019770602,49.1108591292355,50.0983162814107,51.085773433586,52.0732305857613,
53.0606877379366,54.0481448901119,55.0356020422872,56.0230591944625,57.0105163466378,
57.9979734988131,58.9854306509884,59.9728878031637,60.960344955339,61.9478021075143,
62.9352592596896,63.9227164118649),.UNSPECIFIED.);
#473=B_SPLINE_SURFACE_WITH_KNOTS('',3,3,((#39515,#39516,#39517,#39518,#39519,
#39520,#39521,#39522,#39523,#39524,#39525,#39526,#39527,#39528,#39529,#39530,
#39531,#39532,#39533,#39534,#39535,#39536,#39537,#39538,#39539,#39540,#39541,
#39542,#39543,#39544,#39545,#39546,#39547,#39548,#39549,#39550,#39551,#39552,
#39553,#39554,#39555,#39556,#39557,#39558,#39559,#39560,#39561,#39562,#39563,
#39564,#39565,#39566,#39567,#39568,#39569,#39570),(#39571,#39572,#39573,
#39574,#39575,#39576,#39577,#39578,#39579,#39580,#39581,#39582,#39583,#39584,
#39585,#39586,#39587,#39588,#39589,#39590,#39591,#39592,#39593,#39594,#39595,
#39596,#39597,#39598,#39599,#39600,#39601,#39602,#39603,#39604,#39605,#39606,
#39607,#39608,#39609,#39610,#39611,#39612,#39613,#39614,#39615,#39616,#39617,
#39618,#39619,#39620,#39621,#39622,#39623,#39624,#39625,#39626),(#39627,
#39628,#39629,#39630,#39631,#39632,#39633,#39634,#39635,#39636,#39637,#39638,
#39639,#39640,#39641,#39642,#39643,#39644,#39645,#39646,#39647,#39648,#39649,
#39650,#39651,#39652,#39653,#39654,#39655,#39656,#39657,#39658,#39659,#39660,
#39661,#39662,#39663,#39664,#39665,#39666,#39667,#39668,#39669,#39670,#39671,
#39672,#39673,#39674,#39675,#39676,#39677,#39678,#39679,#39680,#39681,#39682),
(#39683,#39684,#39685,#39686,#39687,#39688,#39689,#39690,#39691,#39692,
#39693,#39694,#39695,#39696,#39697,#39698,#39699,#39700,#39701,#39702,#39703,
#39704,#39705,#39706,#39707,#39708,#39709,#39710,#39711,#39712,#39713,#39714,
#39715,#39716,#39717,#39718,#39719,#39720,#39721,#39722,#39723,#39724,#39725,
#39726,#39727,#39728,#39729,#39730,#39731,#39732,#39733,#39734,#39735,#39736,
#39737,#39738)),.UNSPECIFIED.,.F.,.F.,.F.,(4,4),(4,1,1,1,1,1,1,1,1,1,1,
1,1,1,1,1,1,1,1,1,1,1,1,1,1,1,1,1,1,1,1,1,1,1,1,1,1,1,1,1,1,1,1,1,1,1,1,
1,1,1,1,1,1,4),(0.,0.0296469363228873),(14.896352608199,15.8838097603743,
16.8712669125496,17.8587240647249,18.8461812169001,19.8336383690754,20.8210955212507,
21.808552673426,22.7960098256013,23.7834669777766,24.7709241299519,25.7583812821272,
26.7458384343025,27.7332955864778,28.7207527386531,29.7082098908284,30.6956670430037,
31.683124195179,32.6705813473543,33.6580384995296,34.6454956517049,35.6329528038802,
36.6204099560555,37.6078671082307,38.595324260406,39.5827814125813,40.5702385647566,
41.5576957169319,42.5451528691072,43.5326100212825,44.5200671734578,45.5075243256331,
46.4949814778084,47.4824386299837,48.469895782159,49.4573529343343,50.4448100865096,
51.4322672386849,52.4197243908602,53.4071815430355,54.3946386952108,55.3820958473861,
56.3695529995614,57.3570101517367,58.3444673039119,59.3319244560872,60.3193816082625,
61.3068387604378,62.2942959126131,63.2817530647884,64.2692102169637,65.256667369139,
66.2441245213143,67.2315816734896),.UNSPECIFIED.);
#474=B_SPLINE_SURFACE_WITH_KNOTS('',3,3,((#42155,#42156,#42157,#42158,#42159,
#42160,#42161,#42162,#42163,#42164,#42165,#42166,#42167,#42168,#42169,#42170,
#42171,#42172,#42173,#42174,#42175,#42176,#42177,#42178,#42179,#42180,#42181,
#42182,#42183,#42184,#42185,#42186,#42187,#42188,#42189,#42190,#42191,#42192,
#42193,#42194,#42195,#42196,#42197,#42198,#42199,#42200,#42201,#42202,#42203,
#42204,#42205,#42206,#42207,#42208,#42209,#42210,#42211,#42212,#42213,#42214,
#42215,#42216,#42217,#42218,#42219,#42220,#42221,#42222,#42223,#42224,#42225,
#42226,#42227,#42228,#42229,#42230,#42231,#42232,#42233,#42234,#42235,#42236,
#42237,#42238,#42239,#42240,#42241,#42242,#42243,#42244,#42245,#42246,#42247,
#42248,#42249,#42250,#42251,#42252,#42253,#42254,#42255,#42256,#42257,#42258,
#42259,#42260,#42261,#42262,#42263,#42264,#42265,#42266,#42267,#42268,#42269,
#42270,#42271,#42272,#42273,#42274,#42275,#42276,#42277,#42278,#42279,#42280,
#42281,#42282,#42283,#42284,#42285,#42286,#42287,#42288,#42289,#42290,#42291,
#42292,#42293,#42294,#42295,#42296,#42297,#42298,#42299,#42300,#42301,#42302,
#42303,#42304,#42305,#42306,#42307,#42308,#42309,#42310,#42311,#42312,#42313,
#42314,#42315,#42316,#42317,#42318,#42319,#42320,#42321,#42322,#42323,#42324,
#42325,#42326,#42327,#42328,#42329,#42330,#42331,#42332,#42333,#42334,#42335,
#42336,#42337,#42338),(#42339,#42340,#42341,#42342,#42343,#42344,#42345,
#42346,#42347,#42348,#42349,#42350,#42351,#42352,#42353,#42354,#42355,#42356,
#42357,#42358,#42359,#42360,#42361,#42362,#42363,#42364,#42365,#42366,#42367,
#42368,#42369,#42370,#42371,#42372,#42373,#42374,#42375,#42376,#42377,#42378,
#42379,#42380,#42381,#42382,#42383,#42384,#42385,#42386,#42387,#42388,#42389,
#42390,#42391,#42392,#42393,#42394,#42395,#42396,#42397,#42398,#42399,#42400,
#42401,#42402,#42403,#42404,#42405,#42406,#42407,#42408,#42409,#42410,#42411,
#42412,#42413,#42414,#42415,#42416,#42417,#42418,#42419,#42420,#42421,#42422,
#42423,#42424,#42425,#42426,#42427,#42428,#42429,#42430,#42431,#42432,#42433,
#42434,#42435,#42436,#42437,#42438,#42439,#42440,#42441,#42442,#42443,#42444,
#42445,#42446,#42447,#42448,#42449,#42450,#42451,#42452,#42453,#42454,#42455,
#42456,#42457,#42458,#42459,#42460,#42461,#42462,#42463,#42464,#42465,#42466,
#42467,#42468,#42469,#42470,#42471,#42472,#42473,#42474,#42475,#42476,#42477,
#42478,#42479,#42480,#42481,#42482,#42483,#42484,#42485,#42486,#42487,#42488,
#42489,#42490,#42491,#42492,#42493,#42494,#42495,#42496,#42497,#42498,#42499,
#42500,#42501,#42502,#42503,#42504,#42505,#42506,#42507,#42508,#42509,#42510,
#42511,#42512,#42513,#42514,#42515,#42516,#42517,#42518,#42519,#42520,#42521,
#42522),(#42523,#42524,#42525,#42526,#42527,#42528,#42529,#42530,#42531,
#42532,#42533,#42534,#42535,#42536,#42537,#42538,#42539,#42540,#42541,#42542,
#42543,#42544,#42545,#42546,#42547,#42548,#42549,#42550,#42551,#42552,#42553,
#42554,#42555,#42556,#42557,#42558,#42559,#42560,#42561,#42562,#42563,#42564,
#42565,#42566,#42567,#42568,#42569,#42570,#42571,#42572,#42573,#42574,#42575,
#42576,#42577,#42578,#42579,#42580,#42581,#42582,#42583,#42584,#42585,#42586,
#42587,#42588,#42589,#42590,#42591,#42592,#42593,#42594,#42595,#42596,#42597,
#42598,#42599,#42600,#42601,#42602,#42603,#42604,#42605,#42606,#42607,#42608,
#42609,#42610,#42611,#42612,#42613,#42614,#42615,#42616,#42617,#42618,#42619,
#42620,#42621,#42622,#42623,#42624,#42625,#42626,#42627,#42628,#42629,#42630,
#42631,#42632,#42633,#42634,#42635,#42636,#42637,#42638,#42639,#42640,#42641,
#42642,#42643,#42644,#42645,#42646,#42647,#42648,#42649,#42650,#42651,#42652,
#42653,#42654,#42655,#42656,#42657,#42658,#42659,#42660,#42661,#42662,#42663,
#42664,#42665,#42666,#42667,#42668,#42669,#42670,#42671,#42672,#42673,#42674,
#42675,#42676,#42677,#42678,#42679,#42680,#42681,#42682,#42683,#42684,#42685,
#42686,#42687,#42688,#42689,#42690,#42691,#42692,#42693,#42694,#42695,#42696,
#42697,#42698,#42699,#42700,#42701,#42702,#42703,#42704,#42705,#42706),
(#42707,#42708,#42709,#42710,#42711,#42712,#42713,#42714,#42715,#42716,
#42717,#42718,#42719,#42720,#42721,#42722,#42723,#42724,#42725,#42726,#42727,
#42728,#42729,#42730,#42731,#42732,#42733,#42734,#42735,#42736,#42737,#42738,
#42739,#42740,#42741,#42742,#42743,#42744,#42745,#42746,#42747,#42748,#42749,
#42750,#42751,#42752,#42753,#42754,#42755,#42756,#42757,#42758,#42759,#42760,
#42761,#42762,#42763,#42764,#42765,#42766,#42767,#42768,#42769,#42770,#42771,
#42772,#42773,#42774,#42775,#42776,#42777,#42778,#42779,#42780,#42781,#42782,
#42783,#42784,#42785,#42786,#42787,#42788,#42789,#42790,#42791,#42792,#42793,
#42794,#42795,#42796,#42797,#42798,#42799,#42800,#42801,#42802,#42803,#42804,
#42805,#42806,#42807,#42808,#42809,#42810,#42811,#42812,#42813,#42814,#42815,
#42816,#42817,#42818,#42819,#42820,#42821,#42822,#42823,#42824,#42825,#42826,
#42827,#42828,#42829,#42830,#42831,#42832,#42833,#42834,#42835,#42836,#42837,
#42838,#42839,#42840,#42841,#42842,#42843,#42844,#42845,#42846,#42847,#42848,
#42849,#42850,#42851,#42852,#42853,#42854,#42855,#42856,#42857,#42858,#42859,
#42860,#42861,#42862,#42863,#42864,#42865,#42866,#42867,#42868,#42869,#42870,
#42871,#42872,#42873,#42874,#42875,#42876,#42877,#42878,#42879,#42880,#42881,
#42882,#42883,#42884,#42885,#42886,#42887,#42888,#42889,#42890)),
 .UNSPECIFIED.,.F.,.F.,.F.,(4,4),(4,1,1,1,1,1,1,1,1,1,1,1,1,1,1,1,1,1,1,
1,1,1,1,1,1,1,1,1,1,1,1,1,1,1,1,1,1,1,1,1,1,1,1,1,1,1,1,1,1,1,1,1,1,1,1,
1,1,1,1,1,1,1,1,1,1,1,1,1,1,1,1,1,1,1,1,1,1,1,1,1,1,1,1,1,1,1,1,1,1,1,1,
1,1,1,1,1,1,1,1,1,1,1,1,1,1,1,1,1,1,1,1,1,1,1,1,1,1,1,1,1,1,1,1,1,1,1,1,
1,1,1,1,1,1,1,1,1,1,1,1,1,1,1,1,1,1,1,1,1,1,1,1,1,1,1,1,1,1,1,1,1,1,1,1,
1,1,1,1,1,1,1,1,1,1,1,1,1,1,1,1,1,1,4),(0.,0.0262983047615874),(13.0216803321501,
14.0189616954093,15.0162430586686,16.0135244219278,17.010805785187,18.0080871484463,
19.0053685117055,20.0026498749647,20.999931238224,21.9972126014832,22.9944939647424,
23.9917753280017,24.9890566912609,25.9863380545202,26.9836194177794,27.9809007810386,
28.9781821442979,29.9754635075571,30.9727448708163,31.9700262340756,32.9673075973348,
33.9645889605941,34.9618703238533,35.9591516871125,36.9564330503718,37.953714413631,
38.9509957768902,39.9482771401495,40.9455585034087,41.942839866668,42.9401212299272,
43.9374025931864,44.9346839564457,45.9319653197049,46.9292466829641,47.9265280462234,
48.9238094094826,49.9210907727419,50.9183721360011,51.9156534992603,52.9129348625196,
53.9102162257788,54.907497589038,55.9047789522973,56.9020603155565,57.8993416788158,
58.896623042075,59.8939044053342,60.8911857685935,61.8884671318527,62.8857484951119,
63.8830298583712,64.8803112216304,65.8775925848897,66.8748739481489,67.8721553114081,
68.8694366746674,69.8667180379266,70.8639994011859,71.8612807644451,72.8585621277043,
73.8558434909636,74.8531248542228,75.850406217482,76.8476875807413,77.8449689440005,
78.8422503072597,79.839531670519,80.8368130337782,81.8340943970375,82.8313757602967,
83.8286571235559,84.8259384868152,85.8232198500744,86.8205012133336,87.8177825765929,
88.8150639398521,89.8123453031114,90.8096266663706,91.8069080296298,92.8041893928891,
93.8014707561483,94.7987521194075,95.7960334826668,96.793314845926,97.7905962091853,
98.7878775724445,99.7851589357037,100.782440298963,101.779721662222,102.777003025481,
103.774284388741,104.771565752,105.768847115259,106.766128478518,107.763409841778,
108.760691205037,109.757972568296,110.755253931555,111.752535294815,112.749816658074,
113.747098021333,114.744379384592,115.741660747852,116.738942111111,117.73622347437,
118.733504837629,119.730786200888,120.728067564148,121.725348927407,122.722630290666,
123.719911653925,124.717193017185,125.714474380444,126.711755743703,127.709037106962,
128.706318470222,129.703599833481,130.70088119674,131.698162559999,132.695443923259,
133.692725286518,134.690006649777,135.687288013036,136.684569376296,137.681850739555,
138.679132102814,139.676413466073,140.673694829332,141.670976192592,142.668257555851,
143.66553891911,144.662820282369,145.660101645629,146.657383008888,147.654664372147,
148.651945735406,149.649227098666,150.646508461925,151.643789825184,152.641071188443,
153.638352551703,154.635633914962,155.632915278221,156.63019664148,157.627478004739,
158.624759367999,159.622040731258,160.619322094517,161.616603457776,162.613884821036,
163.611166184295,164.608447547554,165.605728910813,166.603010274073,167.600291637332,
168.597573000591,169.59485436385,170.59213572711,171.589417090369,172.586698453628,
173.583979816887,174.581261180147,175.578542543406,176.575823906665,177.573105269924,
178.570386633183,179.567667996443,180.564949359702,181.562230722961,182.55951208622,
183.55679344948,184.554074812739,185.551356175998,186.548637539257,187.545918902517,
188.543200265776,189.540481629035,190.537762992294,191.535044355554,192.532325718813,
193.529607082072),.UNSPECIFIED.);
#475=B_SPLINE_SURFACE_WITH_KNOTS('',3,3,((#43016,#43017,#43018,#43019,#43020,
#43021,#43022,#43023,#43024,#43025,#43026,#43027,#43028,#43029,#43030,#43031,
#43032,#43033,#43034,#43035,#43036,#43037,#43038,#43039,#43040,#43041,#43042,
#43043,#43044,#43045,#43046,#43047,#43048,#43049,#43050,#43051,#43052,#43053,
#43054,#43055,#43056,#43057,#43058,#43059,#43060,#43061,#43062,#43063,#43064,
#43065,#43066,#43067,#43068,#43069,#43070,#43071,#43072,#43073,#43074,#43075,
#43076,#43077,#43078,#43079,#43080,#43081,#43082,#43083,#43084,#43085,#43086,
#43087,#43088,#43089,#43090,#43091,#43092,#43093,#43094,#43095,#43096,#43097,
#43098,#43099,#43100,#43101,#43102,#43103,#43104,#43105,#43106,#43107,#43108,
#43109,#43110,#43111,#43112,#43113,#43114,#43115,#43116,#43117,#43118,#43119,
#43120,#43121,#43122,#43123,#43124,#43125,#43126,#43127,#43128,#43129,#43130,
#43131,#43132,#43133,#43134,#43135,#43136,#43137,#43138,#43139,#43140,#43141,
#43142,#43143,#43144,#43145,#43146,#43147,#43148,#43149,#43150,#43151,#43152,
#43153,#43154,#43155,#43156,#43157,#43158,#43159,#43160,#43161,#43162,#43163,
#43164,#43165,#43166,#43167,#43168,#43169,#43170,#43171,#43172,#43173,#43174,
#43175,#43176,#43177,#43178,#43179,#43180,#43181,#43182,#43183,#43184,#43185,
#43186,#43187,#43188,#43189,#43190,#43191,#43192,#43193,#43194,#43195,#43196,
#43197,#43198,#43199),(#43200,#43201,#43202,#43203,#43204,#43205,#43206,
#43207,#43208,#43209,#43210,#43211,#43212,#43213,#43214,#43215,#43216,#43217,
#43218,#43219,#43220,#43221,#43222,#43223,#43224,#43225,#43226,#43227,#43228,
#43229,#43230,#43231,#43232,#43233,#43234,#43235,#43236,#43237,#43238,#43239,
#43240,#43241,#43242,#43243,#43244,#43245,#43246,#43247,#43248,#43249,#43250,
#43251,#43252,#43253,#43254,#43255,#43256,#43257,#43258,#43259,#43260,#43261,
#43262,#43263,#43264,#43265,#43266,#43267,#43268,#43269,#43270,#43271,#43272,
#43273,#43274,#43275,#43276,#43277,#43278,#43279,#43280,#43281,#43282,#43283,
#43284,#43285,#43286,#43287,#43288,#43289,#43290,#43291,#43292,#43293,#43294,
#43295,#43296,#43297,#43298,#43299,#43300,#43301,#43302,#43303,#43304,#43305,
#43306,#43307,#43308,#43309,#43310,#43311,#43312,#43313,#43314,#43315,#43316,
#43317,#43318,#43319,#43320,#43321,#43322,#43323,#43324,#43325,#43326,#43327,
#43328,#43329,#43330,#43331,#43332,#43333,#43334,#43335,#43336,#43337,#43338,
#43339,#43340,#43341,#43342,#43343,#43344,#43345,#43346,#43347,#43348,#43349,
#43350,#43351,#43352,#43353,#43354,#43355,#43356,#43357,#43358,#43359,#43360,
#43361,#43362,#43363,#43364,#43365,#43366,#43367,#43368,#43369,#43370,#43371,
#43372,#43373,#43374,#43375,#43376,#43377,#43378,#43379,#43380,#43381,#43382,
#43383),(#43384,#43385,#43386,#43387,#43388,#43389,#43390,#43391,#43392,
#43393,#43394,#43395,#43396,#43397,#43398,#43399,#43400,#43401,#43402,#43403,
#43404,#43405,#43406,#43407,#43408,#43409,#43410,#43411,#43412,#43413,#43414,
#43415,#43416,#43417,#43418,#43419,#43420,#43421,#43422,#43423,#43424,#43425,
#43426,#43427,#43428,#43429,#43430,#43431,#43432,#43433,#43434,#43435,#43436,
#43437,#43438,#43439,#43440,#43441,#43442,#43443,#43444,#43445,#43446,#43447,
#43448,#43449,#43450,#43451,#43452,#43453,#43454,#43455,#43456,#43457,#43458,
#43459,#43460,#43461,#43462,#43463,#43464,#43465,#43466,#43467,#43468,#43469,
#43470,#43471,#43472,#43473,#43474,#43475,#43476,#43477,#43478,#43479,#43480,
#43481,#43482,#43483,#43484,#43485,#43486,#43487,#43488,#43489,#43490,#43491,
#43492,#43493,#43494,#43495,#43496,#43497,#43498,#43499,#43500,#43501,#43502,
#43503,#43504,#43505,#43506,#43507,#43508,#43509,#43510,#43511,#43512,#43513,
#43514,#43515,#43516,#43517,#43518,#43519,#43520,#43521,#43522,#43523,#43524,
#43525,#43526,#43527,#43528,#43529,#43530,#43531,#43532,#43533,#43534,#43535,
#43536,#43537,#43538,#43539,#43540,#43541,#43542,#43543,#43544,#43545,#43546,
#43547,#43548,#43549,#43550,#43551,#43552,#43553,#43554,#43555,#43556,#43557,
#43558,#43559,#43560,#43561,#43562,#43563,#43564,#43565,#43566,#43567),
(#43568,#43569,#43570,#43571,#43572,#43573,#43574,#43575,#43576,#43577,
#43578,#43579,#43580,#43581,#43582,#43583,#43584,#43585,#43586,#43587,#43588,
#43589,#43590,#43591,#43592,#43593,#43594,#43595,#43596,#43597,#43598,#43599,
#43600,#43601,#43602,#43603,#43604,#43605,#43606,#43607,#43608,#43609,#43610,
#43611,#43612,#43613,#43614,#43615,#43616,#43617,#43618,#43619,#43620,#43621,
#43622,#43623,#43624,#43625,#43626,#43627,#43628,#43629,#43630,#43631,#43632,
#43633,#43634,#43635,#43636,#43637,#43638,#43639,#43640,#43641,#43642,#43643,
#43644,#43645,#43646,#43647,#43648,#43649,#43650,#43651,#43652,#43653,#43654,
#43655,#43656,#43657,#43658,#43659,#43660,#43661,#43662,#43663,#43664,#43665,
#43666,#43667,#43668,#43669,#43670,#43671,#43672,#43673,#43674,#43675,#43676,
#43677,#43678,#43679,#43680,#43681,#43682,#43683,#43684,#43685,#43686,#43687,
#43688,#43689,#43690,#43691,#43692,#43693,#43694,#43695,#43696,#43697,#43698,
#43699,#43700,#43701,#43702,#43703,#43704,#43705,#43706,#43707,#43708,#43709,
#43710,#43711,#43712,#43713,#43714,#43715,#43716,#43717,#43718,#43719,#43720,
#43721,#43722,#43723,#43724,#43725,#43726,#43727,#43728,#43729,#43730,#43731,
#43732,#43733,#43734,#43735,#43736,#43737,#43738,#43739,#43740,#43741,#43742,
#43743,#43744,#43745,#43746,#43747,#43748,#43749,#43750,#43751)),
 .UNSPECIFIED.,.F.,.F.,.F.,(4,4),(4,1,1,1,1,1,1,1,1,1,1,1,1,1,1,1,1,1,1,
1,1,1,1,1,1,1,1,1,1,1,1,1,1,1,1,1,1,1,1,1,1,1,1,1,1,1,1,1,1,1,1,1,1,1,1,
1,1,1,1,1,1,1,1,1,1,1,1,1,1,1,1,1,1,1,1,1,1,1,1,1,1,1,1,1,1,1,1,1,1,1,1,
1,1,1,1,1,1,1,1,1,1,1,1,1,1,1,1,1,1,1,1,1,1,1,1,1,1,1,1,1,1,1,1,1,1,1,1,
1,1,1,1,1,1,1,1,1,1,1,1,1,1,1,1,1,1,1,1,1,1,1,1,1,1,1,1,1,1,1,1,1,1,1,1,
1,1,1,1,1,1,1,1,1,1,1,1,1,1,1,1,1,1,4),(0.,0.0262983047615874),(16.3287821777263,
17.3260635409855,18.3233449042448,19.320626267504,20.3179076307632,21.3151889940225,
22.3124703572817,23.3097517205409,24.3070330838002,25.3043144470594,26.3015958103187,
27.2988771735779,28.2961585368371,29.2934399000964,30.2907212633556,31.2880026266148,
32.2852839898741,33.2825653531333,34.2798467163926,35.2771280796518,36.274409442911,
37.2716908061703,38.2689721694295,39.2662535326887,40.263534895948,41.2608162592072,
42.2580976224665,43.2553789857257,44.2526603489849,45.2499417122442,46.2472230755034,
47.2445044387626,48.2417858020219,49.2390671652811,50.2363485285403,51.2336298917996,
52.2309112550588,53.2281926183181,54.2254739815773,55.2227553448365,56.2200367080958,
57.217318071355,58.2145994346142,59.2118807978735,60.2091621611327,61.206443524392,
62.2037248876512,63.2010062509104,64.1982876141697,65.1955689774289,66.1928503406881,
67.1901317039474,68.1874130672066,69.1846944304658,70.1819757937251,71.1792571569843,
72.1765385202436,73.1738198835028,74.171101246762,75.1683826100213,76.1656639732805,
77.1629453365397,78.160226699799,79.1575080630582,80.1547894263174,81.1520707895767,
82.1493521528359,83.1466335160952,84.1439148793544,85.1411962426136,86.1384776058729,
87.1357589691321,88.1330403323914,89.1303216956506,90.1276030589098,91.1248844221691,
92.1221657854283,93.1194471486875,94.1167285119468,95.114009875206,96.1112912384653,
97.1085726017245,98.1058539649837,99.103135328243,100.100416691502,101.097698054761,
102.094979418021,103.09226078128,104.089542144539,105.086823507798,106.084104871058,
107.081386234317,108.078667597576,109.075948960835,110.073230324095,111.070511687354,
112.067793050613,113.065074413872,114.062355777132,115.059637140391,116.05691850365,
117.054199866909,118.051481230168,119.048762593428,120.046043956687,121.043325319946,
122.040606683205,123.037888046465,124.035169409724,125.032450772983,126.029732136242,
127.027013499502,128.024294862761,129.02157622602,130.018857589279,131.016138952539,
132.013420315798,133.010701679057,134.007983042316,135.005264405576,136.002545768835,
136.999827132094,137.997108495353,138.994389858612,139.991671221872,140.988952585131,
141.98623394839,142.983515311649,143.980796674909,144.978078038168,145.975359401427,
146.972640764686,147.969922127946,148.967203491205,149.964484854464,150.961766217723,
151.959047580983,152.956328944242,153.953610307501,154.95089167076,155.948173034019,
156.945454397279,157.942735760538,158.940017123797,159.937298487056,160.934579850316,
161.931861213575,162.929142576834,163.926423940093,164.923705303353,165.920986666612,
166.918268029871,167.91554939313,168.91283075639,169.910112119649,170.907393482908,
171.904674846167,172.901956209427,173.899237572686,174.896518935945,175.893800299204,
176.891081662463,177.888363025723,178.885644388982,179.882925752241,180.8802071155,
181.87748847876,182.874769842019,183.872051205278,184.869332568537,185.866613931797,
186.863895295056,187.861176658315,188.858458021574,189.855739384834,190.853020748093,
191.850302111352,192.847583474611,193.84486483787,194.84214620113,195.839427564389,
196.836708927648),.UNSPECIFIED.);
#476=B_SPLINE_SURFACE_WITH_KNOTS('',3,3,((#46447,#46448,#46449,#46450,#46451,
#46452,#46453,#46454,#46455,#46456,#46457,#46458,#46459,#46460,#46461,#46462,
#46463,#46464,#46465,#46466,#46467,#46468,#46469,#46470,#46471,#46472,#46473,
#46474,#46475,#46476,#46477,#46478,#46479,#46480,#46481,#46482,#46483,#46484,
#46485,#46486,#46487,#46488,#46489,#46490,#46491,#46492,#46493,#46494,#46495,
#46496,#46497,#46498,#46499,#46500,#46501,#46502,#46503,#46504,#46505,#46506,
#46507,#46508,#46509,#46510,#46511,#46512,#46513,#46514,#46515,#46516,#46517,
#46518,#46519,#46520,#46521,#46522,#46523,#46524,#46525,#46526,#46527,#46528,
#46529,#46530,#46531,#46532,#46533,#46534,#46535,#46536,#46537,#46538,#46539,
#46540,#46541,#46542,#46543,#46544,#46545,#46546,#46547,#46548,#46549,#46550,
#46551,#46552,#46553,#46554,#46555,#46556,#46557,#46558,#46559,#46560,#46561,
#46562,#46563,#46564,#46565,#46566,#46567,#46568,#46569,#46570,#46571,#46572,
#46573,#46574,#46575,#46576,#46577,#46578,#46579,#46580,#46581,#46582,#46583,
#46584,#46585,#46586,#46587,#46588,#46589,#46590,#46591,#46592,#46593,#46594,
#46595,#46596,#46597,#46598,#46599),(#46600,#46601,#46602,#46603,#46604,
#46605,#46606,#46607,#46608,#46609,#46610,#46611,#46612,#46613,#46614,#46615,
#46616,#46617,#46618,#46619,#46620,#46621,#46622,#46623,#46624,#46625,#46626,
#46627,#46628,#46629,#46630,#46631,#46632,#46633,#46634,#46635,#46636,#46637,
#46638,#46639,#46640,#46641,#46642,#46643,#46644,#46645,#46646,#46647,#46648,
#46649,#46650,#46651,#46652,#46653,#46654,#46655,#46656,#46657,#46658,#46659,
#46660,#46661,#46662,#46663,#46664,#46665,#46666,#46667,#46668,#46669,#46670,
#46671,#46672,#46673,#46674,#46675,#46676,#46677,#46678,#46679,#46680,#46681,
#46682,#46683,#46684,#46685,#46686,#46687,#46688,#46689,#46690,#46691,#46692,
#46693,#46694,#46695,#46696,#46697,#46698,#46699,#46700,#46701,#46702,#46703,
#46704,#46705,#46706,#46707,#46708,#46709,#46710,#46711,#46712,#46713,#46714,
#46715,#46716,#46717,#46718,#46719,#46720,#46721,#46722,#46723,#46724,#46725,
#46726,#46727,#46728,#46729,#46730,#46731,#46732,#46733,#46734,#46735,#46736,
#46737,#46738,#46739,#46740,#46741,#46742,#46743,#46744,#46745,#46746,#46747,
#46748,#46749,#46750,#46751,#46752),(#46753,#46754,#46755,#46756,#46757,
#46758,#46759,#46760,#46761,#46762,#46763,#46764,#46765,#46766,#46767,#46768,
#46769,#46770,#46771,#46772,#46773,#46774,#46775,#46776,#46777,#46778,#46779,
#46780,#46781,#46782,#46783,#46784,#46785,#46786,#46787,#46788,#46789,#46790,
#46791,#46792,#46793,#46794,#46795,#46796,#46797,#46798,#46799,#46800,#46801,
#46802,#46803,#46804,#46805,#46806,#46807,#46808,#46809,#46810,#46811,#46812,
#46813,#46814,#46815,#46816,#46817,#46818,#46819,#46820,#46821,#46822,#46823,
#46824,#46825,#46826,#46827,#46828,#46829,#46830,#46831,#46832,#46833,#46834,
#46835,#46836,#46837,#46838,#46839,#46840,#46841,#46842,#46843,#46844,#46845,
#46846,#46847,#46848,#46849,#46850,#46851,#46852,#46853,#46854,#46855,#46856,
#46857,#46858,#46859,#46860,#46861,#46862,#46863,#46864,#46865,#46866,#46867,
#46868,#46869,#46870,#46871,#46872,#46873,#46874,#46875,#46876,#46877,#46878,
#46879,#46880,#46881,#46882,#46883,#46884,#46885,#46886,#46887,#46888,#46889,
#46890,#46891,#46892,#46893,#46894,#46895,#46896,#46897,#46898,#46899,#46900,
#46901,#46902,#46903,#46904,#46905),(#46906,#46907,#46908,#46909,#46910,
#46911,#46912,#46913,#46914,#46915,#46916,#46917,#46918,#46919,#46920,#46921,
#46922,#46923,#46924,#46925,#46926,#46927,#46928,#46929,#46930,#46931,#46932,
#46933,#46934,#46935,#46936,#46937,#46938,#46939,#46940,#46941,#46942,#46943,
#46944,#46945,#46946,#46947,#46948,#46949,#46950,#46951,#46952,#46953,#46954,
#46955,#46956,#46957,#46958,#46959,#46960,#46961,#46962,#46963,#46964,#46965,
#46966,#46967,#46968,#46969,#46970,#46971,#46972,#46973,#46974,#46975,#46976,
#46977,#46978,#46979,#46980,#46981,#46982,#46983,#46984,#46985,#46986,#46987,
#46988,#46989,#46990,#46991,#46992,#46993,#46994,#46995,#46996,#46997,#46998,
#46999,#47000,#47001,#47002,#47003,#47004,#47005,#47006,#47007,#47008,#47009,
#47010,#47011,#47012,#47013,#47014,#47015,#47016,#47017,#47018,#47019,#47020,
#47021,#47022,#47023,#47024,#47025,#47026,#47027,#47028,#47029,#47030,#47031,
#47032,#47033,#47034,#47035,#47036,#47037,#47038,#47039,#47040,#47041,#47042,
#47043,#47044,#47045,#47046,#47047,#47048,#47049,#47050,#47051,#47052,#47053,
#47054,#47055,#47056,#47057,#47058)),.UNSPECIFIED.,.F.,.F.,.F.,(4,4),(4,
1,1,1,1,1,1,1,1,1,1,1,1,1,1,1,1,1,1,1,1,1,1,1,1,1,1,1,1,1,1,1,1,1,1,1,1,
1,1,1,1,1,1,1,1,1,1,1,1,1,1,1,1,1,1,1,1,1,1,1,1,1,1,1,1,1,1,1,1,1,1,1,1,
1,1,1,1,1,1,1,1,1,1,1,1,1,1,1,1,1,1,1,1,1,1,1,1,1,1,1,1,1,1,1,1,1,1,1,1,
1,1,1,1,1,1,1,1,1,1,1,1,1,1,1,1,1,1,1,1,1,1,1,1,1,1,1,1,1,1,1,1,1,1,1,1,
1,1,1,1,1,4),(0.,0.0262983047615875),(13.02168033215,14.0156270002435,15.009573668337,
16.0035203364305,16.997467004524,17.9914136726175,18.9853603407109,19.9793070088044,
20.9732536768979,21.9672003449914,22.9611470130849,23.9550936811784,24.9490403492719,
25.9429870173654,26.9369336854589,27.9308803535524,28.9248270216459,29.9187736897394,
30.9127203578329,31.9066670259264,32.9006136940199,33.8945603621134,34.8885070302068,
35.8824536983003,36.8764003663938,37.8703470344873,38.8642937025808,39.8582403706743,
40.8521870387678,41.8461337068613,42.8400803749548,43.8340270430483,44.8279737111418,
45.8219203792353,46.8158670473288,47.8098137154223,48.8037603835158,49.7977070516092,
50.7916537197027,51.7856003877962,52.7795470558897,53.7734937239832,54.7674403920767,
55.7613870601702,56.7553337282637,57.7492803963572,58.7432270644507,59.7371737325442,
60.7311204006377,61.7250670687312,62.7190137368247,63.7129604049182,64.7069070730116,
65.7008537411051,66.6948004091986,67.6887470772921,68.6826937453856,69.6766404134791,
70.6705870815726,71.6645337496661,72.6584804177596,73.6524270858531,74.6463737539466,
75.6403204220401,76.6342670901336,77.6282137582271,78.6221604263205,79.616107094414,
80.6100537625075,81.604000430601,82.5979470986945,83.591893766788,84.5858404348815,
85.579787102975,86.5737337710685,87.567680439162,88.5616271072555,89.555573775349,
90.5495204434425,91.543467111536,92.5374137796295,93.5313604477229,94.5253071158164,
95.5192537839099,96.5132004520034,97.5071471200969,98.5010937881904,99.4950404562839,
100.488987124377,101.482933792471,102.476880460564,103.470827128658,104.464773796751,
105.458720464845,106.452667132938,107.446613801032,108.440560469125,109.434507137219,
110.428453805312,111.422400473406,112.416347141499,113.410293809593,114.404240477686,
115.39818714578,116.392133813873,117.386080481967,118.38002715006,119.373973818154,
120.367920486247,121.361867154341,122.355813822434,123.349760490528,124.343707158621,
125.337653826715,126.331600494808,127.325547162902,128.319493830995,129.313440499089,
130.307387167182,131.301333835276,132.295280503369,133.289227171463,134.283173839556,
135.27712050765,136.271067175743,137.265013843837,138.25896051193,139.252907180024,
140.246853848117,141.240800516211,142.234747184304,143.228693852398,144.222640520491,
145.216587188585,146.210533856678,147.204480524772,148.198427192865,149.192373860959,
150.186320529052,151.180267197146,152.174213865239,153.168160533333,154.162107201426,
155.15605386952,156.150000537613,157.143947205707,158.1378938738,159.131840541894,
160.125787209987,161.119733878081,162.113680546174),.UNSPECIFIED.);
#477=B_SPLINE_SURFACE_WITH_KNOTS('',3,3,((#47181,#47182,#47183,#47184,#47185,
#47186,#47187,#47188,#47189,#47190,#47191,#47192,#47193,#47194,#47195,#47196,
#47197,#47198,#47199,#47200,#47201,#47202,#47203,#47204,#47205,#47206,#47207,
#47208,#47209,#47210,#47211,#47212,#47213,#47214,#47215,#47216,#47217,#47218,
#47219,#47220,#47221,#47222,#47223,#47224,#47225,#47226,#47227,#47228,#47229,
#47230,#47231,#47232,#47233,#47234,#47235,#47236,#47237,#47238,#47239,#47240,
#47241,#47242,#47243,#47244,#47245,#47246,#47247,#47248,#47249,#47250,#47251,
#47252,#47253,#47254,#47255,#47256,#47257,#47258,#47259,#47260,#47261,#47262,
#47263,#47264,#47265,#47266,#47267,#47268,#47269,#47270,#47271,#47272,#47273,
#47274,#47275,#47276,#47277,#47278,#47279,#47280,#47281,#47282,#47283,#47284,
#47285,#47286,#47287,#47288,#47289,#47290,#47291,#47292,#47293,#47294,#47295,
#47296,#47297,#47298,#47299,#47300,#47301,#47302,#47303,#47304,#47305,#47306,
#47307,#47308,#47309,#47310,#47311,#47312,#47313,#47314,#47315,#47316,#47317,
#47318,#47319,#47320,#47321,#47322,#47323,#47324,#47325,#47326,#47327,#47328,
#47329,#47330,#47331,#47332,#47333),(#47334,#47335,#47336,#47337,#47338,
#47339,#47340,#47341,#47342,#47343,#47344,#47345,#47346,#47347,#47348,#47349,
#47350,#47351,#47352,#47353,#47354,#47355,#47356,#47357,#47358,#47359,#47360,
#47361,#47362,#47363,#47364,#47365,#47366,#47367,#47368,#47369,#47370,#47371,
#47372,#47373,#47374,#47375,#47376,#47377,#47378,#47379,#47380,#47381,#47382,
#47383,#47384,#47385,#47386,#47387,#47388,#47389,#47390,#47391,#47392,#47393,
#47394,#47395,#47396,#47397,#47398,#47399,#47400,#47401,#47402,#47403,#47404,
#47405,#47406,#47407,#47408,#47409,#47410,#47411,#47412,#47413,#47414,#47415,
#47416,#47417,#47418,#47419,#47420,#47421,#47422,#47423,#47424,#47425,#47426,
#47427,#47428,#47429,#47430,#47431,#47432,#47433,#47434,#47435,#47436,#47437,
#47438,#47439,#47440,#47441,#47442,#47443,#47444,#47445,#47446,#47447,#47448,
#47449,#47450,#47451,#47452,#47453,#47454,#47455,#47456,#47457,#47458,#47459,
#47460,#47461,#47462,#47463,#47464,#47465,#47466,#47467,#47468,#47469,#47470,
#47471,#47472,#47473,#47474,#47475,#47476,#47477,#47478,#47479,#47480,#47481,
#47482,#47483,#47484,#47485,#47486),(#47487,#47488,#47489,#47490,#47491,
#47492,#47493,#47494,#47495,#47496,#47497,#47498,#47499,#47500,#47501,#47502,
#47503,#47504,#47505,#47506,#47507,#47508,#47509,#47510,#47511,#47512,#47513,
#47514,#47515,#47516,#47517,#47518,#47519,#47520,#47521,#47522,#47523,#47524,
#47525,#47526,#47527,#47528,#47529,#47530,#47531,#47532,#47533,#47534,#47535,
#47536,#47537,#47538,#47539,#47540,#47541,#47542,#47543,#47544,#47545,#47546,
#47547,#47548,#47549,#47550,#47551,#47552,#47553,#47554,#47555,#47556,#47557,
#47558,#47559,#47560,#47561,#47562,#47563,#47564,#47565,#47566,#47567,#47568,
#47569,#47570,#47571,#47572,#47573,#47574,#47575,#47576,#47577,#47578,#47579,
#47580,#47581,#47582,#47583,#47584,#47585,#47586,#47587,#47588,#47589,#47590,
#47591,#47592,#47593,#47594,#47595,#47596,#47597,#47598,#47599,#47600,#47601,
#47602,#47603,#47604,#47605,#47606,#47607,#47608,#47609,#47610,#47611,#47612,
#47613,#47614,#47615,#47616,#47617,#47618,#47619,#47620,#47621,#47622,#47623,
#47624,#47625,#47626,#47627,#47628,#47629,#47630,#47631,#47632,#47633,#47634,
#47635,#47636,#47637,#47638,#47639),(#47640,#47641,#47642,#47643,#47644,
#47645,#47646,#47647,#47648,#47649,#47650,#47651,#47652,#47653,#47654,#47655,
#47656,#47657,#47658,#47659,#47660,#47661,#47662,#47663,#47664,#47665,#47666,
#47667,#47668,#47669,#47670,#47671,#47672,#47673,#47674,#47675,#47676,#47677,
#47678,#47679,#47680,#47681,#47682,#47683,#47684,#47685,#47686,#47687,#47688,
#47689,#47690,#47691,#47692,#47693,#47694,#47695,#47696,#47697,#47698,#47699,
#47700,#47701,#47702,#47703,#47704,#47705,#47706,#47707,#47708,#47709,#47710,
#47711,#47712,#47713,#47714,#47715,#47716,#47717,#47718,#47719,#47720,#47721,
#47722,#47723,#47724,#47725,#47726,#47727,#47728,#47729,#47730,#47731,#47732,
#47733,#47734,#47735,#47736,#47737,#47738,#47739,#47740,#47741,#47742,#47743,
#47744,#47745,#47746,#47747,#47748,#47749,#47750,#47751,#47752,#47753,#47754,
#47755,#47756,#47757,#47758,#47759,#47760,#47761,#47762,#47763,#47764,#47765,
#47766,#47767,#47768,#47769,#47770,#47771,#47772,#47773,#47774,#47775,#47776,
#47777,#47778,#47779,#47780,#47781,#47782,#47783,#47784,#47785,#47786,#47787,
#47788,#47789,#47790,#47791,#47792)),.UNSPECIFIED.,.F.,.F.,.F.,(4,4),(4,
1,1,1,1,1,1,1,1,1,1,1,1,1,1,1,1,1,1,1,1,1,1,1,1,1,1,1,1,1,1,1,1,1,1,1,1,
1,1,1,1,1,1,1,1,1,1,1,1,1,1,1,1,1,1,1,1,1,1,1,1,1,1,1,1,1,1,1,1,1,1,1,1,
1,1,1,1,1,1,1,1,1,1,1,1,1,1,1,1,1,1,1,1,1,1,1,1,1,1,1,1,1,1,1,1,1,1,1,1,
1,1,1,1,1,1,1,1,1,1,1,1,1,1,1,1,1,1,1,1,1,1,1,1,1,1,1,1,1,1,1,1,1,1,1,1,
1,1,1,1,1,4),(0.,0.0262983047615874),(16.3287821777262,17.3227288458197,
18.3166755139132,19.3106221820067,20.3045688501002,21.2985155181937,22.2924621862871,
23.2864088543806,24.2803555224741,25.2743021905676,26.2682488586611,27.2621955267546,
28.2561421948481,29.2500888629416,30.2440355310351,31.2379821991286,32.2319288672221,
33.2258755353156,34.2198222034091,35.2137688715026,36.2077155395961,37.2016622076895,
38.195608875783,39.1895555438765,40.18350221197,41.1774488800635,42.171395548157,
43.1653422162505,44.159288884344,45.1532355524375,46.147182220531,47.1411288886245,
48.135075556718,49.1290222248115,50.122968892905,51.1169155609985,52.1108622290919,
53.1048088971854,54.0987555652789,55.0927022333724,56.0866489014659,57.0805955695594,
58.0745422376529,59.0684889057464,60.0624355738399,61.0563822419334,62.0503289100269,
63.0442755781204,64.0382222462139,65.0321689143073,66.0261155824008,67.0200622504943,
68.0140089185878,69.0079555866813,70.0019022547748,70.9958489228683,71.9897955909618,
72.9837422590553,73.9776889271488,74.9716355952423,75.9655822633358,76.9595289314293,
77.9534755995228,78.9474222676163,79.9413689357097,80.9353156038032,81.9292622718967,
82.9232089399902,83.9171556080837,84.9111022761772,85.9050489442707,86.8989956123642,
87.8929422804577,88.8868889485512,89.8808356166447,90.8747822847382,91.8687289528317,
92.8626756209252,93.8566222890186,94.8505689571121,95.8445156252056,96.8384622932991,
97.8324089613926,98.8263556294861,99.8203022975796,100.814248965673,101.808195633767,
102.80214230186,103.796088969954,104.790035638047,105.783982306141,106.777928974234,
107.771875642328,108.765822310421,109.759768978515,110.753715646608,111.747662314702,
112.741608982795,113.735555650889,114.729502318982,115.723448987075,116.717395655169,
117.711342323262,118.705288991356,119.699235659449,120.693182327543,121.687128995636,
122.68107566373,123.675022331823,124.668968999917,125.66291566801,126.656862336104,
127.650809004197,128.644755672291,129.638702340384,130.632649008478,131.626595676571,
132.620542344665,133.614489012758,134.608435680852,135.602382348945,136.596329017039,
137.590275685132,138.584222353226,139.578169021319,140.572115689413,141.566062357506,
142.5600090256,143.553955693693,144.547902361787,145.54184902988,146.535795697974,
147.529742366067,148.523689034161,149.517635702254,150.511582370348,151.505529038441,
152.499475706535,153.493422374628,154.487369042722,155.481315710815,156.475262378909,
157.469209047002,158.463155715096,159.457102383189,160.451049051283,161.444995719376,
162.43894238747,163.432889055563,164.426835723657,165.42078239175),
 .UNSPECIFIED.);
#478=B_SPLINE_SURFACE_WITH_KNOTS('',3,3,((#49663,#49664,#49665,#49666,#49667,
#49668,#49669,#49670,#49671,#49672,#49673,#49674,#49675,#49676,#49677,#49678,
#49679,#49680,#49681,#49682,#49683,#49684,#49685,#49686,#49687,#49688,#49689,
#49690,#49691,#49692,#49693,#49694,#49695,#49696,#49697,#49698,#49699,#49700,
#49701,#49702,#49703,#49704,#49705,#49706,#49707,#49708,#49709,#49710,#49711,
#49712,#49713,#49714,#49715,#49716,#49717,#49718,#49719,#49720,#49721,#49722,
#49723,#49724,#49725,#49726,#49727,#49728,#49729,#49730,#49731,#49732,#49733,
#49734,#49735,#49736,#49737,#49738,#49739,#49740,#49741,#49742),(#49743,
#49744,#49745,#49746,#49747,#49748,#49749,#49750,#49751,#49752,#49753,#49754,
#49755,#49756,#49757,#49758,#49759,#49760,#49761,#49762,#49763,#49764,#49765,
#49766,#49767,#49768,#49769,#49770,#49771,#49772,#49773,#49774,#49775,#49776,
#49777,#49778,#49779,#49780,#49781,#49782,#49783,#49784,#49785,#49786,#49787,
#49788,#49789,#49790,#49791,#49792,#49793,#49794,#49795,#49796,#49797,#49798,
#49799,#49800,#49801,#49802,#49803,#49804,#49805,#49806,#49807,#49808,#49809,
#49810,#49811,#49812,#49813,#49814,#49815,#49816,#49817,#49818,#49819,#49820,
#49821,#49822),(#49823,#49824,#49825,#49826,#49827,#49828,#49829,#49830,
#49831,#49832,#49833,#49834,#49835,#49836,#49837,#49838,#49839,#49840,#49841,
#49842,#49843,#49844,#49845,#49846,#49847,#49848,#49849,#49850,#49851,#49852,
#49853,#49854,#49855,#49856,#49857,#49858,#49859,#49860,#49861,#49862,#49863,
#49864,#49865,#49866,#49867,#49868,#49869,#49870,#49871,#49872,#49873,#49874,
#49875,#49876,#49877,#49878,#49879,#49880,#49881,#49882,#49883,#49884,#49885,
#49886,#49887,#49888,#49889,#49890,#49891,#49892,#49893,#49894,#49895,#49896,
#49897,#49898,#49899,#49900,#49901,#49902),(#49903,#49904,#49905,#49906,
#49907,#49908,#49909,#49910,#49911,#49912,#49913,#49914,#49915,#49916,#49917,
#49918,#49919,#49920,#49921,#49922,#49923,#49924,#49925,#49926,#49927,#49928,
#49929,#49930,#49931,#49932,#49933,#49934,#49935,#49936,#49937,#49938,#49939,
#49940,#49941,#49942,#49943,#49944,#49945,#49946,#49947,#49948,#49949,#49950,
#49951,#49952,#49953,#49954,#49955,#49956,#49957,#49958,#49959,#49960,#49961,
#49962,#49963,#49964,#49965,#49966,#49967,#49968,#49969,#49970,#49971,#49972,
#49973,#49974,#49975,#49976,#49977,#49978,#49979,#49980,#49981,#49982)),
 .UNSPECIFIED.,.F.,.F.,.F.,(4,4),(4,1,1,1,1,1,1,1,1,1,1,1,1,1,1,1,1,1,1,
1,1,1,1,1,1,1,1,1,1,1,1,1,1,1,1,1,1,1,1,1,1,1,1,1,1,1,1,1,1,1,1,1,1,1,1,
1,1,1,1,1,1,1,1,1,1,1,1,1,1,1,1,1,1,1,1,1,1,4),(0.,0.0296469363228873),
(12.4950585576113,13.4830028029673,14.4709470483233,15.4588912936793,16.4468355390354,
17.4347797843914,18.4227240297474,19.4106682751034,20.3986125204594,21.3865567658155,
22.3745010111715,23.3624452565275,24.3503895018835,25.3383337472395,26.3262779925956,
27.3142222379516,28.3021664833076,29.2901107286636,30.2780549740196,31.2659992193757,
32.2539434647317,33.2418877100877,34.2298319554437,35.2177762007997,36.2057204461558,
37.1936646915118,38.1816089368678,39.1695531822238,40.1574974275798,41.1454416729359,
42.1333859182919,43.1213301636479,44.1092744090039,45.0972186543599,46.085162899716,
47.073107145072,48.061051390428,49.048995635784,50.03693988114,51.0248841264961,
52.0128283718521,53.0007726172081,53.9887168625641,54.9766611079201,55.9646053532762,
56.9525495986322,57.9404938439882,58.9284380893442,59.9163823347002,60.9043265800563,
61.8922708254123,62.8802150707683,63.8681593161243,64.8561035614803,65.8440478068363,
66.8319920521924,67.8199362975484,68.8078805429044,69.7958247882604,70.7837690336165,
71.7717132789725,72.7596575243285,73.7476017696845,74.7355460150405,75.7234902603965,
76.7114345057526,77.6993787511086,78.6873229964646,79.6752672418206,80.6632114871766,
81.6511557325327,82.6390999778887,83.6270442232447,84.6149884686007,85.6029327139567,
86.5908769593128,87.5788212046688,88.5667654500248),.UNSPECIFIED.);
#479=B_SPLINE_SURFACE_WITH_KNOTS('',3,3,((#50097,#50098,#50099,#50100,#50101,
#50102,#50103,#50104,#50105,#50106,#50107,#50108,#50109,#50110,#50111,#50112,
#50113,#50114,#50115,#50116,#50117,#50118,#50119,#50120,#50121,#50122,#50123,
#50124,#50125,#50126,#50127,#50128,#50129,#50130,#50131,#50132,#50133,#50134,
#50135,#50136,#50137,#50138,#50139,#50140,#50141,#50142,#50143,#50144,#50145,
#50146,#50147,#50148,#50149,#50150,#50151,#50152,#50153,#50154,#50155,#50156,
#50157,#50158,#50159,#50160,#50161,#50162,#50163,#50164,#50165,#50166,#50167,
#50168,#50169,#50170,#50171,#50172,#50173,#50174,#50175,#50176),(#50177,
#50178,#50179,#50180,#50181,#50182,#50183,#50184,#50185,#50186,#50187,#50188,
#50189,#50190,#50191,#50192,#50193,#50194,#50195,#50196,#50197,#50198,#50199,
#50200,#50201,#50202,#50203,#50204,#50205,#50206,#50207,#50208,#50209,#50210,
#50211,#50212,#50213,#50214,#50215,#50216,#50217,#50218,#50219,#50220,#50221,
#50222,#50223,#50224,#50225,#50226,#50227,#50228,#50229,#50230,#50231,#50232,
#50233,#50234,#50235,#50236,#50237,#50238,#50239,#50240,#50241,#50242,#50243,
#50244,#50245,#50246,#50247,#50248,#50249,#50250,#50251,#50252,#50253,#50254,
#50255,#50256),(#50257,#50258,#50259,#50260,#50261,#50262,#50263,#50264,
#50265,#50266,#50267,#50268,#50269,#50270,#50271,#50272,#50273,#50274,#50275,
#50276,#50277,#50278,#50279,#50280,#50281,#50282,#50283,#50284,#50285,#50286,
#50287,#50288,#50289,#50290,#50291,#50292,#50293,#50294,#50295,#50296,#50297,
#50298,#50299,#50300,#50301,#50302,#50303,#50304,#50305,#50306,#50307,#50308,
#50309,#50310,#50311,#50312,#50313,#50314,#50315,#50316,#50317,#50318,#50319,
#50320,#50321,#50322,#50323,#50324,#50325,#50326,#50327,#50328,#50329,#50330,
#50331,#50332,#50333,#50334,#50335,#50336),(#50337,#50338,#50339,#50340,
#50341,#50342,#50343,#50344,#50345,#50346,#50347,#50348,#50349,#50350,#50351,
#50352,#50353,#50354,#50355,#50356,#50357,#50358,#50359,#50360,#50361,#50362,
#50363,#50364,#50365,#50366,#50367,#50368,#50369,#50370,#50371,#50372,#50373,
#50374,#50375,#50376,#50377,#50378,#50379,#50380,#50381,#50382,#50383,#50384,
#50385,#50386,#50387,#50388,#50389,#50390,#50391,#50392,#50393,#50394,#50395,
#50396,#50397,#50398,#50399,#50400,#50401,#50402,#50403,#50404,#50405,#50406,
#50407,#50408,#50409,#50410,#50411,#50412,#50413,#50414,#50415,#50416)),
 .UNSPECIFIED.,.F.,.F.,.F.,(4,4),(4,1,1,1,1,1,1,1,1,1,1,1,1,1,1,1,1,1,1,
1,1,1,1,1,1,1,1,1,1,1,1,1,1,1,1,1,1,1,1,1,1,1,1,1,1,1,1,1,1,1,1,1,1,1,1,
1,1,1,1,1,1,1,1,1,1,1,1,1,1,1,1,1,1,1,1,1,1,4),(0.,0.0296469363228873),
(15.803923819236,16.791868064592,17.779812309948,18.767756555304,19.7557008006601,
20.7436450460161,21.7315892913721,22.7195335367281,23.7074777820841,24.6954220274402,
25.6833662727962,26.6713105181522,27.6592547635082,28.6471990088642,29.6351432542203,
30.6230874995763,31.6110317449323,32.5989759902883,33.5869202356443,34.5748644810004,
35.5628087263564,36.5507529717124,37.5386972170684,38.5266414624244,39.5145857077805,
40.5025299531365,41.4904741984925,42.4784184438485,43.4663626892045,44.4543069345606,
45.4422511799166,46.4301954252726,47.4181396706286,48.4060839159846,49.3940281613407,
50.3819724066967,51.3699166520527,52.3578608974087,53.3458051427647,54.3337493881208,
55.3216936334768,56.3096378788328,57.2975821241888,58.2855263695448,59.2734706149009,
60.2614148602569,61.2493591056129,62.2373033509689,63.2252475963249,64.213191841681,
65.201136087037,66.189080332393,67.177024577749,68.164968823105,69.1529130684611,
70.1408573138171,71.1288015591731,72.1167458045291,73.1046900498851,74.0926342952412,
75.0805785405972,76.0685227859532,77.0564670313092,78.0444112766652,79.0323555220213,
80.0202997673773,81.0082440127333,81.9961882580893,82.9841325034453,83.9720767488014,
84.9600209941574,85.9479652395134,86.9359094848694,87.9238537302254,88.9117979755815,
89.8997422209375,90.8876864662935,91.8756307116495),.UNSPECIFIED.);
#480=B_SPLINE_SURFACE_WITH_KNOTS('',3,3,((#51812,#51813,#51814,#51815,#51816,
#51817,#51818,#51819,#51820,#51821,#51822,#51823,#51824,#51825,#51826,#51827,
#51828,#51829,#51830,#51831,#51832,#51833,#51834,#51835,#51836,#51837,#51838,
#51839,#51840,#51841,#51842,#51843,#51844,#51845,#51846,#51847,#51848,#51849,
#51850,#51851,#51852,#51853,#51854,#51855,#51856,#51857,#51858,#51859,#51860,
#51861,#51862,#51863),(#51864,#51865,#51866,#51867,#51868,#51869,#51870,
#51871,#51872,#51873,#51874,#51875,#51876,#51877,#51878,#51879,#51880,#51881,
#51882,#51883,#51884,#51885,#51886,#51887,#51888,#51889,#51890,#51891,#51892,
#51893,#51894,#51895,#51896,#51897,#51898,#51899,#51900,#51901,#51902,#51903,
#51904,#51905,#51906,#51907,#51908,#51909,#51910,#51911,#51912,#51913,#51914,
#51915),(#51916,#51917,#51918,#51919,#51920,#51921,#51922,#51923,#51924,
#51925,#51926,#51927,#51928,#51929,#51930,#51931,#51932,#51933,#51934,#51935,
#51936,#51937,#51938,#51939,#51940,#51941,#51942,#51943,#51944,#51945,#51946,
#51947,#51948,#51949,#51950,#51951,#51952,#51953,#51954,#51955,#51956,#51957,
#51958,#51959,#51960,#51961,#51962,#51963,#51964,#51965,#51966,#51967),
(#51968,#51969,#51970,#51971,#51972,#51973,#51974,#51975,#51976,#51977,
#51978,#51979,#51980,#51981,#51982,#51983,#51984,#51985,#51986,#51987,#51988,
#51989,#51990,#51991,#51992,#51993,#51994,#51995,#51996,#51997,#51998,#51999,
#52000,#52001,#52002,#52003,#52004,#52005,#52006,#52007,#52008,#52009,#52010,
#52011,#52012,#52013,#52014,#52015,#52016,#52017,#52018,#52019)),
 .UNSPECIFIED.,.F.,.F.,.F.,(4,4),(4,1,1,1,1,1,1,1,1,1,1,1,1,1,1,1,1,1,1,
1,1,1,1,1,1,1,1,1,1,1,1,1,1,1,1,1,1,1,1,1,1,1,1,1,1,1,1,1,1,4),(0.,0.023094010767585),
(12.4478189520753,13.4456071169044,14.4433952817334,15.4411834465625,16.4389716113915,
17.4367597762206,18.4345479410496,19.4323361058786,20.4301242707077,21.4279124355367,
22.4257006003658,23.4234887651948,24.4212769300238,25.4190650948529,26.4168532596819,
27.414641424511,28.41242958934,29.410217754169,30.4080059189981,31.4057940838271,
32.4035822486562,33.4013704134852,34.3991585783142,35.3969467431433,36.3947349079723,
37.3925230728014,38.3903112376304,39.3880994024594,40.3858875672885,41.3836757321175,
42.3814638969466,43.3792520617756,44.3770402266046,45.3748283914337,46.3726165562627,
47.3704047210918,48.3681928859208,49.3659810507499,50.3637692155789,51.3615573804079,
52.359345545237,53.357133710066,54.3549218748951,55.3527100397241,56.3504982045531,
57.3482863693822,58.3460745342112,59.3438626990403,60.3416508638693,61.3394390286984),
 .UNSPECIFIED.);
#481=B_SPLINE_SURFACE_WITH_KNOTS('',3,3,((#52187,#52188,#52189,#52190,#52191,
#52192,#52193,#52194,#52195,#52196,#52197,#52198,#52199,#52200,#52201,#52202,
#52203,#52204,#52205,#52206,#52207,#52208,#52209,#52210,#52211,#52212,#52213,
#52214,#52215,#52216,#52217,#52218,#52219,#52220,#52221,#52222,#52223,#52224,
#52225,#52226,#52227,#52228,#52229,#52230,#52231,#52232,#52233,#52234,#52235,
#52236,#52237,#52238),(#52239,#52240,#52241,#52242,#52243,#52244,#52245,
#52246,#52247,#52248,#52249,#52250,#52251,#52252,#52253,#52254,#52255,#52256,
#52257,#52258,#52259,#52260,#52261,#52262,#52263,#52264,#52265,#52266,#52267,
#52268,#52269,#52270,#52271,#52272,#52273,#52274,#52275,#52276,#52277,#52278,
#52279,#52280,#52281,#52282,#52283,#52284,#52285,#52286,#52287,#52288,#52289,
#52290),(#52291,#52292,#52293,#52294,#52295,#52296,#52297,#52298,#52299,
#52300,#52301,#52302,#52303,#52304,#52305,#52306,#52307,#52308,#52309,#52310,
#52311,#52312,#52313,#52314,#52315,#52316,#52317,#52318,#52319,#52320,#52321,
#52322,#52323,#52324,#52325,#52326,#52327,#52328,#52329,#52330,#52331,#52332,
#52333,#52334,#52335,#52336,#52337,#52338,#52339,#52340,#52341,#52342),
(#52343,#52344,#52345,#52346,#52347,#52348,#52349,#52350,#52351,#52352,
#52353,#52354,#52355,#52356,#52357,#52358,#52359,#52360,#52361,#52362,#52363,
#52364,#52365,#52366,#52367,#52368,#52369,#52370,#52371,#52372,#52373,#52374,
#52375,#52376,#52377,#52378,#52379,#52380,#52381,#52382,#52383,#52384,#52385,
#52386,#52387,#52388,#52389,#52390,#52391,#52392,#52393,#52394)),
 .UNSPECIFIED.,.F.,.F.,.F.,(4,4),(4,1,1,1,1,1,1,1,1,1,1,1,1,1,1,1,1,1,1,
1,1,1,1,1,1,1,1,1,1,1,1,1,1,1,1,1,1,1,1,1,1,1,1,1,1,1,1,1,1,4),(0.,0.023094010767585),
(15.7552446903951,16.7530328552242,17.7508210200532,18.7486091848822,19.7463973497113,
20.7441855145403,21.7419736793694,22.7397618441984,23.7375500090275,24.7353381738565,
25.7331263386855,26.7309145035146,27.7287026683436,28.7264908331727,29.7242789980017,
30.7220671628307,31.7198553276598,32.7176434924888,33.7154316573179,34.7132198221469,
35.7110079869759,36.708796151805,37.706584316634,38.7043724814631,39.7021606462921,
40.6999488111211,41.6977369759502,42.6955251407792,43.6933133056083,44.6911014704373,
45.6888896352663,46.6866778000954,47.6844659649244,48.6822541297535,49.6800422945825,
50.6778304594116,51.6756186242406,52.6734067890696,53.6711949538987,54.6689831187277,
55.6667712835568,56.6645594483858,57.6623476132148,58.6601357780439,59.6579239428729,
60.655712107702,61.653500272531,62.6512884373601,63.6490766021891,64.6468647670181),
 .UNSPECIFIED.);
#482=B_SPLINE_SURFACE_WITH_KNOTS('',3,3,((#53741,#53742,#53743,#53744,#53745,
#53746,#53747,#53748,#53749,#53750,#53751,#53752,#53753,#53754,#53755,#53756,
#53757,#53758,#53759,#53760,#53761,#53762,#53763,#53764,#53765,#53766,#53767,
#53768,#53769,#53770,#53771,#53772,#53773,#53774,#53775,#53776,#53777,#53778,
#53779,#53780,#53781,#53782,#53783,#53784,#53785,#53786,#53787,#53788,#53789,
#53790,#53791,#53792,#53793,#53794,#53795,#53796,#53797,#53798,#53799,#53800,
#53801,#53802,#53803,#53804,#53805,#53806,#53807,#53808,#53809,#53810,#53811,
#53812,#53813,#53814,#53815,#53816,#53817,#53818,#53819,#53820,#53821,#53822,
#53823,#53824,#53825,#53826,#53827,#53828,#53829,#53830,#53831,#53832,#53833,
#53834,#53835,#53836,#53837,#53838,#53839,#53840,#53841,#53842,#53843,#53844,
#53845,#53846),(#53847,#53848,#53849,#53850,#53851,#53852,#53853,#53854,
#53855,#53856,#53857,#53858,#53859,#53860,#53861,#53862,#53863,#53864,#53865,
#53866,#53867,#53868,#53869,#53870,#53871,#53872,#53873,#53874,#53875,#53876,
#53877,#53878,#53879,#53880,#53881,#53882,#53883,#53884,#53885,#53886,#53887,
#53888,#53889,#53890,#53891,#53892,#53893,#53894,#53895,#53896,#53897,#53898,
#53899,#53900,#53901,#53902,#53903,#53904,#53905,#53906,#53907,#53908,#53909,
#53910,#53911,#53912,#53913,#53914,#53915,#53916,#53917,#53918,#53919,#53920,
#53921,#53922,#53923,#53924,#53925,#53926,#53927,#53928,#53929,#53930,#53931,
#53932,#53933,#53934,#53935,#53936,#53937,#53938,#53939,#53940,#53941,#53942,
#53943,#53944,#53945,#53946,#53947,#53948,#53949,#53950,#53951,#53952),
(#53953,#53954,#53955,#53956,#53957,#53958,#53959,#53960,#53961,#53962,
#53963,#53964,#53965,#53966,#53967,#53968,#53969,#53970,#53971,#53972,#53973,
#53974,#53975,#53976,#53977,#53978,#53979,#53980,#53981,#53982,#53983,#53984,
#53985,#53986,#53987,#53988,#53989,#53990,#53991,#53992,#53993,#53994,#53995,
#53996,#53997,#53998,#53999,#54000,#54001,#54002,#54003,#54004,#54005,#54006,
#54007,#54008,#54009,#54010,#54011,#54012,#54013,#54014,#54015,#54016,#54017,
#54018,#54019,#54020,#54021,#54022,#54023,#54024,#54025,#54026,#54027,#54028,
#54029,#54030,#54031,#54032,#54033,#54034,#54035,#54036,#54037,#54038,#54039,
#54040,#54041,#54042,#54043,#54044,#54045,#54046,#54047,#54048,#54049,#54050,
#54051,#54052,#54053,#54054,#54055,#54056,#54057,#54058),(#54059,#54060,
#54061,#54062,#54063,#54064,#54065,#54066,#54067,#54068,#54069,#54070,#54071,
#54072,#54073,#54074,#54075,#54076,#54077,#54078,#54079,#54080,#54081,#54082,
#54083,#54084,#54085,#54086,#54087,#54088,#54089,#54090,#54091,#54092,#54093,
#54094,#54095,#54096,#54097,#54098,#54099,#54100,#54101,#54102,#54103,#54104,
#54105,#54106,#54107,#54108,#54109,#54110,#54111,#54112,#54113,#54114,#54115,
#54116,#54117,#54118,#54119,#54120,#54121,#54122,#54123,#54124,#54125,#54126,
#54127,#54128,#54129,#54130,#54131,#54132,#54133,#54134,#54135,#54136,#54137,
#54138,#54139,#54140,#54141,#54142,#54143,#54144,#54145,#54146,#54147,#54148,
#54149,#54150,#54151,#54152,#54153,#54154,#54155,#54156,#54157,#54158,#54159,
#54160,#54161,#54162,#54163,#54164)),.UNSPECIFIED.,.F.,.F.,.F.,(4,4),(4,
1,1,1,1,1,1,1,1,1,1,1,1,1,1,1,1,1,1,1,1,1,1,1,1,1,1,1,1,1,1,1,1,1,1,1,1,
1,1,1,1,1,1,1,1,1,1,1,1,1,1,1,1,1,1,1,1,1,1,1,1,1,1,1,1,1,1,1,1,1,1,1,1,
1,1,1,1,1,1,1,1,1,1,1,1,1,1,1,1,1,1,1,1,1,1,1,1,1,1,1,1,1,1,4),(0.,0.0230940107675851),
(12.4478189520753,13.4453674388536,14.4429159256318,15.4404644124101,16.4380128991884,
17.4355613859667,18.433109872745,19.4306583595232,20.4282068463015,21.4257553330798,
22.423303819858,23.4208523066363,24.4184007934146,25.4159492801929,26.4134977669712,
27.4110462537494,28.4085947405277,29.406143227306,30.4036917140842,31.4012402008625,
32.3987886876408,33.3963371744191,34.3938856611974,35.3914341479756,36.3889826347539,
37.3865311215322,38.3840796083105,39.3816280950887,40.379176581867,41.3767250686453,
42.3742735554236,43.3718220422018,44.3693705289801,45.3669190157584,46.3644675025367,
47.3620159893149,48.3595644760932,49.3571129628715,50.3546614496498,51.352209936428,
52.3497584232063,53.3473069099846,54.3448553967629,55.3424038835411,56.3399523703194,
57.3375008570977,58.335049343876,59.3325978306542,60.3301463174325,61.3276948042108,
62.3252432909891,63.3227917777673,64.3203402645456,65.3178887513239,66.3154372381021,
67.3129857248804,68.3105342116587,69.308082698437,70.3056311852153,71.3031796719935,
72.3007281587718,73.2982766455501,74.2958251323284,75.2933736191066,76.2909221058849,
77.2884705926632,78.2860190794415,79.2835675662197,80.281116052998,81.2786645397763,
82.2762130265546,83.2737615133328,84.2713100001111,85.2688584868894,86.2664069736677,
87.2639554604459,88.2615039472242,89.2590524340025,90.2566009207808,91.254149407559,
92.2516978943373,93.2492463811156,94.2467948678939,95.2443433546721,96.2418918414504,
97.2394403282287,98.236988815007,99.2345373017852,100.232085788564,101.229634275342,
102.22718276212,103.224731248898,104.222279735677,105.219828222455,106.217376709233,
107.214925196011,108.21247368279,109.210022169568,110.207570656346,111.205119143125,
112.202667629903,113.200216116681,114.197764603459,115.195313090238),
 .UNSPECIFIED.);
#483=B_SPLINE_SURFACE_WITH_KNOTS('',3,3,((#54329,#54330,#54331,#54332,#54333,
#54334,#54335,#54336,#54337,#54338,#54339,#54340,#54341,#54342,#54343,#54344,
#54345,#54346,#54347,#54348,#54349,#54350,#54351,#54352,#54353,#54354,#54355,
#54356,#54357,#54358,#54359,#54360,#54361,#54362,#54363,#54364,#54365,#54366,
#54367,#54368,#54369,#54370,#54371,#54372,#54373,#54374,#54375,#54376,#54377,
#54378,#54379,#54380,#54381,#54382,#54383,#54384,#54385,#54386,#54387,#54388,
#54389,#54390,#54391,#54392,#54393,#54394,#54395,#54396,#54397,#54398,#54399,
#54400,#54401,#54402,#54403,#54404,#54405,#54406,#54407,#54408,#54409,#54410,
#54411,#54412,#54413,#54414,#54415,#54416,#54417,#54418,#54419,#54420,#54421,
#54422,#54423,#54424,#54425,#54426,#54427,#54428,#54429,#54430,#54431,#54432,
#54433,#54434),(#54435,#54436,#54437,#54438,#54439,#54440,#54441,#54442,
#54443,#54444,#54445,#54446,#54447,#54448,#54449,#54450,#54451,#54452,#54453,
#54454,#54455,#54456,#54457,#54458,#54459,#54460,#54461,#54462,#54463,#54464,
#54465,#54466,#54467,#54468,#54469,#54470,#54471,#54472,#54473,#54474,#54475,
#54476,#54477,#54478,#54479,#54480,#54481,#54482,#54483,#54484,#54485,#54486,
#54487,#54488,#54489,#54490,#54491,#54492,#54493,#54494,#54495,#54496,#54497,
#54498,#54499,#54500,#54501,#54502,#54503,#54504,#54505,#54506,#54507,#54508,
#54509,#54510,#54511,#54512,#54513,#54514,#54515,#54516,#54517,#54518,#54519,
#54520,#54521,#54522,#54523,#54524,#54525,#54526,#54527,#54528,#54529,#54530,
#54531,#54532,#54533,#54534,#54535,#54536,#54537,#54538,#54539,#54540),
(#54541,#54542,#54543,#54544,#54545,#54546,#54547,#54548,#54549,#54550,
#54551,#54552,#54553,#54554,#54555,#54556,#54557,#54558,#54559,#54560,#54561,
#54562,#54563,#54564,#54565,#54566,#54567,#54568,#54569,#54570,#54571,#54572,
#54573,#54574,#54575,#54576,#54577,#54578,#54579,#54580,#54581,#54582,#54583,
#54584,#54585,#54586,#54587,#54588,#54589,#54590,#54591,#54592,#54593,#54594,
#54595,#54596,#54597,#54598,#54599,#54600,#54601,#54602,#54603,#54604,#54605,
#54606,#54607,#54608,#54609,#54610,#54611,#54612,#54613,#54614,#54615,#54616,
#54617,#54618,#54619,#54620,#54621,#54622,#54623,#54624,#54625,#54626,#54627,
#54628,#54629,#54630,#54631,#54632,#54633,#54634,#54635,#54636,#54637,#54638,
#54639,#54640,#54641,#54642,#54643,#54644,#54645,#54646),(#54647,#54648,
#54649,#54650,#54651,#54652,#54653,#54654,#54655,#54656,#54657,#54658,#54659,
#54660,#54661,#54662,#54663,#54664,#54665,#54666,#54667,#54668,#54669,#54670,
#54671,#54672,#54673,#54674,#54675,#54676,#54677,#54678,#54679,#54680,#54681,
#54682,#54683,#54684,#54685,#54686,#54687,#54688,#54689,#54690,#54691,#54692,
#54693,#54694,#54695,#54696,#54697,#54698,#54699,#54700,#54701,#54702,#54703,
#54704,#54705,#54706,#54707,#54708,#54709,#54710,#54711,#54712,#54713,#54714,
#54715,#54716,#54717,#54718,#54719,#54720,#54721,#54722,#54723,#54724,#54725,
#54726,#54727,#54728,#54729,#54730,#54731,#54732,#54733,#54734,#54735,#54736,
#54737,#54738,#54739,#54740,#54741,#54742,#54743,#54744,#54745,#54746,#54747,
#54748,#54749,#54750,#54751,#54752)),.UNSPECIFIED.,.F.,.F.,.F.,(4,4),(4,
1,1,1,1,1,1,1,1,1,1,1,1,1,1,1,1,1,1,1,1,1,1,1,1,1,1,1,1,1,1,1,1,1,1,1,1,
1,1,1,1,1,1,1,1,1,1,1,1,1,1,1,1,1,1,1,1,1,1,1,1,1,1,1,1,1,1,1,1,1,1,1,1,
1,1,1,1,1,1,1,1,1,1,1,1,1,1,1,1,1,1,1,1,1,1,1,1,1,1,1,1,1,1,4),(0.,0.0230940107675851),
(15.755244690395,16.7527931771733,17.7503416639516,18.7478901507299,19.7454386375081,
20.7429871242864,21.7405356110647,22.738084097843,23.7356325846212,24.7331810713995,
25.7307295581778,26.7282780449561,27.7258265317343,28.7233750185126,29.7209235052909,
30.7184719920692,31.7160204788475,32.7135689656257,33.711117452404,34.7086659391823,
35.7062144259606,36.7037629127388,37.7013113995171,38.6988598862954,39.6964083730737,
40.6939568598519,41.6915053466302,42.6890538334085,43.6866023201868,44.684150806965,
45.6816992937433,46.6792477805216,47.6767962672999,48.6743447540781,49.6718932408564,
50.6694417276347,51.666990214413,52.6645387011912,53.6620871879695,54.6596356747478,
55.6571841615261,56.6547326483043,57.6522811350826,58.6498296218609,59.6473781086392,
60.6449265954174,61.6424750821957,62.640023568974,63.6375720557523,64.6351205425305,
65.6326690293088,66.6302175160871,67.6277660028654,68.6253144896436,69.6228629764219,
70.6204114632002,71.6179599499785,72.6155084367567,73.613056923535,74.6106054103133,
75.6081538970916,76.6057023838698,77.6032508706481,78.6007993574264,79.5983478442047,
80.595896330983,81.5934448177612,82.5909933045395,83.5885417913178,84.5860902780961,
85.5836387648743,86.5811872516526,87.5787357384309,88.5762842252092,89.5738327119874,
90.5713811987657,91.568929685544,92.5664781723222,93.5640266591005,94.5615751458788,
95.5591236326571,96.5566721194354,97.5542206062136,98.5517690929919,99.5493175797702,
100.546866066548,101.544414553327,102.541963040105,103.539511526883,104.537060013662,
105.53460850044,106.532156987218,107.529705473996,108.527253960775,109.524802447553,
110.522350934331,111.519899421109,112.517447907888,113.514996394666,114.512544881444,
115.510093368223,116.507641855001,117.505190341779,118.502738828557),
 .UNSPECIFIED.);
#484=B_SPLINE_CURVE_WITH_KNOTS('',3,(#36025,#36026,#36027,#36028,#36029,
#36030,#36031,#36032,#36033,#36034),.UNSPECIFIED.,.F.,.F.,(4,2,2,2,4),(0.529829601296569,
0.55431923537737,0.690027699159176,0.825736162940983,0.850225797021783),
 .UNSPECIFIED.);
#485=B_SPLINE_CURVE_WITH_KNOTS('',3,(#36038,#36039,#36040,#36041,#36042,
#36043,#36044,#36045,#36046,#36047),.UNSPECIFIED.,.F.,.F.,(4,2,2,2,4),(0.529829601296585,
0.554319235377384,0.690027699159196,0.825736162941008,0.850225797021807),
 .UNSPECIFIED.);
#486=B_SPLINE_CURVE_WITH_KNOTS('',3,(#36316,#36317,#36318,#36319),
 .UNSPECIFIED.,.F.,.F.,(4,4),(-0.280466891366677,-0.261609752320044),
 .UNSPECIFIED.);
#487=B_SPLINE_CURVE_WITH_KNOTS('',3,(#36323,#36324,#36325,#36326,#36327,
#36328,#36329,#36330,#36331,#36332,#36333,#36334,#36335,#36336,#36337,#36338,
#36339,#36340,#36341,#36342,#36343,#36344,#36345,#36346,#36347,#36348,#36349,
#36350,#36351,#36352,#36353,#36354,#36355,#36356,#36357,#36358,#36359,#36360,
#36361,#36362,#36363,#36364,#36365),.UNSPECIFIED.,.F.,.F.,(4,3,3,3,3,3,
3,3,3,3,3,3,3,3,4),(-0.630634535346295,-0.607069335853016,-0.607059843804484,
-0.566158823266329,-0.566157090505946,-0.545703566972986,-0.530072037367157,
-0.525248310679643,-0.509616781073714,-0.504793054386299,-0.484339530853349,
-0.484337798092956,-0.443436777554782,-0.443427285506269,-0.41986208601299),
 .UNSPECIFIED.);
#488=B_SPLINE_CURVE_WITH_KNOTS('',3,(#36369,#36370,#36371,#36372),
 .UNSPECIFIED.,.F.,.F.,(4,4),(-0.0885671277154287,-0.0696965455598956),
 .UNSPECIFIED.);
#489=B_SPLINE_CURVE_WITH_KNOTS('',3,(#36379,#36380,#36381,#36382,#36383,
#36384,#36385,#36386,#36387,#36388,#36389,#36390),.UNSPECIFIED.,.F.,.F.,
(4,2,2,2,2,4),(-0.113003243228151,-0.107933555890422,-0.0982851988970644,
-0.0760068744412316,-0.0436115274099374,0.),.UNSPECIFIED.);
#490=B_SPLINE_CURVE_WITH_KNOTS('',3,(#36391,#36392,#36393,#36394,#36395,
#36396,#36397,#36398,#36399,#36400,#36401,#36402,#36403,#36404),
 .UNSPECIFIED.,.F.,.F.,(4,2,2,2,2,2,4),(-0.226033312565039,-0.202158826238804,
-0.175315276513873,-0.140039287867993,-0.124092119684883,-0.115509828763379,
-0.113003243228151),.UNSPECIFIED.);
#491=B_SPLINE_CURVE_WITH_KNOTS('',3,(#36474,#36475,#36476,#36477,#36478,
#36479),.UNSPECIFIED.,.F.,.F.,(4,2,4),(0.,0.0362094892516395,0.0734296059630077),
 .UNSPECIFIED.);
#492=B_SPLINE_CURVE_WITH_KNOTS('',3,(#36481,#36482,#36483,#36484,#36485,
#36486,#36487,#36488,#36489,#36490,#36491,#36492,#36493,#36494,#36495,#36496,
#36497),.UNSPECIFIED.,.F.,.F.,(4,2,2,2,1,2,2,2,4),(0.0282690113416936,0.0484109685685348,
0.093261745053174,0.134172257639861,0.175082770226548,0.215993282813234,
0.256903795399921,0.30175457188456,0.321896529111401),.UNSPECIFIED.);
#493=B_SPLINE_CURVE_WITH_KNOTS('',3,(#36498,#36499,#36500,#36501,#36502,
#36503),.UNSPECIFIED.,.F.,.F.,(4,2,4),(0.,0.0226390736381346,0.0740951944294503),
 .UNSPECIFIED.);
#494=B_SPLINE_CURVE_WITH_KNOTS('',3,(#36645,#36646,#36647,#36648,#36649,
#36650,#36651,#36652,#36653,#36654,#36655,#36656,#36657,#36658,#36659,#36660,
#36661,#36662,#36663,#36664,#36665,#36666),.UNSPECIFIED.,.F.,.F.,(4,3,3,
3,3,3,3,4),(0.,0.0219501236857843,0.0311547049411958,0.0514821946010744,
0.0630509139948673,0.0721978608080179,0.0771276015421864,0.0795991465120393),
 .UNSPECIFIED.);
#495=B_SPLINE_CURVE_WITH_KNOTS('',3,(#36668,#36669,#36670,#36671,#36672,
#36673,#36674,#36675,#36676,#36677,#36678,#36679,#36680,#36681,#36682,#36683,
#36684,#36685,#36686,#36687,#36688,#36689,#36690,#36691,#36692),
 .UNSPECIFIED.,.F.,.F.,(4,3,3,3,3,3,3,3,4),(0.0795991465120393,0.0812132933260193,
0.0858207670056381,0.0934958456969542,0.108889996793442,0.128005586672169,
0.13522501814088,0.156399787118725,0.15916082106724),.UNSPECIFIED.);
#496=B_SPLINE_CURVE_WITH_KNOTS('',3,(#36694,#36695,#36696,#36697,#36698,
#36699,#36700,#36701),.UNSPECIFIED.,.F.,.F.,(4,2,2,4),(-0.0966517478861538,
-0.0795140309908814,-0.0397570154954407,0.),.UNSPECIFIED.);
#497=B_SPLINE_CURVE_WITH_KNOTS('',3,(#36705,#36706,#36707,#36708,#36709,
#36710,#36711,#36712,#36713,#36714,#36715,#36716,#36717,#36718,#36719,#36720,
#36721,#36722),.UNSPECIFIED.,.F.,.F.,(4,2,2,2,2,2,2,2,4),(0.,0.0397570154954407,
0.0795140309908814,0.119264247282177,0.159014463573472,0.198764679864768,
0.238514896156063,0.278271911651504,0.318028927146944),.UNSPECIFIED.);
#498=B_SPLINE_CURVE_WITH_KNOTS('',3,(#36723,#36724,#36725,#36726,#36727,
#36728,#36729,#36730,#36731,#36732,#36733,#36734,#36735,#36736,#36737,#36738,
#36739,#36740),.UNSPECIFIED.,.F.,.F.,(4,2,2,2,2,2,2,2,4),(0.318028927146944,
0.357785942642385,0.397542958137826,0.437293174429121,0.477043390720416,
0.516793607011712,0.556543823303007,0.596300838798448,0.636057854293889),
 .UNSPECIFIED.);
#499=B_SPLINE_CURVE_WITH_KNOTS('',3,(#36742,#36743,#36744,#36745,#36746,
#36747,#36748,#36749,#36750,#36751),.UNSPECIFIED.,.F.,.F.,(4,2,2,2,4),(-0.636057854293889,
-0.596300838798448,-0.556543823303007,-0.516793607011712,-0.50481556113779),
 .UNSPECIFIED.);
#500=B_SPLINE_CURVE_WITH_KNOTS('',3,(#36753,#36754,#36755,#36756,#36757,
#36758,#36759,#36760,#36761,#36762,#36763,#36764,#36765,#36766,#36767,#36768,
#36769,#36770,#36771,#36772,#36773,#36774,#36775,#36776,#36777,#36778,#36779,
#36780,#36781,#36782,#36783,#36784,#36785,#36786),.UNSPECIFIED.,.F.,.F.,
(4,3,3,3,3,3,3,3,3,3,3,4),(0.,0.0113828656482154,0.0288034752669669,0.0331384756330993,
0.0355386446508756,0.0366033865449319,0.0375600712478615,0.0399178311655261,
0.0440602794471665,0.0525575068012412,0.0713574218751575,0.0732127853373217),
 .UNSPECIFIED.);
#501=B_SPLINE_CURVE_WITH_KNOTS('',3,(#36787,#36788,#36789,#36790,#36791,
#36792,#36793,#36794,#36795,#36796,#36797,#36798,#36799,#36800,#36801,#36802),
 .UNSPECIFIED.,.F.,.F.,(4,2,2,2,2,2,2,4),(-0.449271220303512,-0.437293174429121,
-0.397542958137826,-0.357785942642385,-0.318028927146944,-0.278271911651504,
-0.238514896156063,-0.221377182278887),.UNSPECIFIED.);
#502=B_SPLINE_CURVE_WITH_KNOTS('',3,(#36811,#36812,#36813,#36814,#36815,
#36816,#36817,#36818,#36819,#36820,#36821,#36822,#36823,#36824,#36825,#36826,
#36827),.UNSPECIFIED.,.F.,.F.,(4,2,2,2,1,2,2,2,4),(0.378434551794792,0.39857650902163,
0.443427285506269,0.484337798092956,0.525248310679643,0.566158823266329,
0.607069335853016,0.651920112337657,0.672062069564494),.UNSPECIFIED.);
#503=B_SPLINE_CURVE_WITH_KNOTS('',3,(#36901,#36902,#36903,#36904,#36905,
#36906),.UNSPECIFIED.,.F.,.F.,(4,2,4),(0.,0.0362094557981297,0.0734296064948461),
 .UNSPECIFIED.);
#504=B_SPLINE_CURVE_WITH_KNOTS('',3,(#36907,#36908,#36909,#36910,#36911,
#36912),.UNSPECIFIED.,.F.,.F.,(4,2,4),(0.,0.0226438889259442,0.0740951100387875),
 .UNSPECIFIED.);
#505=B_SPLINE_CURVE_WITH_KNOTS('',3,(#37754,#37755,#37756,#37757,#37758,
#37759,#37760,#37761,#37762,#37763,#37764,#37765,#37766,#37767,#37768,#37769,
#37770,#37771,#37772,#37773,#37774,#37775),.UNSPECIFIED.,.F.,.F.,(4,3,3,
3,3,3,3,4),(-8.63182595351423,-7.8853565932139,-6.89968701906216,-5.91401744491043,
-4.92834787075869,-3.94267829660695,-2.95700872245521,-2.34864064633464),
 .UNSPECIFIED.);
#506=B_SPLINE_CURVE_WITH_KNOTS('',3,(#37780,#37781,#37782,#37783),
 .UNSPECIFIED.,.F.,.F.,(4,4),(-2.34864064633464,-2.06546402602172),
 .UNSPECIFIED.);
#507=B_SPLINE_CURVE_WITH_KNOTS('',3,(#37786,#37787,#37788,#37789,#37790,
#37791,#37792,#37793,#37794,#37795,#37796,#37797,#37798,#37799,#37800,#37801,
#37802,#37803,#37804),.UNSPECIFIED.,.F.,.F.,(4,3,3,3,3,3,4),(0.,0.985669574151735,
1.97133914830348,2.95700872245521,3.94267829660695,4.92834787075869,5.65574249191081),
 .UNSPECIFIED.);
#508=B_SPLINE_CURVE_WITH_KNOTS('',3,(#37809,#37810,#37811,#37812,#37813,
#37814,#37815,#37816,#37817,#37818,#37819,#37820,#37821,#37822,#37823,#37824,
#37825,#37826,#37827,#37828,#37829,#37830,#37831,#37832,#37833),
 .UNSPECIFIED.,.F.,.F.,(4,3,3,3,3,3,3,3,4),(-14.9150112606938,-14.7850436122761,
-13.7993740381243,-12.8137044639726,-11.8280348898208,-10.8423653156691,
-9.85669574151737,-8.87102616736564,-8.63182595351423),.UNSPECIFIED.);
#509=B_SPLINE_CURVE_WITH_KNOTS('',3,(#37834,#37835,#37836,#37837,#37838,
#37839,#37840,#37841,#37842,#37843,#37844,#37845,#37846,#37847,#37848,#37849,
#37850,#37851,#37852,#37853,#37854,#37855,#37856,#37857,#37858),
 .UNSPECIFIED.,.F.,.F.,(4,3,3,3,3,3,3,3,4),(5.65574249191081,5.91401744491043,
6.89968701906216,7.8853565932139,8.87102616736564,9.85669574151738,10.8423653156691,
11.8280348898208,11.9389277990904),.UNSPECIFIED.);
#510=B_SPLINE_CURVE_WITH_KNOTS('',3,(#37863,#37864,#37865,#37866,#37867,
#37868,#37869,#37870,#37871,#37872,#37873,#37874,#37875,#37876,#37877,#37878,
#37879,#37880,#37881,#37882,#37883,#37884),.UNSPECIFIED.,.F.,.F.,(4,3,3,
3,3,3,3,4),(-21.1981965678734,-20.6990610571865,-19.7133914830348,-18.727721908883,
-17.7420523347313,-16.7563827605795,-15.7707131864278,-14.9150112606938),
 .UNSPECIFIED.);
#511=B_SPLINE_CURVE_WITH_KNOTS('',3,(#37885,#37886,#37887,#37888,#37889,
#37890,#37891,#37892,#37893,#37894,#37895,#37896,#37897,#37898,#37899,#37900,
#37901,#37902,#37903,#37904,#37905,#37906),.UNSPECIFIED.,.F.,.F.,(4,3,3,
3,3,3,3,4),(11.9389277990904,12.8137044639726,13.7993740381243,14.7850436122761,
15.7707131864278,16.7563827605795,17.7420523347313,18.22211310627),
 .UNSPECIFIED.);
#512=B_SPLINE_CURVE_WITH_KNOTS('',3,(#37912,#37913,#37914,#37915,#37916,
#37917),.UNSPECIFIED.,.F.,.F.,(4,1,1,4),(34.5575191894877,35.0440532529525,
36.0297228271043,36.9212675235378),.UNSPECIFIED.);
#513=B_SPLINE_CURVE_WITH_KNOTS('',3,(#37920,#37921,#37922,#37923,#37924),
 .UNSPECIFIED.,.F.,.F.,(4,1,4),(34.5575191894877,34.6939601298316,35.6796297039833),
 .UNSPECIFIED.);
#514=B_SPLINE_CURVE_WITH_KNOTS('',3,(#37929,#37930,#37931,#37932,#37933,
#37934,#37935,#37936,#37937,#37938),.UNSPECIFIED.,.F.,.F.,(4,1,1,1,1,1,
1,4),(28.2743338823081,29.1300358080421,30.1157053821939,31.1013749563456,
32.0870445304973,33.0727141046491,34.0583836788008,34.5575191894877),
 .UNSPECIFIED.);
#515=B_SPLINE_CURVE_WITH_KNOTS('',3,(#37939,#37940,#37941,#37942,#37943,
#37944,#37945,#37946,#37947,#37948),.UNSPECIFIED.,.F.,.F.,(4,1,1,1,1,1,
1,4),(28.2743338823081,28.7799426849212,29.7656122590729,30.7512818332246,
31.7369514073764,32.7226209815281,33.7082905556798,34.5575191894877),
 .UNSPECIFIED.);
#516=B_SPLINE_CURVE_WITH_KNOTS('',3,(#37953,#37954,#37955,#37956,#37957,
#37958,#37959,#37960,#37961,#37962,#37963),.UNSPECIFIED.,.F.,.F.,(4,1,1,
1,1,1,1,1,4),(21.9911485751285,22.23034878898,23.2160183631317,24.2016879372834,
25.1873575114352,26.1730270855869,27.1586966597386,28.1443662338904,28.2743338823081),
 .UNSPECIFIED.);
#517=B_SPLINE_CURVE_WITH_KNOTS('',3,(#37964,#37965,#37966,#37967,#37968,
#37969,#37970,#37971,#37972,#37973),.UNSPECIFIED.,.F.,.F.,(4,1,1,1,1,1,
1,4),(21.9911485751285,22.8659252400107,23.8515948141625,24.8372643883142,
25.8229339624659,26.8086035366177,27.7942731107694,28.2743338823081),
 .UNSPECIFIED.);
#518=B_SPLINE_CURVE_WITH_KNOTS('',3,(#37978,#37979,#37980,#37981,#37982,
#37983,#37984,#37985,#37986,#37987),.UNSPECIFIED.,.F.,.F.,(4,1,1,1,1,1,
1,4),(15.707963267949,16.3163313440695,17.3020009182213,18.287670492373,
19.2733400665247,20.2590096406765,21.2446792148282,21.9911485751285),
 .UNSPECIFIED.);
#519=B_SPLINE_CURVE_WITH_KNOTS('',3,(#37988,#37989,#37990,#37991,#37992,
#37993,#37994,#37995,#37996,#37997,#37998),.UNSPECIFIED.,.F.,.F.,(4,1,1,
1,1,1,1,1,4),(15.707963267949,15.9662382209486,16.9519077951003,17.937577369252,
18.9232469434038,19.9089165175555,20.8945860917073,21.880255665859,21.9911485751285),
 .UNSPECIFIED.);
#520=B_SPLINE_CURVE_WITH_KNOTS('',3,(#38001,#38002,#38003,#38004,#38005,
#38006,#38007,#38008,#38009,#38010,#38011,#38012,#38013,#38014,#38015,#38016,
#38017,#38018,#38019,#38020,#38021,#38022,#38023,#38024,#38025,#38026,#38027,
#38028,#38029,#38030,#38031,#38032,#38033,#38034,#38035,#38036,#38037,#38038,
#38039,#38040,#38041,#38042,#38043,#38044,#38045,#38046),.UNSPECIFIED.,
 .F.,.F.,(4,3,3,3,3,3,3,3,3,3,3,3,3,3,3,4),(-0.178587760439503,-0.171463223481926,
-0.158469202239697,-0.149838461616654,-0.140115954947833,-0.131832290711792,
-0.111519735101834,-0.104220668242419,-0.0909951576576451,-0.0752259129616406,
-0.0672217662272291,-0.0504163246704218,-0.0371902256154733,-0.0290084673554581,
-0.00644509207244406,0.),.UNSPECIFIED.);
#521=B_SPLINE_CURVE_WITH_KNOTS('',3,(#38051,#38052,#38053,#38054,#38055,
#38056,#38057,#38058,#38059,#38060,#38061,#38062,#38063,#38064,#38065,#38066,
#38067,#38068,#38069,#38070,#38071,#38072,#38073,#38074,#38075,#38076,#38077,
#38078,#38079,#38080,#38081,#38082,#38083,#38084,#38085,#38086,#38087,#38088,
#38089,#38090,#38091,#38092,#38093,#38094,#38095,#38096),.UNSPECIFIED.,
 .F.,.F.,(4,3,3,3,3,3,3,3,3,3,3,3,3,3,3,4),(-0.177567088092161,-0.168491849215037,
-0.152129281927587,-0.143009688907872,-0.128326089911933,-0.120351006519644,
-0.0990535795520566,-0.087638613810708,-0.079080103543658,-0.064425434388532,
-0.0552021544374827,-0.041401615828112,-0.0308502855955504,-0.0238678565643904,
-0.00551137719623127,0.),.UNSPECIFIED.);
#522=B_SPLINE_CURVE_WITH_KNOTS('',3,(#38213,#38214,#38215,#38216,#38217,
#38218,#38219,#38220,#38221,#38222,#38223,#38224,#38225,#38226,#38227,#38228,
#38229,#38230,#38231),.UNSPECIFIED.,.F.,.F.,(4,3,3,3,3,3,4),(18.22211310627,
18.727721908883,19.7133914830347,20.6990610571865,21.6847306313382,22.67040020549,
23.5619449019235),.UNSPECIFIED.);
#523=B_SPLINE_CURVE_WITH_KNOTS('',3,(#38233,#38234,#38235,#38236,#38237,
#38238,#38239,#38240,#38241,#38242,#38243,#38244,#38245,#38246,#38247,#38248,
#38249,#38250,#38251,#38252,#38253,#38254,#38255,#38256,#38257,#38258,#38259,
#38260,#38261,#38262,#38263,#38264,#38265,#38266,#38267,#38268,#38269,#38270,
#38271,#38272,#38273,#38274,#38275,#38276,#38277,#38278),.UNSPECIFIED.,
 .F.,.F.,(4,3,3,3,3,3,3,3,3,3,3,3,3,3,3,4),(-0.178587760439501,-0.171463223481924,
-0.158469220396003,-0.149838461060004,-0.140115983264454,-0.131832291484538,
-0.11151973540878,-0.104220666177739,-0.0909951576576466,-0.0752259249257156,
-0.0672217660243099,-0.0504163245182324,-0.0371902270455756,-0.0290084696776603,
-0.00644510100322751,0.),.UNSPECIFIED.);
#524=B_SPLINE_CURVE_WITH_KNOTS('',3,(#38279,#38280,#38281,#38282,#38283,
#38284,#38285),.UNSPECIFIED.,.F.,.F.,(4,1,1,1,4),(12.1176848020599,13.0092294984934,
13.9948990726451,14.9805686467968,15.707963267949),.UNSPECIFIED.);
#525=B_SPLINE_CURVE_WITH_KNOTS('',3,(#38288,#38289,#38290,#38291,#38292,
#38293,#38294,#38295,#38296,#38297,#38298,#38299,#38300,#38301,#38302,#38303,
#38304,#38305,#38306,#38307,#38308,#38309,#38310,#38311,#38312,#38313,#38314,
#38315,#38316,#38317,#38318,#38319,#38320,#38321,#38322,#38323,#38324,#38325,
#38326,#38327,#38328,#38329,#38330,#38331,#38332,#38333),.UNSPECIFIED.,
 .F.,.F.,(4,3,3,3,3,3,3,3,3,3,3,3,3,3,3,4),(-0.177567088092159,-0.168491849215035,
-0.152129287596336,-0.143009693943577,-0.128326090026494,-0.120351011600958,
-0.0990535966185752,-0.087638608675612,-0.0790801035436585,-0.0644254494454798,
-0.0552021579381271,-0.0414016184535953,-0.0308502860822931,-0.0238678558967309,
-0.00551135674322404,0.),.UNSPECIFIED.);
#526=B_SPLINE_CURVE_WITH_KNOTS('',3,(#38336,#38337,#38338,#38339,#38340,
#38341),.UNSPECIFIED.,.F.,.F.,(4,1,1,4),(13.3593226216143,14.3449921957661,
15.3306617699178,15.707963267949),.UNSPECIFIED.);
#527=B_SPLINE_CURVE_WITH_KNOTS('',3,(#38458,#38459,#38460,#38461,#38462,
#38463,#38464,#38465,#38466,#38467,#38468,#38469,#38470,#38471,#38472,#38473),
 .UNSPECIFIED.,.F.,.F.,(4,3,3,3,3,4),(-25.6274089279452,-24.6417393537934,
-23.6560697796417,-22.67040020549,-21.6847306313382,-21.1981965678734),
 .UNSPECIFIED.);
#528=B_SPLINE_CURVE_WITH_KNOTS('',3,(#38534,#38535,#38536,#38537,#38538,
#38539,#38540,#38541,#38542,#38543,#38544,#38545,#38546,#38547,#38548,#38549,
#38550,#38551,#38552),.UNSPECIFIED.,.F.,.F.,(4,3,3,3,3,3,4),(-7.09479596692956,
-6.91220006522707,-5.92474291305177,-4.93728576087648,-3.94982860870118,
-2.96237145652589,-2.06974660785394),.UNSPECIFIED.);
#529=B_SPLINE_CURVE_WITH_KNOTS('',3,(#38560,#38561,#38562,#38563,#38564,
#38565,#38566,#38567,#38568,#38569,#38570,#38571,#38572,#38573,#38574,#38575),
 .UNSPECIFIED.,.F.,.F.,(4,3,3,3,3,4),(0.,0.987457152175289,1.97491430435059,
2.96237145652588,3.94982860870118,4.12047592137467),.UNSPECIFIED.);
#530=B_SPLINE_CURVE_WITH_KNOTS('',3,(#38580,#38581,#38582,#38583,#38584,
#38585,#38586,#38587,#38588,#38589,#38590,#38591,#38592,#38593,#38594,#38595,
#38596,#38597,#38598,#38599,#38600,#38601),.UNSPECIFIED.,.F.,.F.,(4,3,3,
3,3,3,3,4),(-13.3779812741091,-12.8369429782788,-11.8494858261035,-10.8620286739282,
-9.87457152175295,-8.88711436957765,-7.89965721740236,-7.09479596692956),
 .UNSPECIFIED.);
#531=B_SPLINE_CURVE_WITH_KNOTS('',3,(#38602,#38603,#38604,#38605,#38606,
#38607,#38608,#38609,#38610,#38611,#38612,#38613,#38614,#38615,#38616,#38617,
#38618,#38619,#38620,#38621,#38622,#38623),.UNSPECIFIED.,.F.,.F.,(4,3,3,
3,3,3,3,4),(4.12047592137467,4.93728576087648,5.92474291305177,6.91220006522707,
7.89965721740236,8.88711436957765,9.87457152175295,10.4036612285542),
 .UNSPECIFIED.);
#532=B_SPLINE_CURVE_WITH_KNOTS('',3,(#38628,#38629,#38630,#38631,#38632,
#38633,#38634,#38635,#38636,#38637,#38638,#38639,#38640,#38641,#38642,#38643,
#38644,#38645,#38646,#38647,#38648,#38649),.UNSPECIFIED.,.F.,.F.,(4,3,3,
3,3,3,3,4),(-19.6611665812887,-18.7616858913306,-17.7742287391553,-16.78677158698,
-15.7993144348047,-14.8118572826294,-13.8244001304541,-13.3779812741091),
 .UNSPECIFIED.);
#533=B_SPLINE_CURVE_WITH_KNOTS('',3,(#38650,#38651,#38652,#38653,#38654,
#38655,#38656,#38657,#38658,#38659,#38660,#38661,#38662,#38663,#38664,#38665,
#38666,#38667,#38668,#38669,#38670,#38671),.UNSPECIFIED.,.F.,.F.,(4,3,3,
3,3,3,3,4),(10.4036612285542,10.8620286739282,11.8494858261035,12.8369429782788,
13.8244001304541,14.8118572826294,15.7993144348047,16.6868465357338),
 .UNSPECIFIED.);
#534=B_SPLINE_CURVE_WITH_KNOTS('',3,(#38676,#38677,#38678,#38679,#38680,
#38681,#38682,#38683,#38684,#38685,#38686,#38687,#38688,#38689,#38690,#38691,
#38692,#38693,#38694,#38695,#38696,#38697,#38698,#38699,#38700),
 .UNSPECIFIED.,.F.,.F.,(4,3,3,3,3,3,3,3,4),(-25.9443518884683,-25.6738859565577,
-24.6864288043824,-23.6989716522071,-22.7115145000318,-21.7240573478565,
-20.7366001956812,-19.7491430435059,-19.6611665812887),.UNSPECIFIED.);
#535=B_SPLINE_CURVE_WITH_KNOTS('',3,(#38701,#38702,#38703,#38704,#38705,
#38706,#38707,#38708,#38709,#38710,#38711,#38712,#38713,#38714,#38715,#38716,
#38717,#38718,#38719,#38720,#38721,#38722,#38723,#38724,#38725),
 .UNSPECIFIED.,.F.,.F.,(4,3,3,3,3,3,3,3,4),(16.6868465357338,16.78677158698,
17.7742287391553,18.7616858913306,19.7491430435059,20.7366001956812,21.7240573478565,
22.7115145000318,22.9700318429134),.UNSPECIFIED.);
#536=B_SPLINE_CURVE_WITH_KNOTS('',3,(#38730,#38731,#38732,#38733,#38734,
#38735,#38736,#38737,#38738,#38739,#38740,#38741,#38742,#38743,#38744,#38745,
#38746,#38747,#38748,#38749,#38750,#38751),.UNSPECIFIED.,.F.,.F.,(4,3,3,
3,3,3,3,4),(-32.2275371956479,-31.5986288696094,-30.6111717174341,-29.6237145652589,
-28.6362574130836,-27.6488002609083,-26.661343108733,-25.9443518884683),
 .UNSPECIFIED.);
#537=B_SPLINE_CURVE_WITH_KNOTS('',3,(#38752,#38753,#38754,#38755,#38756,
#38757,#38758,#38759,#38760,#38761,#38762,#38763,#38764,#38765,#38766,#38767,
#38768,#38769,#38770,#38771,#38772,#38773),.UNSPECIFIED.,.F.,.F.,(4,3,3,
3,3,3,3,4),(22.9700318429134,23.6989716522071,24.6864288043824,25.6738859565577,
26.661343108733,27.6488002609083,28.6362574130836,29.253217150093),
 .UNSPECIFIED.);
#538=B_SPLINE_CURVE_WITH_KNOTS('',3,(#38778,#38779,#38780,#38781,#38782,
#38783,#38784,#38785,#38786,#38787,#38788,#38789,#38790,#38791,#38792,#38793,
#38794,#38795,#38796,#38797,#38798,#38799),.UNSPECIFIED.,.F.,.F.,(4,3,3,
3,3,3,3,4),(-38.5107225028275,-37.5233717826612,-36.5359146304859,-35.5484574783106,
-34.5610003261353,-33.57354317396,-32.5860860217847,-32.2275371956479),
 .UNSPECIFIED.);
#539=B_SPLINE_CURVE_WITH_KNOTS('',3,(#38800,#38801,#38802,#38803,#38804,
#38805,#38806,#38807,#38808,#38809,#38810,#38811,#38812,#38813,#38814,#38815,
#38816,#38817,#38818,#38819,#38820,#38821),.UNSPECIFIED.,.F.,.F.,(4,3,3,
3,3,3,3,4),(29.253217150093,29.6237145652588,30.6111717174341,31.5986288696094,
32.5860860217847,33.57354317396,34.5610003261353,35.5364024572726),
 .UNSPECIFIED.);
#540=B_SPLINE_CURVE_WITH_KNOTS('',3,(#38826,#38827,#38828,#38829,#38830,
#38831,#38832,#38833,#38834,#38835,#38836,#38837,#38838,#38839,#38840,#38841,
#38842,#38843,#38844,#38845,#38846,#38847),.UNSPECIFIED.,.F.,.F.,(4,3,3,
3,3,3,3,4),(-44.7939078100071,-44.4355718478883,-43.448114695713,-42.4606575435377,
-41.4732003913624,-40.4857432391871,-39.4982860870118,-38.5107225028275),
 .UNSPECIFIED.);
#541=B_SPLINE_CURVE_WITH_KNOTS('',3,(#38848,#38849,#38850,#38851,#38852,
#38853,#38854,#38855,#38856,#38857,#38858,#38859,#38860,#38861,#38862,#38863,
#38864,#38865,#38866,#38867,#38868,#38869,#38870,#38871,#38872),
 .UNSPECIFIED.,.F.,.F.,(4,3,3,3,3,3,3,3,4),(35.5364024572726,35.5484574783106,
36.5359146304859,37.5233717826612,38.5108289348365,39.4982860870118,40.4857432391871,
41.4732003913624,41.8195877644522),.UNSPECIFIED.);
#542=B_SPLINE_CURVE_WITH_KNOTS('',3,(#38877,#38878,#38879,#38880,#38881,
#38882,#38883,#38884,#38885,#38886,#38887,#38888,#38889,#38890,#38891,#38892,
#38893,#38894,#38895,#38896,#38897,#38898),.UNSPECIFIED.,.F.,.F.,(4,3,3,
3,3,3,3,4),(-51.0770931171867,-50.36031476094,-49.3728576087648,-48.3854004565895,
-47.3979433044142,-46.4104861522389,-45.4230290000636,-44.7939078100071),
 .UNSPECIFIED.);
#543=B_SPLINE_CURVE_WITH_KNOTS('',3,(#38899,#38900,#38901,#38902,#38903,
#38904,#38905,#38906,#38907,#38908,#38909,#38910,#38911,#38912,#38913,#38914,
#38915,#38916,#38917,#38918,#38919,#38920),.UNSPECIFIED.,.F.,.F.,(4,3,3,
3,3,3,3,4),(41.8195877644522,42.4606575435377,43.448114695713,44.4355718478883,
45.4230290000636,46.4104861522389,47.3979433044142,48.1027730716318),
 .UNSPECIFIED.);
#544=B_SPLINE_CURVE_WITH_KNOTS('',3,(#38926,#38927,#38928,#38929,#38930,
#38931,#38932,#38933,#38934),.UNSPECIFIED.,.F.,.F.,(4,1,1,1,1,1,4),(59.6902604182061,
60.3193816082625,61.3068387604378,62.2942959126131,63.2817530647884,64.2692102169637,
65.1618350656357),.UNSPECIFIED.);
#545=B_SPLINE_CURVE_WITH_KNOTS('',3,(#38937,#38938,#38939,#38940,#38941,
#38942,#38943,#38944),.UNSPECIFIED.,.F.,.F.,(4,1,1,1,1,4),(59.6902604182061,
59.9728878031637,60.960344955339,61.9478021075143,62.9352592596896,63.9227164118649),
 .UNSPECIFIED.);
#546=B_SPLINE_CURVE_WITH_KNOTS('',3,(#38949,#38950,#38951,#38952,#38953,
#38954,#38955,#38956,#38957,#38958,#38959),.UNSPECIFIED.,.F.,.F.,(4,1,1,
1,1,1,1,1,4),(53.4070751110265,53.4071815430355,54.3946386952108,55.3820958473861,
56.3695529995614,57.3570101517367,58.3444673039119,59.3319244560872,59.6902604182061),
 .UNSPECIFIED.);
#547=B_SPLINE_CURVE_WITH_KNOTS('',3,(#38960,#38961,#38962,#38963,#38964,
#38965,#38966,#38967,#38968,#38969),.UNSPECIFIED.,.F.,.F.,(4,1,1,1,1,1,
1,4),(53.4070751110265,54.0481448901119,55.0356020422872,56.0230591944625,
57.0105163466378,57.9979734988131,58.9854306509884,59.6902604182061),
 .UNSPECIFIED.);
#548=B_SPLINE_CURVE_WITH_KNOTS('',3,(#38974,#38975,#38976,#38977,#38978,
#38979,#38980,#38981,#38982,#38983),.UNSPECIFIED.,.F.,.F.,(4,1,1,1,1,1,
1,4),(47.1238898038469,47.4824386299837,48.469895782159,49.4573529343343,
50.4448100865096,51.4322672386849,52.4197243908602,53.4070751110265),
 .UNSPECIFIED.);
#549=B_SPLINE_CURVE_WITH_KNOTS('',3,(#38984,#38985,#38986,#38987,#38988,
#38989,#38990,#38991,#38992,#38993,#38994),.UNSPECIFIED.,.F.,.F.,(4,1,1,
1,1,1,1,1,4),(47.1238898038469,47.1359448248849,48.1234019770602,49.1108591292355,
50.0983162814107,51.085773433586,52.0732305857613,53.0606877379366,53.4070751110265),
 .UNSPECIFIED.);
#550=B_SPLINE_CURVE_WITH_KNOTS('',3,(#38999,#39000,#39001,#39002,#39003,
#39004,#39005,#39006,#39007,#39008),.UNSPECIFIED.,.F.,.F.,(4,1,1,1,1,1,
1,4),(40.8407044966673,41.5576957169319,42.5451528691072,43.5326100212825,
44.5200671734578,45.5075243256331,46.4949814778084,47.1238898038469),
 .UNSPECIFIED.);
#551=B_SPLINE_CURVE_WITH_KNOTS('',3,(#39009,#39010,#39011,#39012,#39013,
#39014,#39015,#39016,#39017,#39018),.UNSPECIFIED.,.F.,.F.,(4,1,1,1,1,1,
1,4),(40.8407044966673,41.2112019118331,42.1986590640084,43.1861162161837,
44.173573368359,45.1610305205343,46.1484876727096,47.1238898038469),
 .UNSPECIFIED.);
#552=B_SPLINE_CURVE_WITH_KNOTS('',3,(#39023,#39024,#39025,#39026,#39027,
#39028,#39029,#39030,#39031,#39032,#39033),.UNSPECIFIED.,.F.,.F.,(4,1,1,
1,1,1,1,1,4),(34.5575191894877,34.6454956517049,35.6329528038802,36.6204099560555,
37.6078671082307,38.595324260406,39.5827814125813,40.5702385647566,40.8407044966673),
 .UNSPECIFIED.);
#553=B_SPLINE_CURVE_WITH_KNOTS('',3,(#39034,#39035,#39036,#39037,#39038,
#39039,#39040,#39041,#39042,#39043),.UNSPECIFIED.,.F.,.F.,(4,1,1,1,1,1,
1,4),(34.5575191894877,35.2864589987813,36.2739161509566,37.2613733031319,
38.2488304553072,39.2362876074825,40.2237447596578,40.8407044966673),
 .UNSPECIFIED.);
#554=B_SPLINE_CURVE_WITH_KNOTS('',3,(#39048,#39049,#39050,#39051,#39052,
#39053,#39054,#39055,#39056,#39057),.UNSPECIFIED.,.F.,.F.,(4,1,1,1,1,1,
1,4),(28.2743338823081,28.7207527386531,29.7082098908284,30.6956670430037,
31.683124195179,32.6705813473543,33.6580384995296,34.5575191894877),
 .UNSPECIFIED.);
#555=B_SPLINE_CURVE_WITH_KNOTS('',3,(#39058,#39059,#39060,#39061,#39062,
#39063,#39064,#39065,#39066,#39067,#39068),.UNSPECIFIED.,.F.,.F.,(4,1,1,
1,1,1,1,1,4),(28.2743338823081,28.3742589335543,29.3617160857296,30.3491732379048,
31.3366303900801,32.3240875422554,33.3115446944307,34.299001846606,34.5575191894877),
 .UNSPECIFIED.);
#556=B_SPLINE_CURVE_WITH_KNOTS('',3,(#39073,#39074,#39075,#39076,#39077,
#39078,#39079,#39080,#39081,#39082),.UNSPECIFIED.,.F.,.F.,(4,1,1,1,1,1,
1,4),(21.9911485751285,22.7960098256013,23.7834669777766,24.7709241299519,
25.7583812821272,26.7458384343025,27.7332955864778,28.2743338823081),
 .UNSPECIFIED.);
#557=B_SPLINE_CURVE_WITH_KNOTS('',3,(#39083,#39084,#39085,#39086,#39087,
#39088,#39089,#39090,#39091,#39092),.UNSPECIFIED.,.F.,.F.,(4,1,1,1,1,1,
1,4),(21.9911485751285,22.4495160205025,23.4369731726778,24.4244303248531,
25.4118874770284,26.3993446292037,27.386801781379,28.2743338823081),
 .UNSPECIFIED.);
#558=B_SPLINE_CURVE_WITH_KNOTS('',3,(#39097,#39098,#39099,#39100,#39101,
#39102,#39103,#39104,#39105,#39106,#39107),.UNSPECIFIED.,.F.,.F.,(4,1,1,
1,1,1,1,1,4),(15.7079632679489,15.8838097603743,16.8712669125496,17.8587240647249,
18.8461812169001,19.8336383690754,20.8210955212507,21.808552673426,21.9911485751285),
 .UNSPECIFIED.);
#559=B_SPLINE_CURVE_WITH_KNOTS('',3,(#39108,#39109,#39110,#39111,#39112,
#39113,#39114,#39115,#39116,#39117),.UNSPECIFIED.,.F.,.F.,(4,1,1,1,1,1,
1,4),(15.7079632679489,16.5247731074507,17.512230259626,18.4996874118013,
19.4871445639766,20.4746017161519,21.4620588683272,21.9911485751285),
 .UNSPECIFIED.);
#560=B_SPLINE_CURVE_WITH_KNOTS('',3,(#39343,#39344,#39345,#39346,#39347,
#39348,#39349,#39350,#39351,#39352,#39353,#39354,#39355,#39356,#39357,#39358,
#39359,#39360,#39361,#39362,#39363,#39364,#39365,#39366,#39367,#39368,#39369,
#39370,#39371,#39372,#39373,#39374,#39375,#39376,#39377,#39378,#39379,#39380,
#39381,#39382,#39383,#39384,#39385,#39386,#39387,#39388,#39389,#39390,#39391),
 .UNSPECIFIED.,.F.,.F.,(4,3,3,3,3,3,3,3,3,3,3,3,3,3,3,3,4),(-0.226379821609611,
-0.214890180424997,-0.195063355378614,-0.183728168968286,-0.169237877031892,
-0.156768292348793,-0.131336338642949,-0.121264777035684,-0.11376486268334,
-0.101603376860372,-0.0859957740860565,-0.07722199741945,-0.0531920110136073,
-0.041845954216628,-0.0323163699760562,-0.00989131159632156,0.),
 .UNSPECIFIED.);
#561=B_SPLINE_CURVE_WITH_KNOTS('',3,(#39392,#39393,#39394,#39395,#39396,
#39397,#39398,#39399,#39400,#39401),.UNSPECIFIED.,.F.,.F.,(4,3,3,4),(48.1027730716318,
48.3854004565894,49.3728576087647,50.2654824574367),.UNSPECIFIED.);
#562=B_SPLINE_CURVE_WITH_KNOTS('',3,(#39403,#39404,#39405,#39406,#39407,
#39408,#39409,#39410,#39411,#39412,#39413,#39414,#39415,#39416,#39417,#39418,
#39419,#39420,#39421,#39422,#39423,#39424,#39425,#39426,#39427,#39428,#39429,
#39430,#39431,#39432,#39433,#39434,#39435,#39436,#39437,#39438,#39439,#39440,
#39441,#39442,#39443,#39444,#39445,#39446,#39447,#39448,#39449,#39450,#39451),
 .UNSPECIFIED.,.F.,.F.,(4,3,3,3,3,3,3,3,3,3,3,3,3,3,3,3,4),(-0.227523845437318,
-0.218254285946759,-0.205376019353374,-0.194839584423376,-0.181726252813619,
-0.172870003901879,-0.148477559368614,-0.136842916469509,-0.12791553259114,
-0.115084966565271,-0.0973336680873777,-0.0847825202648984,-0.0635868901986738,
-0.0502811887773191,-0.0410407821760877,-0.014115200632659,0.),
 .UNSPECIFIED.);
#563=B_SPLINE_CURVE_WITH_KNOTS('',3,(#39452,#39453,#39454,#39455,#39456,
#39457),.UNSPECIFIED.,.F.,.F.,(4,1,1,4),(13.6572339544282,14.5498588031001,
15.5373159552754,15.7079632679489),.UNSPECIFIED.);
#564=B_SPLINE_CURVE_WITH_KNOTS('',3,(#39460,#39461,#39462,#39463,#39464,
#39465,#39466,#39467,#39468,#39469,#39470,#39471,#39472,#39473,#39474,#39475,
#39476,#39477,#39478,#39479,#39480,#39481,#39482,#39483,#39484,#39485,#39486,
#39487,#39488,#39489,#39490,#39491,#39492,#39493,#39494,#39495,#39496,#39497,
#39498,#39499,#39500,#39501,#39502,#39503,#39504,#39505,#39506,#39507,#39508),
 .UNSPECIFIED.,.F.,.F.,(4,3,3,3,3,3,3,3,3,3,3,3,3,3,3,3,4),(-0.226379821609596,
-0.214890180424979,-0.195063350039947,-0.183728164322639,-0.169237850825561,
-0.156768290223532,-0.131336328824517,-0.12126472687929,-0.113764786721133,
-0.101603376860369,-0.0859957671104269,-0.0772219948002901,-0.0531920146182027,
-0.0418459669675516,-0.0323163753079122,-0.00989133560397837,0.),
 .UNSPECIFIED.);
#565=B_SPLINE_CURVE_WITH_KNOTS('',3,(#39511,#39512,#39513,#39514),
 .UNSPECIFIED.,.F.,.F.,(4,4),(14.896352608199,15.7079632679489),
 .UNSPECIFIED.);
#566=B_SPLINE_CURVE_WITH_KNOTS('',3,(#39740,#39741,#39742,#39743,#39744,
#39745,#39746,#39747,#39748,#39749,#39750,#39751,#39752,#39753,#39754,#39755,
#39756,#39757,#39758,#39759,#39760,#39761,#39762,#39763,#39764,#39765,#39766,
#39767,#39768,#39769,#39770,#39771,#39772,#39773,#39774,#39775,#39776,#39777,
#39778,#39779,#39780,#39781,#39782,#39783,#39784,#39785,#39786,#39787,#39788),
 .UNSPECIFIED.,.F.,.F.,(4,3,3,3,3,3,3,3,3,3,3,3,3,3,3,3,4),(-0.227523845437314,
-0.218254285946756,-0.205376031384273,-0.194839581377744,-0.181726328485879,
-0.172870086995034,-0.148477642599549,-0.13684302479023,-0.127915530672829,
-0.11508496656527,-0.0973336777498854,-0.0847825188673741,-0.0635868891505306,
-0.050281187305254,-0.0410407836210242,-0.0141152073468077,0.),
 .UNSPECIFIED.);
#567=B_SPLINE_CURVE_WITH_KNOTS('',3,(#39789,#39790,#39791,#39792,#39793,
#39794,#39795),.UNSPECIFIED.,.F.,.F.,(4,3,4),(-52.3352290652906,-51.3477719131153,
-51.0770931171867),.UNSPECIFIED.);
#568=B_SPLINE_CURVE_WITH_KNOTS('',3,(#39980,#39981,#39982,#39983,#39984,
#39985,#39986,#39987,#39988,#39989,#39990,#39991,#39992),.UNSPECIFIED.,
 .F.,.F.,(4,3,3,3,4),(-5.66236639740239,-4.98640681629618,-3.98912545303695,
-2.99184408977771,-2.0654640260217),.UNSPECIFIED.);
#569=B_SPLINE_CURVE_WITH_KNOTS('',3,(#40000,#40001,#40002,#40003,#40004,
#40005,#40006,#40007,#40008,#40009),.UNSPECIFIED.,.F.,.F.,(4,3,3,4),(0.,
0.997281363259236,1.99456272651847,2.68628293579911),.UNSPECIFIED.);
#570=B_SPLINE_CURVE_WITH_KNOTS('',3,(#40014,#40015,#40016,#40017,#40018,
#40019,#40020,#40021,#40022,#40023,#40024,#40025,#40026,#40027,#40028,#40029,
#40030,#40031,#40032,#40033,#40034,#40035),.UNSPECIFIED.,.F.,.F.,(4,3,3,
3,3,3,3,4),(-11.945551704582,-10.9700949958516,-9.97281363259237,-8.97553226933314,
-7.9782509060739,-6.98096954281466,-5.98368817955542,-5.66236639740239),
 .UNSPECIFIED.);
#571=B_SPLINE_CURVE_WITH_KNOTS('',3,(#40036,#40037,#40038,#40039,#40040,
#40041,#40042,#40043,#40044,#40045,#40046,#40047,#40048,#40049,#40050,#40051,
#40052,#40053,#40054,#40055,#40056,#40057),.UNSPECIFIED.,.F.,.F.,(4,3,3,
3,3,3,3,4),(2.68628293579911,2.99184408977771,3.98912545303695,4.98640681629619,
5.98368817955542,6.98096954281466,7.9782509060739,8.9694682429787),
 .UNSPECIFIED.);
#572=B_SPLINE_CURVE_WITH_KNOTS('',3,(#40062,#40063,#40064,#40065,#40066,
#40067,#40068,#40069,#40070,#40071,#40072,#40073,#40074,#40075,#40076,#40077,
#40078,#40079,#40080,#40081,#40082,#40083,#40084,#40085,#40086),
 .UNSPECIFIED.,.F.,.F.,(4,3,3,3,3,3,3,3,4),(-18.2287370117616,-17.9510645386663,
-16.953783175407,-15.9565018121478,-14.9592204488886,-13.9619390856293,
-12.9646577223701,-11.9673763591108,-11.945551704582),.UNSPECIFIED.);
#573=B_SPLINE_CURVE_WITH_KNOTS('',3,(#40087,#40088,#40089,#40090,#40091,
#40092,#40093,#40094,#40095,#40096,#40097,#40098,#40099,#40100,#40101,#40102,
#40103,#40104,#40105,#40106,#40107,#40108),.UNSPECIFIED.,.F.,.F.,(4,3,3,
3,3,3,3,4),(8.9694682429787,9.97281363259238,10.9700949958516,11.9673763591108,
12.9646577223701,13.9619390856293,14.9592204488886,15.2526535501583),
 .UNSPECIFIED.);
#574=B_SPLINE_CURVE_WITH_KNOTS('',3,(#40113,#40114,#40115,#40116,#40117,
#40118,#40119,#40120,#40121,#40122,#40123,#40124,#40125,#40126,#40127,#40128,
#40129,#40130,#40131,#40132,#40133,#40134),.UNSPECIFIED.,.F.,.F.,(4,3,3,
3,3,3,3,4),(-24.5119223189412,-23.9347527182217,-22.9374713549625,-21.9401899917032,
-20.942908628444,-19.9456272651847,-18.9483459019255,-18.2287370117616),
 .UNSPECIFIED.);
#575=B_SPLINE_CURVE_WITH_KNOTS('',3,(#40135,#40136,#40137,#40138,#40139,
#40140,#40141,#40142,#40143,#40144,#40145,#40146,#40147,#40148,#40149,#40150,
#40151,#40152,#40153,#40154,#40155,#40156),.UNSPECIFIED.,.F.,.F.,(4,3,3,
3,3,3,3,4),(15.2526535501583,15.9565018121478,16.953783175407,17.9510645386663,
18.9483459019255,19.9456272651847,20.942908628444,21.5358388573379),
 .UNSPECIFIED.);
#576=B_SPLINE_CURVE_WITH_KNOTS('',3,(#40161,#40162,#40163,#40164,#40165,
#40166,#40167,#40168,#40169,#40170,#40171,#40172,#40173,#40174,#40175,#40176,
#40177,#40178,#40179,#40180,#40181,#40182),.UNSPECIFIED.,.F.,.F.,(4,3,3,
3,3,3,3,4),(-30.7951076261207,-29.9184408977771,-28.9211595345179,-27.9238781712586,
-26.9265968079994,-25.9293154447402,-24.9320340814809,-24.5119223189412),
 .UNSPECIFIED.);
#577=B_SPLINE_CURVE_WITH_KNOTS('',3,(#40183,#40184,#40185,#40186,#40187,
#40188,#40189,#40190,#40191,#40192,#40193,#40194,#40195,#40196,#40197,#40198,
#40199,#40200,#40201,#40202,#40203,#40204),.UNSPECIFIED.,.F.,.F.,(4,3,3,
3,3,3,3,4),(21.5358388573379,21.9401899917032,22.9374713549625,23.9347527182217,
24.9320340814809,25.9293154447402,26.9265968079994,27.8190241645175),
 .UNSPECIFIED.);
#578=B_SPLINE_CURVE_WITH_KNOTS('',3,(#40209,#40210,#40211,#40212,#40213,
#40214,#40215,#40216,#40217,#40218,#40219,#40220,#40221,#40222,#40223,#40224,
#40225,#40226,#40227,#40228,#40229,#40230,#40231,#40232,#40233),
 .UNSPECIFIED.,.F.,.F.,(4,3,3,3,3,3,3,3,4),(-37.0782929333003,-36.8994104405918,
-35.9021290773325,-34.9048477140733,-33.9075663508141,-32.9102849875548,
-31.9130036242956,-30.9157222610364,-30.7951076261207),.UNSPECIFIED.);
#579=B_SPLINE_CURVE_WITH_KNOTS('',3,(#40234,#40235,#40236,#40237,#40238,
#40239,#40240,#40241,#40242,#40243,#40244,#40245,#40246,#40247,#40248,#40249,
#40250,#40251,#40252,#40253,#40254,#40255,#40256,#40257,#40258),
 .UNSPECIFIED.,.F.,.F.,(4,3,3,3,3,3,3,3,4),(27.8190241645175,27.9238781712587,
28.9211595345179,29.9184408977771,30.9157222610364,31.9130036242956,32.9102849875548,
33.9075663508141,34.1022094716971),.UNSPECIFIED.);
#580=B_SPLINE_CURVE_WITH_KNOTS('',3,(#40263,#40264,#40265,#40266,#40267,
#40268,#40269,#40270,#40271,#40272,#40273,#40274,#40275,#40276,#40277,#40278,
#40279,#40280,#40281,#40282,#40283,#40284),.UNSPECIFIED.,.F.,.F.,(4,3,3,
3,3,3,3,4),(-43.3614782404799,-42.8830986201472,-41.885817256888,-40.8885358936287,
-39.8912545303695,-38.8939731671102,-37.896691803851,-37.0782929333003),
 .UNSPECIFIED.);
#581=B_SPLINE_CURVE_WITH_KNOTS('',3,(#40285,#40286,#40287,#40288,#40289,
#40290,#40291,#40292,#40293,#40294,#40295,#40296,#40297,#40298,#40299,#40300,
#40301,#40302,#40303,#40304,#40305,#40306),.UNSPECIFIED.,.F.,.F.,(4,3,3,
3,3,3,3,4),(34.1022094716971,34.9048477140733,35.9021290773325,36.8994104405918,
37.896691803851,38.8939731671102,39.8912545303695,40.3853947788766),
 .UNSPECIFIED.);
#582=B_SPLINE_CURVE_WITH_KNOTS('',3,(#40311,#40312,#40313,#40314,#40315,
#40316,#40317,#40318,#40319,#40320,#40321,#40322,#40323,#40324,#40325,#40326,
#40327,#40328,#40329,#40330,#40331,#40332),.UNSPECIFIED.,.F.,.F.,(4,3,3,
3,3,3,3,4),(-49.6446635476595,-48.8667867997026,-47.8695054364434,-46.8722240731841,
-45.8749427099249,-44.8776613466657,-43.8803799834064,-43.3614782404799),
 .UNSPECIFIED.);
#583=B_SPLINE_CURVE_WITH_KNOTS('',3,(#40333,#40334,#40335,#40336,#40337,
#40338,#40339,#40340,#40341,#40342,#40343,#40344,#40345,#40346,#40347,#40348,
#40349,#40350,#40351,#40352,#40353,#40354),.UNSPECIFIED.,.F.,.F.,(4,3,3,
3,3,3,3,4),(40.3853947788766,40.8885358936287,41.885817256888,42.8830986201472,
43.8803799834064,44.8776613466657,45.8749427099249,46.6685800860562),
 .UNSPECIFIED.);
#584=B_SPLINE_CURVE_WITH_KNOTS('',3,(#40359,#40360,#40361,#40362,#40363,
#40364,#40365,#40366,#40367,#40368,#40369,#40370,#40371,#40372,#40373,#40374,
#40375,#40376,#40377,#40378,#40379,#40380,#40381,#40382,#40383),
 .UNSPECIFIED.,.F.,.F.,(4,3,3,3,3,3,3,3,4),(-55.9278488548391,-55.8477563425173,
-54.8504749792581,-53.8531936159988,-52.8559122527396,-51.8586308894803,
-50.8613495262211,-49.8640681629619,-49.6446635476595),.UNSPECIFIED.);
#585=B_SPLINE_CURVE_WITH_KNOTS('',3,(#40384,#40385,#40386,#40387,#40388,
#40389,#40390,#40391,#40392,#40393,#40394,#40395,#40396,#40397,#40398,#40399,
#40400,#40401,#40402,#40403,#40404,#40405,#40406,#40407,#40408),
 .UNSPECIFIED.,.F.,.F.,(4,3,3,3,3,3,3,3,4),(46.6685800860562,46.8722240731842,
47.8695054364434,48.8667867997026,49.8640681629619,50.8613495262211,51.8586308894803,
52.8559122527396,52.9517653932358),.UNSPECIFIED.);
#586=B_SPLINE_CURVE_WITH_KNOTS('',3,(#40413,#40414,#40415,#40416,#40417,
#40418,#40419,#40420,#40421,#40422,#40423,#40424,#40425,#40426,#40427,#40428,
#40429,#40430,#40431,#40432,#40433,#40434),.UNSPECIFIED.,.F.,.F.,(4,3,3,
3,3,3,3,4),(-62.2110341620187,-61.8314445220727,-60.8341631588134,-59.8368817955542,
-58.839600432295,-57.8423190690358,-56.8450377057765,-55.9278488548391),
 .UNSPECIFIED.);
#587=B_SPLINE_CURVE_WITH_KNOTS('',3,(#40435,#40436,#40437,#40438,#40439,
#40440,#40441,#40442,#40443,#40444,#40445,#40446,#40447,#40448,#40449,#40450,
#40451,#40452,#40453,#40454,#40455,#40456),.UNSPECIFIED.,.F.,.F.,(4,3,3,
3,3,3,3,4),(52.9517653932358,53.8531936159988,54.8504749792581,55.8477563425173,
56.8450377057765,57.8423190690358,58.839600432295,59.2349507004154),
 .UNSPECIFIED.);
#588=B_SPLINE_CURVE_WITH_KNOTS('',3,(#40461,#40462,#40463,#40464,#40465,
#40466,#40467,#40468,#40469,#40470,#40471,#40472,#40473,#40474,#40475,#40476,
#40477,#40478,#40479,#40480,#40481,#40482),.UNSPECIFIED.,.F.,.F.,(4,3,3,
3,3,3,3,4),(-68.4942194691983,-67.8151327016281,-66.8178513383689,-65.8205699751096,
-64.8232886118504,-63.8260072485912,-62.8287258853319,-62.2110341620187),
 .UNSPECIFIED.);
#589=B_SPLINE_CURVE_WITH_KNOTS('',3,(#40483,#40484,#40485,#40486,#40487,
#40488,#40489,#40490,#40491,#40492,#40493,#40494,#40495,#40496,#40497,#40498,
#40499,#40500,#40501,#40502,#40503,#40504),.UNSPECIFIED.,.F.,.F.,(4,3,3,
3,3,3,3,4),(59.2349507004154,59.8368817955542,60.8341631588135,61.8314445220727,
62.8287258853319,63.8260072485912,64.8232886118504,65.518136007595),
 .UNSPECIFIED.);
#590=B_SPLINE_CURVE_WITH_KNOTS('',3,(#40509,#40510,#40511,#40512,#40513,
#40514,#40515,#40516,#40517,#40518,#40519,#40520,#40521,#40522,#40523,#40524,
#40525,#40526,#40527,#40528,#40529,#40530),.UNSPECIFIED.,.F.,.F.,(4,3,3,
3,3,3,3,4),(-74.7774047763779,-73.7988208811836,-72.8015395179243,-71.8042581546651,
-70.8069767914058,-69.8096954281466,-68.8124140648874,-68.4942194691983),
 .UNSPECIFIED.);
#591=B_SPLINE_CURVE_WITH_KNOTS('',3,(#40531,#40532,#40533,#40534,#40535,
#40536,#40537,#40538,#40539,#40540,#40541,#40542,#40543,#40544,#40545,#40546,
#40547,#40548,#40549,#40550,#40551,#40552),.UNSPECIFIED.,.F.,.F.,(4,3,3,
3,3,3,3,4),(65.518136007595,65.8205699751097,66.8178513383689,67.8151327016281,
68.8124140648874,69.8096954281466,70.8069767914059,71.8013213147746),
 .UNSPECIFIED.);
#592=B_SPLINE_CURVE_WITH_KNOTS('',3,(#40557,#40558,#40559,#40560,#40561,
#40562,#40563,#40564,#40565,#40566,#40567,#40568,#40569,#40570,#40571,#40572,
#40573,#40574,#40575,#40576,#40577,#40578,#40579,#40580,#40581),
 .UNSPECIFIED.,.F.,.F.,(4,3,3,3,3,3,3,3,4),(-81.0605900835575,-80.7797904239982,
-79.782509060739,-78.7852276974797,-77.7879463342205,-76.7906649709613,
-75.793383607702,-74.7961022444428,-74.7774047763779),.UNSPECIFIED.);
#593=B_SPLINE_CURVE_WITH_KNOTS('',3,(#40582,#40583,#40584,#40585,#40586,
#40587,#40588,#40589,#40590,#40591,#40592,#40593,#40594,#40595,#40596,#40597,
#40598,#40599,#40600,#40601,#40602,#40603),.UNSPECIFIED.,.F.,.F.,(4,3,3,
3,3,3,3,4),(71.8013213147746,72.8015395179243,73.7988208811836,74.7961022444428,
75.793383607702,76.7906649709613,77.7879463342205,78.0845066219542),
 .UNSPECIFIED.);
#594=B_SPLINE_CURVE_WITH_KNOTS('',3,(#40608,#40609,#40610,#40611,#40612,
#40613,#40614,#40615,#40616,#40617,#40618,#40619,#40620,#40621,#40622,#40623,
#40624,#40625,#40626,#40627,#40628,#40629),.UNSPECIFIED.,.F.,.F.,(4,3,3,
3,3,3,3,4),(-87.3437753907371,-86.7634786035536,-85.7661972402944,-84.7689158770352,
-83.7716345137759,-82.7743531505167,-81.7770717872575,-81.0605900835575),
 .UNSPECIFIED.);
#595=B_SPLINE_CURVE_WITH_KNOTS('',3,(#40630,#40631,#40632,#40633,#40634,
#40635,#40636,#40637,#40638,#40639,#40640,#40641,#40642,#40643,#40644,#40645,
#40646,#40647,#40648,#40649,#40650,#40651),.UNSPECIFIED.,.F.,.F.,(4,3,3,
3,3,3,3,4),(78.0845066219542,78.7852276974798,79.782509060739,80.7797904239982,
81.7770717872575,82.7743531505167,83.7716345137759,84.3676919291338),
 .UNSPECIFIED.);
#596=B_SPLINE_CURVE_WITH_KNOTS('',3,(#40656,#40657,#40658,#40659,#40660,
#40661,#40662,#40663,#40664,#40665,#40666,#40667,#40668,#40669,#40670,#40671,
#40672,#40673,#40674,#40675,#40676,#40677),.UNSPECIFIED.,.F.,.F.,(4,3,3,
3,3,3,3,4),(-93.6269606979167,-92.7471667831091,-91.7498854198498,-90.7526040565906,
-89.7553226933313,-88.7580413300721,-87.7607599668129,-87.3437753907371),
 .UNSPECIFIED.);
#597=B_SPLINE_CURVE_WITH_KNOTS('',3,(#40678,#40679,#40680,#40681,#40682,
#40683,#40684,#40685,#40686,#40687,#40688,#40689,#40690,#40691,#40692,#40693,
#40694,#40695,#40696,#40697,#40698,#40699),.UNSPECIFIED.,.F.,.F.,(4,3,3,
3,3,3,3,4),(84.3676919291338,84.7689158770352,85.7661972402944,86.7634786035537,
87.7607599668129,88.7580413300721,89.7553226933314,90.6508772363134),
 .UNSPECIFIED.);
#598=B_SPLINE_CURVE_WITH_KNOTS('',3,(#40704,#40705,#40706,#40707,#40708,
#40709,#40710,#40711,#40712,#40713,#40714,#40715,#40716,#40717,#40718,#40719,
#40720,#40721,#40722,#40723,#40724,#40725,#40726,#40727,#40728),
 .UNSPECIFIED.,.F.,.F.,(4,3,3,3,3,3,3,3,4),(-99.9101460050962,-99.7281363259237,
-98.7308549626645,-97.7335735994052,-96.736292236146,-95.7390108728868,
-94.7417295096275,-93.7444481463683,-93.6269606979167),.UNSPECIFIED.);
#599=B_SPLINE_CURVE_WITH_KNOTS('',3,(#40729,#40730,#40731,#40732,#40733,
#40734,#40735,#40736,#40737,#40738,#40739,#40740,#40741,#40742,#40743,#40744,
#40745,#40746,#40747,#40748,#40749,#40750,#40751,#40752,#40753),
 .UNSPECIFIED.,.F.,.F.,(4,3,3,3,3,3,3,3,4),(90.6508772363134,90.7526040565906,
91.7498854198498,92.7471667831091,93.7444481463683,94.7417295096275,95.7390108728868,
96.736292236146,96.934062543493),.UNSPECIFIED.);
#600=B_SPLINE_CURVE_WITH_KNOTS('',3,(#40758,#40759,#40760,#40761,#40762,
#40763,#40764,#40765,#40766,#40767,#40768,#40769,#40770,#40771,#40772,#40773,
#40774,#40775,#40776,#40777,#40778,#40779),.UNSPECIFIED.,.F.,.F.,(4,3,3,
3,3,3,3,4),(-106.193331312276,-105.711824505479,-104.71454314222,-103.717261778961,
-102.719980415701,-101.722699052442,-100.725417689183,-99.9101460050962),
 .UNSPECIFIED.);
#601=B_SPLINE_CURVE_WITH_KNOTS('',3,(#40780,#40781,#40782,#40783,#40784,
#40785,#40786,#40787,#40788,#40789,#40790,#40791,#40792,#40793,#40794,#40795,
#40796,#40797,#40798,#40799,#40800,#40801),.UNSPECIFIED.,.F.,.F.,(4,3,3,
3,3,3,3,4),(96.934062543493,97.7335735994053,98.7308549626645,99.7281363259237,
100.725417689183,101.722699052442,102.719980415701,103.217247850673),
 .UNSPECIFIED.);
#602=B_SPLINE_CURVE_WITH_KNOTS('',3,(#40806,#40807,#40808,#40809,#40810,
#40811,#40812,#40813,#40814,#40815,#40816,#40817,#40818,#40819,#40820,#40821,
#40822,#40823,#40824,#40825,#40826,#40827),.UNSPECIFIED.,.F.,.F.,(4,3,3,
3,3,3,3,4),(-112.476516619455,-111.695512685035,-110.698231321775,-109.700949958516,
-108.703668595257,-107.706387231998,-106.709105868738,-106.193331312276),
 .UNSPECIFIED.);
#603=B_SPLINE_CURVE_WITH_KNOTS('',3,(#40828,#40829,#40830,#40831,#40832,
#40833,#40834,#40835,#40836,#40837,#40838,#40839,#40840,#40841,#40842,#40843,
#40844,#40845,#40846,#40847,#40848,#40849),.UNSPECIFIED.,.F.,.F.,(4,3,3,
3,3,3,3,4),(103.217247850673,103.717261778961,104.71454314222,105.711824505479,
106.709105868738,107.706387231998,108.703668595257,109.500433157852),
 .UNSPECIFIED.);
#604=B_SPLINE_CURVE_WITH_KNOTS('',3,(#40854,#40855,#40856,#40857,#40858,
#40859,#40860,#40861,#40862,#40863,#40864,#40865,#40866,#40867,#40868,#40869,
#40870,#40871,#40872,#40873,#40874,#40875,#40876,#40877,#40878),
 .UNSPECIFIED.,.F.,.F.,(4,3,3,3,3,3,3,3,4),(-118.759701926635,-118.676482227849,
-117.67920086459,-116.681919501331,-115.684638138071,-114.687356774812,
-113.690075411553,-112.692794048294,-112.476516619455),.UNSPECIFIED.);
#605=B_SPLINE_CURVE_WITH_KNOTS('',3,(#40879,#40880,#40881,#40882,#40883,
#40884,#40885,#40886,#40887,#40888,#40889,#40890,#40891,#40892,#40893,#40894,
#40895,#40896,#40897,#40898,#40899,#40900,#40901,#40902,#40903),
 .UNSPECIFIED.,.F.,.F.,(4,3,3,3,3,3,3,3,4),(109.500433157852,109.700949958516,
110.698231321775,111.695512685035,112.692794048294,113.690075411553,114.687356774812,
115.684638138072,115.783618465032),.UNSPECIFIED.);
#606=B_SPLINE_CURVE_WITH_KNOTS('',3,(#40908,#40909,#40910,#40911,#40912,
#40913,#40914,#40915,#40916,#40917,#40918,#40919,#40920,#40921,#40922,#40923,
#40924,#40925,#40926,#40927,#40928,#40929),.UNSPECIFIED.,.F.,.F.,(4,3,3,
3,3,3,3,4),(-125.042887233815,-124.660170407405,-123.662889044145,-122.665607680886,
-121.668326317627,-120.671044954368,-119.673763591108,-118.759701926635),
 .UNSPECIFIED.);
#607=B_SPLINE_CURVE_WITH_KNOTS('',3,(#40930,#40931,#40932,#40933,#40934,
#40935,#40936,#40937,#40938,#40939,#40940,#40941,#40942,#40943,#40944,#40945,
#40946,#40947,#40948,#40949,#40950,#40951),.UNSPECIFIED.,.F.,.F.,(4,3,3,
3,3,3,3,4),(115.783618465032,116.681919501331,117.67920086459,118.676482227849,
119.673763591108,120.671044954368,121.668326317627,122.066803772211),
 .UNSPECIFIED.);
#608=B_SPLINE_CURVE_WITH_KNOTS('',3,(#40956,#40957,#40958,#40959,#40960,
#40961,#40962,#40963,#40964,#40965,#40966,#40967,#40968,#40969,#40970,#40971,
#40972,#40973,#40974,#40975,#40976,#40977),.UNSPECIFIED.,.F.,.F.,(4,3,3,
3,3,3,3,4),(-131.326072540994,-130.64385858696,-129.646577223701,-128.649295860442,
-127.652014497182,-126.654733133923,-125.657451770664,-125.042887233815),
 .UNSPECIFIED.);
#609=B_SPLINE_CURVE_WITH_KNOTS('',3,(#40978,#40979,#40980,#40981,#40982,
#40983,#40984,#40985,#40986,#40987,#40988,#40989,#40990,#40991,#40992,#40993,
#40994,#40995,#40996,#40997,#40998,#40999),.UNSPECIFIED.,.F.,.F.,(4,3,3,
3,3,3,3,4),(122.066803772211,122.665607680886,123.662889044145,124.660170407405,
125.657451770664,126.654733133923,127.652014497182,128.349989079391),
 .UNSPECIFIED.);
#610=B_SPLINE_CURVE_WITH_KNOTS('',3,(#41004,#41005,#41006,#41007,#41008,
#41009,#41010,#41011,#41012,#41013,#41014,#41015,#41016,#41017,#41018,#41019,
#41020,#41021,#41022,#41023,#41024,#41025),.UNSPECIFIED.,.F.,.F.,(4,3,3,
3,3,3,3,4),(-137.609257848174,-136.627546766515,-135.630265403256,-134.632984039997,
-133.635702676738,-132.638421313479,-131.641139950219,-131.326072540994),
 .UNSPECIFIED.);
#611=B_SPLINE_CURVE_WITH_KNOTS('',3,(#41026,#41027,#41028,#41029,#41030,
#41031,#41032,#41033,#41034,#41035,#41036,#41037,#41038,#41039,#41040,#41041,
#41042,#41043,#41044,#41045,#41046,#41047),.UNSPECIFIED.,.F.,.F.,(4,3,3,
3,3,3,3,4),(128.349989079391,128.649295860442,129.646577223701,130.64385858696,
131.641139950219,132.638421313479,133.635702676738,134.633174386571),
 .UNSPECIFIED.);
#612=B_SPLINE_CURVE_WITH_KNOTS('',3,(#41052,#41053,#41054,#41055,#41056,
#41057,#41058,#41059,#41060,#41061,#41062,#41063,#41064,#41065,#41066,#41067,
#41068,#41069,#41070,#41071,#41072,#41073,#41074,#41075,#41076),
 .UNSPECIFIED.,.F.,.F.,(4,3,3,3,3,3,3,3,4),(-143.892443155353,-143.60851630933,
-142.611234946071,-141.613953582812,-140.616672219552,-139.619390856293,
-138.622109493034,-137.624828129775,-137.609257848174),.UNSPECIFIED.);
#613=B_SPLINE_CURVE_WITH_KNOTS('',3,(#41077,#41078,#41079,#41080,#41081,
#41082,#41083,#41084,#41085,#41086,#41087,#41088,#41089,#41090,#41091,#41092,
#41093,#41094,#41095,#41096,#41097,#41098),.UNSPECIFIED.,.F.,.F.,(4,3,3,
3,3,3,3,4),(134.633174386571,135.630265403256,136.627546766516,137.624828129775,
138.622109493034,139.619390856293,140.616672219552,140.91635969375),
 .UNSPECIFIED.);
#614=B_SPLINE_CURVE_WITH_KNOTS('',3,(#41103,#41104,#41105,#41106,#41107,
#41108,#41109,#41110,#41111,#41112,#41113,#41114,#41115,#41116,#41117,#41118,
#41119,#41120,#41121,#41122,#41123,#41124),.UNSPECIFIED.,.F.,.F.,(4,3,3,
3,3,3,3,4),(-150.175628462533,-149.592204488886,-148.594923125626,-147.597641762367,
-146.600360399108,-145.603079035849,-144.605797672589,-143.892443155353),
 .UNSPECIFIED.);
#615=B_SPLINE_CURVE_WITH_KNOTS('',3,(#41125,#41126,#41127,#41128,#41129,
#41130,#41131,#41132,#41133,#41134,#41135,#41136,#41137,#41138,#41139,#41140,
#41141,#41142,#41143,#41144,#41145,#41146),.UNSPECIFIED.,.F.,.F.,(4,3,3,
3,3,3,3,4),(140.91635969375,141.613953582812,142.611234946071,143.60851630933,
144.605797672589,145.603079035849,146.600360399108,147.19954500093),
 .UNSPECIFIED.);
#616=B_SPLINE_CURVE_WITH_KNOTS('',3,(#41151,#41152,#41153,#41154,#41155,
#41156,#41157,#41158,#41159,#41160,#41161,#41162,#41163,#41164,#41165,#41166,
#41167,#41168,#41169,#41170,#41171,#41172),.UNSPECIFIED.,.F.,.F.,(4,3,3,
3,3,3,3,4),(-156.458813769712,-155.575892668441,-154.578611305182,-153.581329941923,
-152.584048578663,-151.586767215404,-150.589485852145,-150.175628462533),
 .UNSPECIFIED.);
#617=B_SPLINE_CURVE_WITH_KNOTS('',3,(#41173,#41174,#41175,#41176,#41177,
#41178,#41179,#41180,#41181,#41182,#41183,#41184,#41185,#41186,#41187,#41188,
#41189,#41190,#41191,#41192,#41193,#41194),.UNSPECIFIED.,.F.,.F.,(4,3,3,
3,3,3,3,4),(147.19954500093,147.597641762367,148.594923125626,149.592204488886,
150.589485852145,151.586767215404,152.584048578663,153.482730308109),
 .UNSPECIFIED.);
#618=B_SPLINE_CURVE_WITH_KNOTS('',3,(#41199,#41200,#41201,#41202,#41203,
#41204,#41205,#41206,#41207,#41208,#41209,#41210,#41211,#41212,#41213,#41214,
#41215,#41216,#41217,#41218,#41219,#41220,#41221,#41222,#41223),
 .UNSPECIFIED.,.F.,.F.,(4,3,3,3,3,3,3,3,4),(-162.741999076892,-162.556862211256,
-161.559580847996,-160.562299484737,-159.565018121478,-158.567736758219,
-157.570455394959,-156.5731740317,-156.458813769712),.UNSPECIFIED.);
#619=B_SPLINE_CURVE_WITH_KNOTS('',3,(#41224,#41225,#41226,#41227,#41228,
#41229,#41230,#41231,#41232,#41233,#41234,#41235,#41236,#41237,#41238,#41239,
#41240,#41241,#41242,#41243,#41244,#41245,#41246,#41247,#41248),
 .UNSPECIFIED.,.F.,.F.,(4,3,3,3,3,3,3,3,4),(153.482730308109,153.581329941923,
154.578611305182,155.575892668441,156.5731740317,157.57045539496,158.567736758219,
159.565018121478,159.765915615289),.UNSPECIFIED.);
#620=B_SPLINE_CURVE_WITH_KNOTS('',3,(#41253,#41254,#41255,#41256,#41257,
#41258,#41259,#41260,#41261,#41262,#41263,#41264,#41265,#41266,#41267,#41268,
#41269,#41270,#41271,#41272,#41273,#41274),.UNSPECIFIED.,.F.,.F.,(4,3,3,
3,3,3,3,4),(-169.025184384072,-168.540550390811,-167.543269027552,-166.545987664293,
-165.548706301033,-164.551424937774,-163.554143574515,-162.741999076892),
 .UNSPECIFIED.);
#621=B_SPLINE_CURVE_WITH_KNOTS('',3,(#41275,#41276,#41277,#41278,#41279,
#41280,#41281,#41282,#41283,#41284,#41285,#41286,#41287,#41288,#41289,#41290,
#41291,#41292,#41293,#41294,#41295,#41296),.UNSPECIFIED.,.F.,.F.,(4,3,3,
3,3,3,3,4),(159.765915615289,160.562299484737,161.559580847996,162.556862211256,
163.554143574515,164.551424937774,165.548706301033,166.049100922468),
 .UNSPECIFIED.);
#622=B_SPLINE_CURVE_WITH_KNOTS('',3,(#41301,#41302,#41303,#41304,#41305,
#41306,#41307,#41308,#41309,#41310,#41311,#41312,#41313,#41314,#41315,#41316,
#41317,#41318,#41319,#41320,#41321,#41322),.UNSPECIFIED.,.F.,.F.,(4,3,3,
3,3,3,3,4),(-175.308369691251,-174.524238570367,-173.526957207107,-172.529675843848,
-171.532394480589,-170.53511311733,-169.53783175407,-169.025184384072),
 .UNSPECIFIED.);
#623=B_SPLINE_CURVE_WITH_KNOTS('',3,(#41323,#41324,#41325,#41326,#41327,
#41328,#41329,#41330,#41331,#41332,#41333,#41334,#41335,#41336,#41337,#41338,
#41339,#41340,#41341,#41342,#41343,#41344),.UNSPECIFIED.,.F.,.F.,(4,3,3,
3,3,3,3,4),(166.049100922468,166.545987664293,167.543269027552,168.540550390811,
169.53783175407,170.53511311733,171.532394480589,172.332286229648),
 .UNSPECIFIED.);
#624=B_SPLINE_CURVE_WITH_KNOTS('',3,(#41350,#41351,#41352,#41353,#41354,
#41355,#41356),.UNSPECIFIED.,.F.,.F.,(4,1,1,1,4),(191.637151868977,191.850302111352,
192.847583474611,193.84486483787,194.771244901626),.UNSPECIFIED.);
#625=B_SPLINE_CURVE_WITH_KNOTS('',3,(#41359,#41360,#41361,#41362,#41363),
 .UNSPECIFIED.,.F.,.F.,(4,1,4),(191.637151868977,192.532325718813,193.529607082072),
 .UNSPECIFIED.);
#626=B_SPLINE_CURVE_WITH_KNOTS('',3,(#41368,#41369,#41370,#41371,#41372,
#41373,#41374,#41375,#41376,#41377),.UNSPECIFIED.,.F.,.F.,(4,1,1,1,1,1,
1,4),(185.353966561798,185.866613931797,186.863895295056,187.861176658315,
188.858458021574,189.855739384834,190.853020748093,191.637151868977),
 .UNSPECIFIED.);
#627=B_SPLINE_CURVE_WITH_KNOTS('',3,(#41378,#41379,#41380,#41381,#41382,
#41383,#41384,#41385,#41386,#41387,#41388),.UNSPECIFIED.,.F.,.F.,(4,1,1,
1,1,1,1,1,4),(185.353966561798,185.551356175998,186.548637539257,187.545918902517,
188.543200265776,189.540481629035,190.537762992294,191.535044355554,191.637151868977),
 .UNSPECIFIED.);
#628=B_SPLINE_CURVE_WITH_KNOTS('',3,(#41393,#41394,#41395,#41396,#41397,
#41398,#41399,#41400,#41401,#41402),.UNSPECIFIED.,.F.,.F.,(4,1,1,1,1,1,
1,4),(179.070781254618,179.882925752241,180.8802071155,181.87748847876,
182.874769842019,183.872051205278,184.869332568537,185.353966561798),
 .UNSPECIFIED.);
#629=B_SPLINE_CURVE_WITH_KNOTS('',3,(#41403,#41404,#41405,#41406,#41407,
#41408,#41409,#41410,#41411,#41412),.UNSPECIFIED.,.F.,.F.,(4,1,1,1,1,1,
1,4),(179.070781254618,179.567667996443,180.564949359702,181.562230722961,
182.55951208622,183.55679344948,184.554074812739,185.353966561798),
 .UNSPECIFIED.);
#630=B_SPLINE_CURVE_WITH_KNOTS('',3,(#41417,#41418,#41419,#41420,#41421,
#41422,#41423,#41424,#41425,#41426,#41427),.UNSPECIFIED.,.F.,.F.,(4,1,1,
1,1,1,1,1,4),(172.787595947439,172.901956209427,173.899237572686,174.896518935945,
175.893800299204,176.891081662463,177.888363025723,178.885644388982,179.070781254618),
 .UNSPECIFIED.);
#631=B_SPLINE_CURVE_WITH_KNOTS('',3,(#41428,#41429,#41430,#41431,#41432,
#41433,#41434,#41435,#41436,#41437),.UNSPECIFIED.,.F.,.F.,(4,1,1,1,1,1,
1,4),(172.787595947439,173.583979816887,174.581261180147,175.578542543406,
176.575823906665,177.573105269924,178.570386633183,179.070781254618),
 .UNSPECIFIED.);
#632=B_SPLINE_CURVE_WITH_KNOTS('',3,(#41442,#41443,#41444,#41445,#41446,
#41447,#41448,#41449,#41450,#41451),.UNSPECIFIED.,.F.,.F.,(4,1,1,1,1,1,
1,4),(166.504410640259,166.918268029871,167.91554939313,168.91283075639,
169.910112119649,170.907393482908,171.904674846167,172.787595947439),
 .UNSPECIFIED.);
#633=B_SPLINE_CURVE_WITH_KNOTS('',3,(#41452,#41453,#41454,#41455,#41456,
#41457,#41458,#41459,#41460,#41461,#41462),.UNSPECIFIED.,.F.,.F.,(4,1,1,
1,1,1,1,1,4),(166.504410640259,166.603010274073,167.600291637332,168.597573000591,
169.59485436385,170.59213572711,171.589417090369,172.586698453628,172.787595947439),
 .UNSPECIFIED.);
#634=B_SPLINE_CURVE_WITH_KNOTS('',3,(#41467,#41468,#41469,#41470,#41471,
#41472,#41473,#41474,#41475,#41476),.UNSPECIFIED.,.F.,.F.,(4,1,1,1,1,1,
1,4),(160.22122533308,160.934579850316,161.931861213575,162.929142576834,
163.926423940093,164.923705303353,165.920986666612,166.504410640259),
 .UNSPECIFIED.);
#635=B_SPLINE_CURVE_WITH_KNOTS('',3,(#41477,#41478,#41479,#41480,#41481,
#41482,#41483,#41484,#41485,#41486),.UNSPECIFIED.,.F.,.F.,(4,1,1,1,1,1,
1,4),(160.22122533308,160.619322094517,161.616603457776,162.613884821036,
163.611166184295,164.608447547554,165.605728910813,166.504410640259),
 .UNSPECIFIED.);
#636=B_SPLINE_CURVE_WITH_KNOTS('',3,(#41491,#41492,#41493,#41494,#41495,
#41496,#41497,#41498,#41499,#41500,#41501),.UNSPECIFIED.,.F.,.F.,(4,1,1,
1,1,1,1,1,4),(153.9380400259,153.953610307501,154.95089167076,155.948173034019,
156.945454397279,157.942735760538,158.940017123797,159.937298487056,160.22122533308),
 .UNSPECIFIED.);
#637=B_SPLINE_CURVE_WITH_KNOTS('',3,(#41502,#41503,#41504,#41505,#41506,
#41507,#41508,#41509,#41510,#41511),.UNSPECIFIED.,.F.,.F.,(4,1,1,1,1,1,
1,4),(153.9380400259,154.635633914962,155.632915278221,156.63019664148,
157.627478004739,158.624759367999,159.622040731258,160.22122533308),
 .UNSPECIFIED.);
#638=B_SPLINE_CURVE_WITH_KNOTS('',3,(#41516,#41517,#41518,#41519,#41520,
#41521,#41522,#41523,#41524,#41525),.UNSPECIFIED.,.F.,.F.,(4,1,1,1,1,1,
1,4),(147.65485471872,147.969922127946,148.967203491205,149.964484854464,
150.961766217723,151.959047580983,152.956328944242,153.9380400259),
 .UNSPECIFIED.);
#639=B_SPLINE_CURVE_WITH_KNOTS('',3,(#41526,#41527,#41528,#41529,#41530,
#41531,#41532,#41533,#41534,#41535),.UNSPECIFIED.,.F.,.F.,(4,1,1,1,1,1,
1,4),(147.65485471872,148.651945735406,149.649227098666,150.646508461925,
151.643789825184,152.641071188443,153.638352551703,153.9380400259),
 .UNSPECIFIED.);
#640=B_SPLINE_CURVE_WITH_KNOTS('',3,(#41540,#41541,#41542,#41543,#41544,
#41545,#41546,#41547,#41548,#41549),.UNSPECIFIED.,.F.,.F.,(4,1,1,1,1,1,
1,4),(141.371669411541,141.98623394839,142.983515311649,143.980796674909,
144.978078038168,145.975359401427,146.972640764686,147.65485471872),
 .UNSPECIFIED.);
#641=B_SPLINE_CURVE_WITH_KNOTS('',3,(#41550,#41551,#41552,#41553,#41554,
#41555,#41556,#41557,#41558,#41559,#41560),.UNSPECIFIED.,.F.,.F.,(4,1,1,
1,1,1,1,1,4),(141.371669411541,141.670976192592,142.668257555851,143.66553891911,
144.662820282369,145.660101645629,146.657383008888,147.654664372147,147.65485471872),
 .UNSPECIFIED.);
#642=B_SPLINE_CURVE_WITH_KNOTS('',3,(#41565,#41566,#41567,#41568,#41569,
#41570,#41571,#41572,#41573,#41574),.UNSPECIFIED.,.F.,.F.,(4,1,1,1,1,1,
1,4),(135.088484104361,136.002545768835,136.999827132094,137.997108495353,
138.994389858612,139.991671221872,140.988952585131,141.371669411541),
 .UNSPECIFIED.);
#643=B_SPLINE_CURVE_WITH_KNOTS('',3,(#41575,#41576,#41577,#41578,#41579,
#41580,#41581,#41582,#41583,#41584),.UNSPECIFIED.,.F.,.F.,(4,1,1,1,1,1,
1,4),(135.088484104361,135.687288013036,136.684569376296,137.681850739555,
138.679132102814,139.676413466073,140.673694829332,141.371669411541),
 .UNSPECIFIED.);
#644=B_SPLINE_CURVE_WITH_KNOTS('',3,(#41589,#41590,#41591,#41592,#41593,
#41594,#41595,#41596,#41597,#41598,#41599),.UNSPECIFIED.,.F.,.F.,(4,1,1,
1,1,1,1,1,4),(128.805298797182,129.02157622602,130.018857589279,131.016138952539,
132.013420315798,133.010701679057,134.007983042316,135.005264405576,135.088484104361),
 .UNSPECIFIED.);
#645=B_SPLINE_CURVE_WITH_KNOTS('',3,(#41600,#41601,#41602,#41603,#41604,
#41605,#41606,#41607,#41608,#41609),.UNSPECIFIED.,.F.,.F.,(4,1,1,1,1,1,
1,4),(128.805298797182,129.703599833481,130.70088119674,131.698162559999,
132.695443923259,133.692725286518,134.690006649777,135.088484104361),
 .UNSPECIFIED.);
#646=B_SPLINE_CURVE_WITH_KNOTS('',3,(#41614,#41615,#41616,#41617,#41618,
#41619,#41620,#41621,#41622,#41623),.UNSPECIFIED.,.F.,.F.,(4,1,1,1,1,1,
1,4),(122.522113490002,123.037888046465,124.035169409724,125.032450772983,
126.029732136242,127.027013499502,128.024294862761,128.805298797182),
 .UNSPECIFIED.);
#647=B_SPLINE_CURVE_WITH_KNOTS('',3,(#41624,#41625,#41626,#41627,#41628,
#41629,#41630,#41631,#41632,#41633,#41634),.UNSPECIFIED.,.F.,.F.,(4,1,1,
1,1,1,1,1,4),(122.522113490002,122.722630290666,123.719911653925,124.717193017185,
125.714474380444,126.711755743703,127.709037106962,128.706318470222,128.805298797182),
 .UNSPECIFIED.);
#648=B_SPLINE_CURVE_WITH_KNOTS('',3,(#41639,#41640,#41641,#41642,#41643,
#41644,#41645,#41646,#41647,#41648),.UNSPECIFIED.,.F.,.F.,(4,1,1,1,1,1,
1,4),(116.238928182823,117.054199866909,118.051481230168,119.048762593428,
120.046043956687,121.043325319946,122.040606683205,122.522113490002),
 .UNSPECIFIED.);
#649=B_SPLINE_CURVE_WITH_KNOTS('',3,(#41649,#41650,#41651,#41652,#41653,
#41654,#41655,#41656,#41657,#41658),.UNSPECIFIED.,.F.,.F.,(4,1,1,1,1,1,
1,4),(116.238928182823,116.738942111111,117.73622347437,118.733504837629,
119.730786200888,120.728067564148,121.725348927407,122.522113490002),
 .UNSPECIFIED.);
#650=B_SPLINE_CURVE_WITH_KNOTS('',3,(#41663,#41664,#41665,#41666,#41667,
#41668,#41669,#41670,#41671,#41672,#41673),.UNSPECIFIED.,.F.,.F.,(4,1,1,
1,1,1,1,1,4),(109.955742875643,110.073230324095,111.070511687354,112.067793050613,
113.065074413872,114.062355777132,115.059637140391,116.05691850365,116.238928182823),
 .UNSPECIFIED.);
#651=B_SPLINE_CURVE_WITH_KNOTS('',3,(#41674,#41675,#41676,#41677,#41678,
#41679,#41680,#41681,#41682,#41683),.UNSPECIFIED.,.F.,.F.,(4,1,1,1,1,1,
1,4),(109.955742875643,110.755253931555,111.752535294815,112.749816658074,
113.747098021333,114.744379384592,115.741660747852,116.238928182823),
 .UNSPECIFIED.);
#652=B_SPLINE_CURVE_WITH_KNOTS('',3,(#41688,#41689,#41690,#41691,#41692,
#41693,#41694,#41695,#41696,#41697),.UNSPECIFIED.,.F.,.F.,(4,1,1,1,1,1,
1,4),(103.672557568463,104.089542144539,105.086823507798,106.084104871058,
107.081386234317,108.078667597576,109.075948960835,109.955742875643),
 .UNSPECIFIED.);
#653=B_SPLINE_CURVE_WITH_KNOTS('',3,(#41698,#41699,#41700,#41701,#41702,
#41703,#41704,#41705,#41706,#41707,#41708),.UNSPECIFIED.,.F.,.F.,(4,1,1,
1,1,1,1,1,4),(103.672557568463,103.774284388741,104.771565752,105.768847115259,
106.766128478518,107.763409841778,108.760691205037,109.757972568296,109.955742875643),
 .UNSPECIFIED.);
#654=B_SPLINE_CURVE_WITH_KNOTS('',3,(#41713,#41714,#41715,#41716,#41717,
#41718,#41719,#41720,#41721,#41722),.UNSPECIFIED.,.F.,.F.,(4,1,1,1,1,1,
1,4),(97.3893722612837,98.1058539649837,99.103135328243,100.100416691502,
101.097698054761,102.094979418021,103.09226078128,103.672557568463),
 .UNSPECIFIED.);
#655=B_SPLINE_CURVE_WITH_KNOTS('',3,(#41723,#41724,#41725,#41726,#41727,
#41728,#41729,#41730,#41731,#41732),.UNSPECIFIED.,.F.,.F.,(4,1,1,1,1,1,
1,4),(97.3893722612838,97.7905962091853,98.7878775724445,99.7851589357037,
100.782440298963,101.779721662222,102.777003025481,103.672557568463),
 .UNSPECIFIED.);
#656=B_SPLINE_CURVE_WITH_KNOTS('',3,(#41737,#41738,#41739,#41740,#41741,
#41742,#41743,#41744,#41745,#41746,#41747),.UNSPECIFIED.,.F.,.F.,(4,1,1,
1,1,1,1,1,4),(91.1061869541041,91.1248844221691,92.1221657854283,93.1194471486875,
94.1167285119468,95.114009875206,96.1112912384653,97.1085726017245,97.3893722612837),
 .UNSPECIFIED.);
#657=B_SPLINE_CURVE_WITH_KNOTS('',3,(#41748,#41749,#41750,#41751,#41752,
#41753,#41754,#41755,#41756,#41757),.UNSPECIFIED.,.F.,.F.,(4,1,1,1,1,1,
1,4),(91.1061869541042,91.8069080296298,92.8041893928891,93.8014707561483,
94.7987521194075,95.7960334826668,96.793314845926,97.3893722612838),
 .UNSPECIFIED.);
#658=B_SPLINE_CURVE_WITH_KNOTS('',3,(#41762,#41763,#41764,#41765,#41766,
#41767,#41768,#41769,#41770,#41771),.UNSPECIFIED.,.F.,.F.,(4,1,1,1,1,1,
1,4),(84.8230016469246,85.1411962426136,86.1384776058729,87.1357589691321,
88.1330403323914,89.1303216956506,90.1276030589098,91.1061869541041),
 .UNSPECIFIED.);
#659=B_SPLINE_CURVE_WITH_KNOTS('',3,(#41772,#41773,#41774,#41775,#41776,
#41777,#41778,#41779,#41780,#41781,#41782),.UNSPECIFIED.,.F.,.F.,(4,1,1,
1,1,1,1,1,4),(84.8230016469246,84.8259384868152,85.8232198500744,86.8205012133336,
87.8177825765929,88.8150639398521,89.8123453031114,90.8096266663706,91.1061869541042),
 .UNSPECIFIED.);
#660=B_SPLINE_CURVE_WITH_KNOTS('',3,(#41787,#41788,#41789,#41790,#41791,
#41792,#41793,#41794,#41795,#41796),.UNSPECIFIED.,.F.,.F.,(4,1,1,1,1,1,
1,4),(78.539816339745,79.1575080630582,80.1547894263174,81.1520707895767,
82.1493521528359,83.1466335160952,84.1439148793544,84.8230016469246),
 .UNSPECIFIED.);
#661=B_SPLINE_CURVE_WITH_KNOTS('',3,(#41797,#41798,#41799,#41800,#41801,
#41802,#41803,#41804,#41805,#41806),.UNSPECIFIED.,.F.,.F.,(4,1,1,1,1,1,
1,4),(78.539816339745,78.8422503072597,79.839531670519,80.8368130337782,
81.8340943970375,82.8313757602967,83.8286571235559,84.8230016469246),
 .UNSPECIFIED.);
#662=B_SPLINE_CURVE_WITH_KNOTS('',3,(#41811,#41812,#41813,#41814,#41815,
#41816,#41817,#41818,#41819,#41820),.UNSPECIFIED.,.F.,.F.,(4,1,1,1,1,1,
1,4),(72.2566310325654,73.1738198835028,74.171101246762,75.1683826100213,
76.1656639732805,77.1629453365397,78.160226699799,78.539816339745),
 .UNSPECIFIED.);
#663=B_SPLINE_CURVE_WITH_KNOTS('',3,(#41821,#41822,#41823,#41824,#41825,
#41826,#41827,#41828,#41829,#41830),.UNSPECIFIED.,.F.,.F.,(4,1,1,1,1,1,
1,4),(72.2566310325654,72.8585621277043,73.8558434909636,74.8531248542228,
75.850406217482,76.8476875807413,77.8449689440005,78.539816339745),
 .UNSPECIFIED.);
#664=B_SPLINE_CURVE_WITH_KNOTS('',3,(#41835,#41836,#41837,#41838,#41839,
#41840,#41841,#41842,#41843,#41844,#41845),.UNSPECIFIED.,.F.,.F.,(4,1,1,
1,1,1,1,1,4),(65.9734457253857,66.1928503406881,67.1901317039474,68.1874130672066,
69.1846944304658,70.1819757937251,71.1792571569843,72.1765385202436,72.2566310325654),
 .UNSPECIFIED.);
#665=B_SPLINE_CURVE_WITH_KNOTS('',3,(#41846,#41847,#41848,#41849,#41850,
#41851,#41852,#41853,#41854,#41855),.UNSPECIFIED.,.F.,.F.,(4,1,1,1,1,1,
1,4),(65.9734457253858,66.8748739481489,67.8721553114081,68.8694366746674,
69.8667180379266,70.8639994011859,71.8612807644451,72.2566310325654),
 .UNSPECIFIED.);
#666=B_SPLINE_CURVE_WITH_KNOTS('',3,(#41860,#41861,#41862,#41863,#41864,
#41865,#41866,#41867,#41868,#41869),.UNSPECIFIED.,.F.,.F.,(4,1,1,1,1,1,
1,4),(59.6902604182062,60.2091621611327,61.206443524392,62.2037248876512,
63.2010062509104,64.1982876141697,65.1955689774289,65.9734457253857),
 .UNSPECIFIED.);
#667=B_SPLINE_CURVE_WITH_KNOTS('',3,(#41870,#41871,#41872,#41873,#41874,
#41875,#41876,#41877,#41878,#41879,#41880),.UNSPECIFIED.,.F.,.F.,(4,1,1,
1,1,1,1,1,4),(59.6902604182062,59.8939044053342,60.8911857685935,61.8884671318527,
62.8857484951119,63.8830298583712,64.8803112216304,65.8775925848897,65.9734457253858),
 .UNSPECIFIED.);
#668=B_SPLINE_CURVE_WITH_KNOTS('',3,(#41885,#41886,#41887,#41888,#41889,
#41890,#41891,#41892,#41893,#41894),.UNSPECIFIED.,.F.,.F.,(4,1,1,1,1,1,
1,4),(53.4070751110266,54.2254739815773,55.2227553448365,56.2200367080958,
57.217318071355,58.2145994346142,59.2118807978735,59.6902604182062),
 .UNSPECIFIED.);
#669=B_SPLINE_CURVE_WITH_KNOTS('',3,(#41895,#41896,#41897,#41898,#41899,
#41900,#41901,#41902,#41903,#41904),.UNSPECIFIED.,.F.,.F.,(4,1,1,1,1,1,
1,4),(53.4070751110266,53.9102162257788,54.907497589038,55.9047789522973,
56.9020603155565,57.8993416788158,58.896623042075,59.6902604182062),
 .UNSPECIFIED.);
#670=B_SPLINE_CURVE_WITH_KNOTS('',3,(#41909,#41910,#41911,#41912,#41913,
#41914,#41915,#41916,#41917,#41918,#41919),.UNSPECIFIED.,.F.,.F.,(4,1,1,
1,1,1,1,1,4),(47.123889803847,47.2445044387626,48.2417858020219,49.2390671652811,
50.2363485285403,51.2336298917996,52.2309112550588,53.2281926183181,53.4070751110266),
 .UNSPECIFIED.);
#671=B_SPLINE_CURVE_WITH_KNOTS('',3,(#41920,#41921,#41922,#41923,#41924,
#41925,#41926,#41927,#41928,#41929),.UNSPECIFIED.,.F.,.F.,(4,1,1,1,1,1,
1,4),(47.123889803847,47.9265280462234,48.9238094094826,49.9210907727419,
50.9183721360011,51.9156534992603,52.9129348625196,53.4070751110266),
 .UNSPECIFIED.);
#672=B_SPLINE_CURVE_WITH_KNOTS('',3,(#41934,#41935,#41936,#41937,#41938,
#41939,#41940,#41941,#41942,#41943),.UNSPECIFIED.,.F.,.F.,(4,1,1,1,1,1,
1,4),(40.8407044966674,41.2608162592072,42.2580976224665,43.2553789857257,
44.2526603489849,45.2499417122442,46.2472230755034,47.123889803847),
 .UNSPECIFIED.);
#673=B_SPLINE_CURVE_WITH_KNOTS('',3,(#41944,#41945,#41946,#41947,#41948,
#41949,#41950,#41951,#41952,#41953,#41954),.UNSPECIFIED.,.F.,.F.,(4,1,1,
1,1,1,1,1,4),(40.8407044966674,40.9455585034087,41.942839866668,42.9401212299272,
43.9374025931864,44.9346839564457,45.9319653197049,46.9292466829641,47.123889803847),
 .UNSPECIFIED.);
#674=B_SPLINE_CURVE_WITH_KNOTS('',3,(#41959,#41960,#41961,#41962,#41963,
#41964,#41965,#41966,#41967,#41968),.UNSPECIFIED.,.F.,.F.,(4,1,1,1,1,1,
1,4),(34.5575191894878,35.2771280796518,36.274409442911,37.2716908061703,
38.2689721694295,39.2662535326887,40.263534895948,40.8407044966674),
 .UNSPECIFIED.);
#675=B_SPLINE_CURVE_WITH_KNOTS('',3,(#41969,#41970,#41971,#41972,#41973,
#41974,#41975,#41976,#41977,#41978),.UNSPECIFIED.,.F.,.F.,(4,1,1,1,1,1,
1,4),(34.5575191894878,34.9618703238533,35.9591516871125,36.9564330503718,
37.953714413631,38.9509957768902,39.9482771401495,40.8407044966674),
 .UNSPECIFIED.);
#676=B_SPLINE_CURVE_WITH_KNOTS('',3,(#41983,#41984,#41985,#41986,#41987,
#41988,#41989,#41990,#41991,#41992,#41993),.UNSPECIFIED.,.F.,.F.,(4,1,1,
1,1,1,1,1,4),(28.2743338823082,28.2961585368371,29.2934399000964,30.2907212633556,
31.2880026266148,32.2852839898741,33.2825653531333,34.2798467163926,34.5575191894878),
 .UNSPECIFIED.);
#677=B_SPLINE_CURVE_WITH_KNOTS('',3,(#41994,#41995,#41996,#41997,#41998,
#41999,#42000,#42001,#42002,#42003),.UNSPECIFIED.,.F.,.F.,(4,1,1,1,1,1,
1,4),(28.2743338823083,28.9781821442979,29.9754635075571,30.9727448708163,
31.9700262340756,32.9673075973348,33.9645889605941,34.5575191894878),
 .UNSPECIFIED.);
#678=B_SPLINE_CURVE_WITH_KNOTS('',3,(#42008,#42009,#42010,#42011,#42012,
#42013,#42014,#42015,#42016,#42017),.UNSPECIFIED.,.F.,.F.,(4,1,1,1,1,1,
1,4),(21.9911485751286,22.3124703572817,23.3097517205409,24.3070330838002,
25.3043144470594,26.3015958103187,27.2988771735779,28.2743338823082),
 .UNSPECIFIED.);
#679=B_SPLINE_CURVE_WITH_KNOTS('',3,(#42018,#42019,#42020,#42021,#42022,
#42023,#42024,#42025,#42026,#42027,#42028),.UNSPECIFIED.,.F.,.F.,(4,1,1,
1,1,1,1,1,4),(21.9911485751287,21.9972126014832,22.9944939647424,23.9917753280017,
24.9890566912609,25.9863380545202,26.9836194177794,27.9809007810386,28.2743338823083),
 .UNSPECIFIED.);
#680=B_SPLINE_CURVE_WITH_KNOTS('',3,(#42035,#42036,#42037,#42038,#42039,
#42040,#42041,#42042,#42043),.UNSPECIFIED.,.F.,.F.,(4,1,1,1,1,1,4),(16.3287821777263,
17.3260635409855,18.3233449042448,19.320626267504,20.3179076307632,21.3151889940225,
21.9911485751286),.UNSPECIFIED.);
#681=B_SPLINE_CURVE_WITH_KNOTS('',3,(#42044,#42045,#42046,#42047,#42048,
#42049,#42050,#42051,#42052,#42053),.UNSPECIFIED.,.F.,.F.,(4,1,1,1,1,1,
1,4),(15.7079632679491,16.0135244219278,17.010805785187,18.0080871484463,
19.0053685117055,20.0026498749647,20.999931238224,21.9911485751287),
 .UNSPECIFIED.);
#682=B_SPLINE_CURVE_WITH_KNOTS('',3,(#42056,#42057,#42058,#42059,#42060,
#42061,#42062,#42063,#42064,#42065,#42066,#42067,#42068,#42069,#42070,#42071,
#42072,#42073,#42074,#42075,#42076,#42077,#42078,#42079,#42080,#42081,#42082,
#42083,#42084,#42085,#42086,#42087,#42088,#42089,#42090,#42091,#42092,#42093,
#42094,#42095,#42096,#42097,#42098,#42099,#42100,#42101),.UNSPECIFIED.,
 .F.,.F.,(4,3,3,3,3,3,3,3,3,3,3,3,3,3,3,4),(-0.178587760439498,-0.17323124397687,
-0.160983113245847,-0.152353885869142,-0.140321204623344,-0.131822429222877,
-0.111507763274134,-0.104192183870485,-0.0920062408537154,-0.0761220460318835,
-0.066495657095031,-0.0498717428212732,-0.0376847964718908,-0.0291012278395342,
-0.00653686159787477,0.),.UNSPECIFIED.);
#683=B_SPLINE_CURVE_WITH_KNOTS('',3,(#42106,#42107,#42108,#42109,#42110,
#42111,#42112,#42113,#42114,#42115,#42116,#42117,#42118,#42119,#42120,#42121,
#42122,#42123,#42124,#42125,#42126,#42127,#42128,#42129,#42130,#42131,#42132,
#42133,#42134,#42135,#42136,#42137,#42138,#42139,#42140,#42141,#42142,#42143,
#42144,#42145,#42146,#42147,#42148,#42149,#42150,#42151,#42152,#42153,#42154),
 .UNSPECIFIED.,.F.,.F.,(4,3,3,3,3,3,3,3,3,3,3,3,3,3,3,3,4),(-0.177567088092139,
-0.170723718372817,-0.155497180017511,-0.145825010567084,-0.12979337606496,
-0.121643046295364,-0.10085906030943,-0.0933124832844217,-0.0856434724597094,
-0.0800750743234962,-0.0675594968156845,-0.0595371790067273,-0.0397284982519809,
-0.030777491864391,-0.0244620215328627,-0.00609433026311949,0.),
 .UNSPECIFIED.);
#684=B_SPLINE_CURVE_WITH_KNOTS('',3,(#42891,#42892,#42893,#42894,#42895,
#42896,#42897,#42898,#42899,#42900,#42901,#42902,#42903,#42904,#42905,#42906,
#42907,#42908,#42909,#42910,#42911,#42912),.UNSPECIFIED.,.F.,.F.,(4,3,3,
3,3,3,3,4),(172.332286229648,172.529675843848,173.526957207107,174.524238570367,
175.521519933626,176.518801296885,177.516082660144,178.4424627239),
 .UNSPECIFIED.);
#685=B_SPLINE_CURVE_WITH_KNOTS('',3,(#42914,#42915,#42916,#42917,#42918,
#42919,#42920,#42921,#42922,#42923,#42924,#42925,#42926,#42927,#42928,#42929,
#42930,#42931,#42932,#42933,#42934,#42935,#42936,#42937,#42938,#42939,#42940,
#42941,#42942,#42943,#42944,#42945,#42946,#42947,#42948,#42949,#42950,#42951,
#42952,#42953,#42954,#42955,#42956,#42957,#42958,#42959),.UNSPECIFIED.,
 .F.,.F.,(4,3,3,3,3,3,3,3,3,3,3,3,3,3,3,4),(-0.178587760439495,-0.173231243976866,
-0.160983111934104,-0.15235388586526,-0.140321196401713,-0.131822429300813,
-0.111507763491313,-0.104192184639522,-0.0920062408537155,-0.0761220434809652,
-0.0664956565909429,-0.0498717424432072,-0.0376847913304863,-0.0291012266178207,
-0.006536858955891,0.),.UNSPECIFIED.);
#686=B_SPLINE_CURVE_WITH_KNOTS('',3,(#42960,#42961,#42962,#42963),
 .UNSPECIFIED.,.F.,.F.,(4,4),(15.0871443581718,15.7079632679491),
 .UNSPECIFIED.);
#687=B_SPLINE_CURVE_WITH_KNOTS('',3,(#42965,#42966,#42967,#42968,#42969,
#42970,#42971,#42972,#42973,#42974,#42975,#42976,#42977,#42978,#42979,#42980,
#42981,#42982,#42983,#42984,#42985,#42986,#42987,#42988,#42989,#42990,#42991,
#42992,#42993,#42994,#42995,#42996,#42997,#42998,#42999,#43000,#43001,#43002,
#43003,#43004,#43005,#43006,#43007,#43008,#43009,#43010,#43011,#43012,#43013),
 .UNSPECIFIED.,.F.,.F.,(4,3,3,3,3,3,3,3,3,3,3,3,3,3,3,3,4),(-0.177567088092158,
-0.170723718372832,-0.155497179061098,-0.145825009845381,-0.129793369296123,
-0.121643042061732,-0.100859058192623,-0.0933124790575794,-0.0856434713972359,
-0.0800750743235143,-0.0675595120764577,-0.0595372059277545,-0.0397285262789718,
-0.0307775036558628,-0.0244620394540028,-0.00609435183518047,0.),
 .UNSPECIFIED.);
#688=B_SPLINE_CURVE_WITH_KNOTS('',3,(#43752,#43753,#43754,#43755,#43756,
#43757,#43758,#43759,#43760,#43761,#43762,#43763,#43764,#43765,#43766,#43767,
#43768,#43769,#43770),.UNSPECIFIED.,.F.,.F.,(4,3,3,3,3,3,4),(-180.507926749922,
-179.510645386663,-178.513364023404,-177.516082660144,-176.518801296885,
-175.521519933626,-175.308369691251),.UNSPECIFIED.);
#689=B_SPLINE_CURVE_WITH_KNOTS('',3,(#44634,#44635,#44636,#44637,#44638,
#44639,#44640,#44641,#44642,#44643,#44644,#44645,#44646),.UNSPECIFIED.,
 .F.,.F.,(4,3,3,3,4),(-5.66236639740237,-4.96973334046747,-3.97578667237397,
-2.98184000428048,-2.06546402602168),.UNSPECIFIED.);
#690=B_SPLINE_CURVE_WITH_KNOTS('',3,(#44654,#44655,#44656,#44657,#44658,
#44659,#44660,#44661,#44662,#44663),.UNSPECIFIED.,.F.,.F.,(4,3,3,4),(0.,
0.993946668093495,1.98789333618699,2.68628293579895),.UNSPECIFIED.);
#691=B_SPLINE_CURVE_WITH_KNOTS('',3,(#44668,#44669,#44670,#44671,#44672,
#44673,#44674,#44675,#44676,#44677,#44678,#44679,#44680,#44681,#44682,#44683,
#44684,#44685,#44686,#44687,#44688,#44689,#44690,#44691,#44692),
 .UNSPECIFIED.,.F.,.F.,(4,3,3,3,3,3,3,3,4),(-11.945551704582,-11.9273600171219,
-10.9334133490284,-9.93946668093493,-8.94552001284144,-7.95157334474795,
-6.95762667665445,-5.96368000856096,-5.66236639740237),.UNSPECIFIED.);
#692=B_SPLINE_CURVE_WITH_KNOTS('',3,(#44693,#44694,#44695,#44696,#44697,
#44698,#44699,#44700,#44701,#44702,#44703,#44704,#44705,#44706,#44707,#44708,
#44709,#44710,#44711,#44712,#44713,#44714,#44715,#44716,#44717),
 .UNSPECIFIED.,.F.,.F.,(4,3,3,3,3,3,3,3,4),(2.68628293579895,2.98184000428049,
3.97578667237398,4.96973334046747,5.96368000856096,6.95762667665446,7.95157334474795,
8.94552001284145,8.96946824297854),.UNSPECIFIED.);
#693=B_SPLINE_CURVE_WITH_KNOTS('',3,(#44722,#44723,#44724,#44725,#44726,
#44727,#44728,#44729,#44730,#44731,#44732,#44733,#44734,#44735,#44736,#44737,
#44738,#44739,#44740,#44741,#44742,#44743),.UNSPECIFIED.,.F.,.F.,(4,3,3,
3,3,3,3,4),(-18.2287370117615,-17.8910400256829,-16.8970933575894,-15.9031466894959,
-14.9092000214024,-13.9152533533089,-12.9213066852154,-11.945551704582),
 .UNSPECIFIED.);
#694=B_SPLINE_CURVE_WITH_KNOTS('',3,(#44744,#44745,#44746,#44747,#44748,
#44749,#44750,#44751,#44752,#44753,#44754,#44755,#44756,#44757,#44758,#44759,
#44760,#44761,#44762,#44763,#44764,#44765),.UNSPECIFIED.,.F.,.F.,(4,3,3,
3,3,3,3,4),(8.96946824297854,9.93946668093494,10.9334133490284,11.9273600171219,
12.9213066852154,13.9152533533089,14.9092000214024,15.2526535501581),
 .UNSPECIFIED.);
#695=B_SPLINE_CURVE_WITH_KNOTS('',3,(#44770,#44771,#44772,#44773,#44774,
#44775,#44776,#44777,#44778,#44779,#44780,#44781,#44782,#44783,#44784,#44785,
#44786,#44787,#44788,#44789,#44790,#44791),.UNSPECIFIED.,.F.,.F.,(4,3,3,
3,3,3,3,4),(-24.5119223189411,-23.8547200342438,-22.8607733661503,-21.8668266980569,
-20.8728800299634,-19.8789333618699,-18.8849866937764,-18.2287370117615),
 .UNSPECIFIED.);
#696=B_SPLINE_CURVE_WITH_KNOTS('',3,(#44792,#44793,#44794,#44795,#44796,
#44797,#44798,#44799,#44800,#44801,#44802,#44803,#44804,#44805,#44806,#44807,
#44808,#44809,#44810,#44811,#44812,#44813),.UNSPECIFIED.,.F.,.F.,(4,3,3,
3,3,3,3,4),(15.2526535501581,15.9031466894959,16.8970933575894,17.8910400256829,
18.8849866937764,19.8789333618699,20.8728800299634,21.5358388573377),
 .UNSPECIFIED.);
#697=B_SPLINE_CURVE_WITH_KNOTS('',3,(#44818,#44819,#44820,#44821,#44822,
#44823,#44824,#44825,#44826,#44827,#44828,#44829,#44830,#44831,#44832,#44833,
#44834,#44835,#44836,#44837,#44838,#44839),.UNSPECIFIED.,.F.,.F.,(4,3,3,
3,3,3,3,4),(-30.7951076261207,-29.8184000428048,-28.8244533747113,-27.8305067066178,
-26.8365600385243,-25.8426133704308,-24.8486667023373,-24.5119223189411),
 .UNSPECIFIED.);
#698=B_SPLINE_CURVE_WITH_KNOTS('',3,(#44840,#44841,#44842,#44843,#44844,
#44845,#44846,#44847,#44848,#44849,#44850,#44851,#44852,#44853,#44854,#44855,
#44856,#44857,#44858,#44859,#44860,#44861),.UNSPECIFIED.,.F.,.F.,(4,3,3,
3,3,3,3,4),(21.5358388573377,21.8668266980569,22.8607733661503,23.8547200342438,
24.8486667023373,25.8426133704308,26.8365600385243,27.8190241645173),
 .UNSPECIFIED.);
#699=B_SPLINE_CURVE_WITH_KNOTS('',3,(#44866,#44867,#44868,#44869,#44870,
#44871,#44872,#44873,#44874,#44875,#44876,#44877,#44878,#44879,#44880,#44881,
#44882,#44883,#44884,#44885,#44886,#44887,#44888,#44889,#44890),
 .UNSPECIFIED.,.F.,.F.,(4,3,3,3,3,3,3,3,4),(-37.0782929333003,-36.7760267194593,
-35.7820800513658,-34.7881333832723,-33.7941867151788,-32.8002400470853,
-31.8062933789918,-30.8123467108983,-30.7951076261207),.UNSPECIFIED.);
#700=B_SPLINE_CURVE_WITH_KNOTS('',3,(#44891,#44892,#44893,#44894,#44895,
#44896,#44897,#44898,#44899,#44900,#44901,#44902,#44903,#44904,#44905,#44906,
#44907,#44908,#44909,#44910,#44911,#44912,#44913,#44914,#44915),
 .UNSPECIFIED.,.F.,.F.,(4,3,3,3,3,3,3,3,4),(27.8190241645173,27.8305067066178,
28.8244533747113,29.8184000428048,30.8123467108983,31.8062933789918,32.8002400470853,
33.7941867151788,34.1022094716969),.UNSPECIFIED.);
#701=B_SPLINE_CURVE_WITH_KNOTS('',3,(#44920,#44921,#44922,#44923,#44924,
#44925,#44926,#44927,#44928,#44929,#44930,#44931,#44932,#44933,#44934,#44935,
#44936,#44937,#44938,#44939,#44940,#44941),.UNSPECIFIED.,.F.,.F.,(4,3,3,
3,3,3,3,4),(-43.3614782404799,-42.7397067280202,-41.7457600599267,-40.7518133918332,
-39.7578667237397,-38.7639200556462,-37.7699733875527,-37.0782929333003),
 .UNSPECIFIED.);
#702=B_SPLINE_CURVE_WITH_KNOTS('',3,(#44942,#44943,#44944,#44945,#44946,
#44947,#44948,#44949,#44950,#44951,#44952,#44953,#44954,#44955,#44956,#44957,
#44958,#44959,#44960,#44961,#44962,#44963),.UNSPECIFIED.,.F.,.F.,(4,3,3,
3,3,3,3,4),(34.1022094716969,34.7881333832723,35.7820800513658,36.7760267194593,
37.7699733875528,38.7639200556462,39.7578667237397,40.3853947788765),
 .UNSPECIFIED.);
#703=B_SPLINE_CURVE_WITH_KNOTS('',3,(#44968,#44969,#44970,#44971,#44972,
#44973,#44974,#44975,#44976,#44977,#44978,#44979,#44980,#44981,#44982,#44983,
#44984,#44985,#44986,#44987,#44988,#44989),.UNSPECIFIED.,.F.,.F.,(4,3,3,
3,3,3,3,4),(-49.6446635476595,-48.7033867365812,-47.7094400684877,-46.7154934003942,
-45.7215467323007,-44.7276000642072,-43.7336533961137,-43.3614782404799),
 .UNSPECIFIED.);
#704=B_SPLINE_CURVE_WITH_KNOTS('',3,(#44990,#44991,#44992,#44993,#44994,
#44995,#44996,#44997,#44998,#44999,#45000,#45001,#45002,#45003,#45004,#45005,
#45006,#45007,#45008,#45009,#45010,#45011),.UNSPECIFIED.,.F.,.F.,(4,3,3,
3,3,3,3,4),(40.3853947788765,40.7518133918332,41.7457600599267,42.7397067280202,
43.7336533961137,44.7276000642072,45.7215467323007,46.6685800860561),
 .UNSPECIFIED.);
#705=B_SPLINE_CURVE_WITH_KNOTS('',3,(#45016,#45017,#45018,#45019,#45020,
#45021,#45022,#45023,#45024,#45025,#45026,#45027,#45028,#45029,#45030,#45031,
#45032,#45033,#45034,#45035,#45036,#45037,#45038,#45039,#45040),
 .UNSPECIFIED.,.F.,.F.,(4,3,3,3,3,3,3,3,4),(-55.9278488548391,-55.6610134132356,
-54.6670667451421,-53.6731200770486,-52.6791734089552,-51.6852267408617,
-50.6912800727682,-49.6973334046747,-49.6446635476595),.UNSPECIFIED.);
#706=B_SPLINE_CURVE_WITH_KNOTS('',3,(#45041,#45042,#45043,#45044,#45045,
#45046,#45047,#45048,#45049,#45050,#45051,#45052,#45053,#45054,#45055,#45056,
#45057,#45058,#45059,#45060,#45061,#45062,#45063,#45064,#45065),
 .UNSPECIFIED.,.F.,.F.,(4,3,3,3,3,3,3,3,4),(46.6685800860561,46.7154934003942,
47.7094400684877,48.7033867365812,49.6973334046747,50.6912800727682,51.6852267408617,
52.6791734089551,52.9517653932357),.UNSPECIFIED.);
#707=B_SPLINE_CURVE_WITH_KNOTS('',3,(#45070,#45071,#45072,#45073,#45074,
#45075,#45076,#45077,#45078,#45079,#45080,#45081,#45082,#45083,#45084,#45085,
#45086,#45087,#45088,#45089,#45090,#45091),.UNSPECIFIED.,.F.,.F.,(4,3,3,
3,3,3,3,4),(-62.2110341620187,-61.6246934217966,-60.6307467537031,-59.6368000856096,
-58.6428534175161,-57.6489067494226,-56.6549600813291,-55.9278488548391),
 .UNSPECIFIED.);
#708=B_SPLINE_CURVE_WITH_KNOTS('',3,(#45092,#45093,#45094,#45095,#45096,
#45097,#45098,#45099,#45100,#45101,#45102,#45103,#45104,#45105,#45106,#45107,
#45108,#45109,#45110,#45111,#45112,#45113),.UNSPECIFIED.,.F.,.F.,(4,3,3,
3,3,3,3,4),(52.9517653932357,53.6731200770486,54.6670667451421,55.6610134132356,
56.6549600813291,57.6489067494226,58.6428534175161,59.2349507004152),
 .UNSPECIFIED.);
#709=B_SPLINE_CURVE_WITH_KNOTS('',3,(#45118,#45119,#45120,#45121,#45122,
#45123,#45124,#45125,#45126,#45127,#45128,#45129,#45130,#45131,#45132,#45133,
#45134,#45135,#45136,#45137,#45138,#45139),.UNSPECIFIED.,.F.,.F.,(4,3,3,
3,3,3,3,4),(-68.4942194691983,-67.5883734303575,-66.5944267622641,-65.6004800941705,
-64.6065334260771,-63.6125867579836,-62.6186400898901,-62.2110341620187),
 .UNSPECIFIED.);
#710=B_SPLINE_CURVE_WITH_KNOTS('',3,(#45140,#45141,#45142,#45143,#45144,
#45145,#45146,#45147,#45148,#45149,#45150,#45151,#45152,#45153,#45154,#45155,
#45156,#45157,#45158,#45159,#45160,#45161),.UNSPECIFIED.,.F.,.F.,(4,3,3,
3,3,3,3,4),(59.2349507004152,59.6368000856096,60.6307467537031,61.6246934217966,
62.6186400898901,63.6125867579836,64.6065334260771,65.5181360075948),
 .UNSPECIFIED.);
#711=B_SPLINE_CURVE_WITH_KNOTS('',3,(#45166,#45167,#45168,#45169,#45170,
#45171,#45172,#45173,#45174,#45175,#45176,#45177,#45178,#45179,#45180,#45181,
#45182,#45183,#45184,#45185,#45186,#45187,#45188,#45189,#45190),
 .UNSPECIFIED.,.F.,.F.,(4,3,3,3,3,3,3,3,4),(-74.7774047763779,-74.546000107012,
-73.5520534389185,-72.558106770825,-71.5641601027315,-70.570213434638,-69.5762667665445,
-68.582320098451,-68.4942194691983),.UNSPECIFIED.);
#712=B_SPLINE_CURVE_WITH_KNOTS('',3,(#45191,#45192,#45193,#45194,#45195,
#45196,#45197,#45198,#45199,#45200,#45201,#45202,#45203,#45204,#45205,#45206,
#45207,#45208,#45209,#45210,#45211,#45212,#45213,#45214,#45215),
 .UNSPECIFIED.,.F.,.F.,(4,3,3,3,3,3,3,3,4),(65.5181360075948,65.6004800941706,
66.5944267622641,67.5883734303575,68.582320098451,69.5762667665445,70.570213434638,
71.5641601027315,71.8013213147744),.UNSPECIFIED.);
#713=B_SPLINE_CURVE_WITH_KNOTS('',3,(#45220,#45221,#45222,#45223,#45224,
#45225,#45226,#45227,#45228,#45229,#45230,#45231,#45232,#45233,#45234,#45235,
#45236,#45237,#45238,#45239,#45240,#45241),.UNSPECIFIED.,.F.,.F.,(4,3,3,
3,3,3,3,4),(-81.0605900835575,-80.5096801155729,-79.5157334474794,-78.521786779386,
-77.5278401112925,-76.533893443199,-75.5399467751055,-74.7774047763779),
 .UNSPECIFIED.);
#714=B_SPLINE_CURVE_WITH_KNOTS('',3,(#45242,#45243,#45244,#45245,#45246,
#45247,#45248,#45249,#45250,#45251,#45252,#45253,#45254,#45255,#45256,#45257,
#45258,#45259,#45260,#45261,#45262,#45263),.UNSPECIFIED.,.F.,.F.,(4,3,3,
3,3,3,3,4),(71.8013213147744,72.558106770825,73.5520534389185,74.546000107012,
75.5399467751055,76.533893443199,77.5278401112925,78.084506621954),
 .UNSPECIFIED.);
#715=B_SPLINE_CURVE_WITH_KNOTS('',3,(#45268,#45269,#45270,#45271,#45272,
#45273,#45274,#45275,#45276,#45277,#45278,#45279,#45280,#45281,#45282,#45283,
#45284,#45285,#45286,#45287,#45288,#45289),.UNSPECIFIED.,.F.,.F.,(4,3,3,
3,3,3,3,4),(-87.343775390737,-86.4733601241339,-85.4794134560404,-84.4854667879469,
-83.4915201198534,-82.4975734517599,-81.5036267836664,-81.0605900835575),
 .UNSPECIFIED.);
#716=B_SPLINE_CURVE_WITH_KNOTS('',3,(#45290,#45291,#45292,#45293,#45294,
#45295,#45296,#45297,#45298,#45299,#45300,#45301,#45302,#45303,#45304,#45305,
#45306,#45307,#45308,#45309,#45310,#45311),.UNSPECIFIED.,.F.,.F.,(4,3,3,
3,3,3,3,4),(78.084506621954,78.521786779386,79.5157334474795,80.509680115573,
81.5036267836665,82.4975734517599,83.4915201198534,84.3676919291336),
 .UNSPECIFIED.);
#717=B_SPLINE_CURVE_WITH_KNOTS('',3,(#45316,#45317,#45318,#45319,#45320,
#45321,#45322,#45323,#45324,#45325,#45326,#45327,#45328,#45329,#45330,#45331,
#45332,#45333,#45334,#45335,#45336,#45337,#45338,#45339,#45340),
 .UNSPECIFIED.,.F.,.F.,(4,3,3,3,3,3,3,3,4),(-93.6269606979166,-93.4309868007884,
-92.4370401326949,-91.4430934646014,-90.4491467965079,-89.4552001284144,
-88.4612534603209,-87.4673067922274,-87.343775390737),.UNSPECIFIED.);
#718=B_SPLINE_CURVE_WITH_KNOTS('',3,(#45341,#45342,#45343,#45344,#45345,
#45346,#45347,#45348,#45349,#45350,#45351,#45352,#45353,#45354,#45355,#45356,
#45357,#45358,#45359,#45360,#45361,#45362,#45363,#45364,#45365),
 .UNSPECIFIED.,.F.,.F.,(4,3,3,3,3,3,3,3,4),(84.3676919291336,84.4854667879469,
85.4794134560404,86.4733601241339,87.4673067922274,88.4612534603209,89.4552001284144,
90.4491467965079,90.6508772363132),.UNSPECIFIED.);
#719=B_SPLINE_CURVE_WITH_KNOTS('',3,(#45370,#45371,#45372,#45373,#45374,
#45375,#45376,#45377,#45378,#45379,#45380,#45381,#45382,#45383,#45384,#45385,
#45386,#45387,#45388,#45389,#45390,#45391),.UNSPECIFIED.,.F.,.F.,(4,3,3,
3,3,3,3,4),(-99.9101460050962,-99.3946668093493,-98.4007201412558,-97.4067734731623,
-96.4128268050689,-95.4188801369753,-94.4249334688819,-93.6269606979166),
 .UNSPECIFIED.);
#720=B_SPLINE_CURVE_WITH_KNOTS('',3,(#45392,#45393,#45394,#45395,#45396,
#45397,#45398,#45399,#45400,#45401,#45402,#45403,#45404,#45405,#45406,#45407,
#45408,#45409,#45410,#45411,#45412,#45413),.UNSPECIFIED.,.F.,.F.,(4,3,3,
3,3,3,3,4),(90.6508772363132,91.4430934646014,92.4370401326949,93.4309868007884,
94.4249334688819,95.4188801369754,96.4128268050689,96.9340625434928),
 .UNSPECIFIED.);
#721=B_SPLINE_CURVE_WITH_KNOTS('',3,(#45418,#45419,#45420,#45421,#45422,
#45423,#45424,#45425,#45426,#45427,#45428,#45429,#45430,#45431,#45432,#45433,
#45434,#45435,#45436,#45437,#45438,#45439),.UNSPECIFIED.,.F.,.F.,(4,3,3,
3,3,3,3,4),(-106.193331312276,-105.35834681791,-104.364400149817,-103.370453481723,
-102.37650681363,-101.382560145536,-100.388613477443,-99.9101460050962),
 .UNSPECIFIED.);
#722=B_SPLINE_CURVE_WITH_KNOTS('',3,(#45440,#45441,#45442,#45443,#45444,
#45445,#45446,#45447,#45448,#45449,#45450,#45451,#45452,#45453,#45454,#45455,
#45456,#45457,#45458,#45459,#45460,#45461),.UNSPECIFIED.,.F.,.F.,(4,3,3,
3,3,3,3,4),(96.9340625434928,97.4067734731624,98.4007201412558,99.3946668093493,
100.388613477443,101.382560145536,102.37650681363,103.217247850672),
 .UNSPECIFIED.);
#723=B_SPLINE_CURVE_WITH_KNOTS('',3,(#45466,#45467,#45468,#45469,#45470,
#45471,#45472,#45473,#45474,#45475,#45476,#45477,#45478,#45479,#45480,#45481,
#45482,#45483,#45484,#45485,#45486,#45487,#45488,#45489,#45490),
 .UNSPECIFIED.,.F.,.F.,(4,3,3,3,3,3,3,3,4),(-112.476516619455,-112.315973494565,
-111.322026826471,-110.328080158378,-109.334133490284,-108.340186822191,
-107.346240154097,-106.352293486004,-106.193331312276),.UNSPECIFIED.);
#724=B_SPLINE_CURVE_WITH_KNOTS('',3,(#45491,#45492,#45493,#45494,#45495,
#45496,#45497,#45498,#45499,#45500,#45501,#45502,#45503,#45504,#45505,#45506,
#45507,#45508,#45509,#45510,#45511,#45512,#45513,#45514,#45515),
 .UNSPECIFIED.,.F.,.F.,(4,3,3,3,3,3,3,3,4),(103.217247850672,103.370453481723,
104.364400149817,105.35834681791,106.352293486004,107.346240154097,108.340186822191,
109.334133490284,109.500433157852),.UNSPECIFIED.);
#725=B_SPLINE_CURVE_WITH_KNOTS('',3,(#45520,#45521,#45522,#45523,#45524,
#45525,#45526,#45527,#45528,#45529,#45530,#45531,#45532,#45533,#45534,#45535,
#45536,#45537,#45538,#45539,#45540,#45541),.UNSPECIFIED.,.F.,.F.,(4,3,3,
3,3,3,3,4),(-118.759701926635,-118.279653503126,-117.285706835032,-116.291760166939,
-115.297813498845,-114.303866830752,-113.309920162658,-112.476516619455),
 .UNSPECIFIED.);
#726=B_SPLINE_CURVE_WITH_KNOTS('',3,(#45542,#45543,#45544,#45545,#45546,
#45547,#45548,#45549,#45550,#45551,#45552,#45553,#45554,#45555,#45556,#45557,
#45558,#45559,#45560,#45561,#45562,#45563),.UNSPECIFIED.,.F.,.F.,(4,3,3,
3,3,3,3,4),(109.500433157852,110.328080158378,111.322026826471,112.315973494565,
113.309920162658,114.303866830752,115.297813498845,115.783618465032),
 .UNSPECIFIED.);
#727=B_SPLINE_CURVE_WITH_KNOTS('',3,(#45568,#45569,#45570,#45571,#45572,
#45573,#45574,#45575,#45576,#45577,#45578,#45579,#45580,#45581,#45582,#45583,
#45584,#45585,#45586,#45587,#45588,#45589),.UNSPECIFIED.,.F.,.F.,(4,3,3,
3,3,3,3,4),(-125.042887233815,-124.243333511687,-123.249386843593,-122.2554401755,
-121.261493507406,-120.267546839313,-119.273600171219,-118.759701926635),
 .UNSPECIFIED.);
#728=B_SPLINE_CURVE_WITH_KNOTS('',3,(#45590,#45591,#45592,#45593,#45594,
#45595,#45596,#45597,#45598,#45599,#45600,#45601,#45602,#45603,#45604,#45605,
#45606,#45607,#45608,#45609,#45610,#45611),.UNSPECIFIED.,.F.,.F.,(4,3,3,
3,3,3,3,4),(115.783618465032,116.291760166939,117.285706835032,118.279653503126,
119.273600171219,120.267546839313,121.261493507406,122.066803772211),
 .UNSPECIFIED.);
#729=B_SPLINE_CURVE_WITH_KNOTS('',3,(#45616,#45617,#45618,#45619,#45620,
#45621,#45622,#45623,#45624,#45625,#45626,#45627,#45628,#45629,#45630,#45631,
#45632,#45633,#45634,#45635,#45636,#45637,#45638,#45639,#45640),
 .UNSPECIFIED.,.F.,.F.,(4,3,3,3,3,3,3,3,4),(-131.326072540994,-131.200960188341,
-130.207013520248,-129.213066852154,-128.219120184061,-127.225173515967,
-126.231226847874,-125.23728017978,-125.042887233815),.UNSPECIFIED.);
#730=B_SPLINE_CURVE_WITH_KNOTS('',3,(#45641,#45642,#45643,#45644,#45645,
#45646,#45647,#45648,#45649,#45650,#45651,#45652,#45653,#45654,#45655,#45656,
#45657,#45658,#45659,#45660,#45661,#45662,#45663,#45664,#45665),
 .UNSPECIFIED.,.F.,.F.,(4,3,3,3,3,3,3,3,4),(122.066803772211,122.2554401755,
123.249386843593,124.243333511687,125.23728017978,126.231226847874,127.225173515967,
128.219120184061,128.349989079391),.UNSPECIFIED.);
#731=B_SPLINE_CURVE_WITH_KNOTS('',3,(#45670,#45671,#45672,#45673,#45674,
#45675,#45676,#45677,#45678,#45679,#45680,#45681,#45682,#45683,#45684,#45685,
#45686,#45687,#45688,#45689,#45690,#45691),.UNSPECIFIED.,.F.,.F.,(4,3,3,
3,3,3,3,4),(-137.609257848174,-137.164640196902,-136.170693528809,-135.176746860715,
-134.182800192622,-133.188853524528,-132.194906856435,-131.326072540994),
 .UNSPECIFIED.);
#732=B_SPLINE_CURVE_WITH_KNOTS('',3,(#45692,#45693,#45694,#45695,#45696,
#45697,#45698,#45699,#45700,#45701,#45702,#45703,#45704,#45705,#45706,#45707,
#45708,#45709,#45710,#45711,#45712,#45713),.UNSPECIFIED.,.F.,.F.,(4,3,3,
3,3,3,3,4),(128.349989079391,129.213066852154,130.207013520248,131.200960188341,
132.194906856435,133.188853524528,134.182800192622,134.63317438657),
 .UNSPECIFIED.);
#733=B_SPLINE_CURVE_WITH_KNOTS('',3,(#45718,#45719,#45720,#45721,#45722,
#45723,#45724,#45725,#45726,#45727,#45728,#45729,#45730,#45731,#45732,#45733,
#45734,#45735,#45736,#45737,#45738,#45739),.UNSPECIFIED.,.F.,.F.,(4,3,3,
3,3,3,3,4),(-143.892443155353,-143.128320205463,-142.13437353737,-141.140426869276,
-140.146480201183,-139.152533533089,-138.158586864996,-137.609257848174),
 .UNSPECIFIED.);
#734=B_SPLINE_CURVE_WITH_KNOTS('',3,(#45740,#45741,#45742,#45743,#45744,
#45745,#45746,#45747,#45748,#45749,#45750,#45751,#45752,#45753,#45754,#45755,
#45756,#45757,#45758,#45759,#45760,#45761),.UNSPECIFIED.,.F.,.F.,(4,3,3,
3,3,3,3,4),(134.63317438657,135.176746860715,136.170693528809,137.164640196902,
138.158586864996,139.152533533089,140.146480201183,140.91635969375),
 .UNSPECIFIED.);
#735=B_SPLINE_CURVE_WITH_KNOTS('',3,(#45767,#45768,#45769,#45770,#45771,
#45772,#45773),.UNSPECIFIED.,.F.,.F.,(4,1,1,1,4),(160.221225333079,160.451049051283,
161.444995719376,162.43894238747,163.355318365728),.UNSPECIFIED.);
#736=B_SPLINE_CURVE_WITH_KNOTS('',3,(#45776,#45777,#45778,#45779,#45780),
 .UNSPECIFIED.,.F.,.F.,(4,1,4),(160.221225333079,161.119733878081,162.113680546174),
 .UNSPECIFIED.);
#737=B_SPLINE_CURVE_WITH_KNOTS('',3,(#45785,#45786,#45787,#45788,#45789,
#45790,#45791,#45792,#45793,#45794),.UNSPECIFIED.,.F.,.F.,(4,1,1,1,1,1,
1,4),(153.9380400259,154.487369042722,155.481315710815,156.475262378909,
157.469209047002,158.463155715096,159.457102383189,160.221225333079),
 .UNSPECIFIED.);
#738=B_SPLINE_CURVE_WITH_KNOTS('',3,(#45795,#45796,#45797,#45798,#45799,
#45800,#45801,#45802,#45803,#45804,#45805),.UNSPECIFIED.,.F.,.F.,(4,1,1,
1,1,1,1,1,4),(153.9380400259,154.162107201426,155.15605386952,156.150000537613,
157.143947205707,158.1378938738,159.131840541894,160.125787209987,160.221225333079),
 .UNSPECIFIED.);
#739=B_SPLINE_CURVE_WITH_KNOTS('',3,(#45810,#45811,#45812,#45813,#45814,
#45815,#45816,#45817,#45818,#45819),.UNSPECIFIED.,.F.,.F.,(4,1,1,1,1,1,
1,4),(147.65485471872,148.523689034161,149.517635702254,150.511582370348,
151.505529038441,152.499475706535,153.493422374628,153.9380400259),
 .UNSPECIFIED.);
#740=B_SPLINE_CURVE_WITH_KNOTS('',3,(#45820,#45821,#45822,#45823,#45824,
#45825,#45826,#45827,#45828,#45829),.UNSPECIFIED.,.F.,.F.,(4,1,1,1,1,1,
1,4),(147.65485471872,148.198427192865,149.192373860959,150.186320529052,
151.180267197146,152.174213865239,153.168160533333,153.9380400259),
 .UNSPECIFIED.);
#741=B_SPLINE_CURVE_WITH_KNOTS('',3,(#45834,#45835,#45836,#45837,#45838,
#45839,#45840,#45841,#45842,#45843,#45844),.UNSPECIFIED.,.F.,.F.,(4,1,1,
1,1,1,1,1,4),(141.371669411541,141.566062357506,142.5600090256,143.553955693693,
144.547902361787,145.54184902988,146.535795697974,147.529742366067,147.65485471872),
 .UNSPECIFIED.);
#742=B_SPLINE_CURVE_WITH_KNOTS('',3,(#45845,#45846,#45847,#45848,#45849,
#45850,#45851,#45852,#45853,#45854),.UNSPECIFIED.,.F.,.F.,(4,1,1,1,1,1,
1,4),(141.371669411541,142.234747184304,143.228693852398,144.222640520491,
145.216587188585,146.210533856678,147.204480524772,147.65485471872),
 .UNSPECIFIED.);
#743=B_SPLINE_CURVE_WITH_KNOTS('',3,(#45859,#45860,#45861,#45862,#45863,
#45864,#45865,#45866,#45867,#45868),.UNSPECIFIED.,.F.,.F.,(4,1,1,1,1,1,
1,4),(135.088484104361,135.602382348945,136.596329017039,137.590275685132,
138.584222353226,139.578169021319,140.572115689413,141.371669411541),
 .UNSPECIFIED.);
#744=B_SPLINE_CURVE_WITH_KNOTS('',3,(#45869,#45870,#45871,#45872,#45873,
#45874,#45875,#45876,#45877,#45878,#45879),.UNSPECIFIED.,.F.,.F.,(4,1,1,
1,1,1,1,1,4),(135.088484104361,135.27712050765,136.271067175743,137.265013843837,
138.25896051193,139.252907180024,140.246853848117,141.240800516211,141.371669411541),
 .UNSPECIFIED.);
#745=B_SPLINE_CURVE_WITH_KNOTS('',3,(#45884,#45885,#45886,#45887,#45888,
#45889,#45890,#45891,#45892,#45893),.UNSPECIFIED.,.F.,.F.,(4,1,1,1,1,1,
1,4),(128.805298797182,129.638702340384,130.632649008478,131.626595676571,
132.620542344665,133.614489012758,134.608435680852,135.088484104361),
 .UNSPECIFIED.);
#746=B_SPLINE_CURVE_WITH_KNOTS('',3,(#45894,#45895,#45896,#45897,#45898,
#45899,#45900,#45901,#45902,#45903),.UNSPECIFIED.,.F.,.F.,(4,1,1,1,1,1,
1,4),(128.805298797182,129.313440499089,130.307387167182,131.301333835276,
132.295280503369,133.289227171463,134.283173839556,135.088484104361),
 .UNSPECIFIED.);
#747=B_SPLINE_CURVE_WITH_KNOTS('',3,(#45908,#45909,#45910,#45911,#45912,
#45913,#45914,#45915,#45916,#45917,#45918),.UNSPECIFIED.,.F.,.F.,(4,1,1,
1,1,1,1,1,4),(122.522113490002,122.68107566373,123.675022331823,124.668968999917,
125.66291566801,126.656862336104,127.650809004197,128.644755672291,128.805298797182),
 .UNSPECIFIED.);
#748=B_SPLINE_CURVE_WITH_KNOTS('',3,(#45919,#45920,#45921,#45922,#45923,
#45924,#45925,#45926,#45927,#45928),.UNSPECIFIED.,.F.,.F.,(4,1,1,1,1,1,
1,4),(122.522113490002,123.349760490528,124.343707158621,125.337653826715,
126.331600494808,127.325547162902,128.319493830995,128.805298797182),
 .UNSPECIFIED.);
#749=B_SPLINE_CURVE_WITH_KNOTS('',3,(#45933,#45934,#45935,#45936,#45937,
#45938,#45939,#45940,#45941,#45942),.UNSPECIFIED.,.F.,.F.,(4,1,1,1,1,1,
1,4),(116.238928182822,116.717395655169,117.711342323262,118.705288991356,
119.699235659449,120.693182327543,121.687128995636,122.522113490002),
 .UNSPECIFIED.);
#750=B_SPLINE_CURVE_WITH_KNOTS('',3,(#45943,#45944,#45945,#45946,#45947,
#45948,#45949,#45950,#45951,#45952,#45953),.UNSPECIFIED.,.F.,.F.,(4,1,1,
1,1,1,1,1,4),(116.238928182822,116.392133813873,117.386080481967,118.38002715006,
119.373973818154,120.367920486247,121.361867154341,122.355813822434,122.522113490002),
 .UNSPECIFIED.);
#751=B_SPLINE_CURVE_WITH_KNOTS('',3,(#45958,#45959,#45960,#45961,#45962,
#45963,#45964,#45965,#45966,#45967),.UNSPECIFIED.,.F.,.F.,(4,1,1,1,1,1,
1,4),(109.955742875643,110.753715646608,111.747662314702,112.741608982795,
113.735555650889,114.729502318982,115.723448987075,116.238928182822),
 .UNSPECIFIED.);
#752=B_SPLINE_CURVE_WITH_KNOTS('',3,(#45968,#45969,#45970,#45971,#45972,
#45973,#45974,#45975,#45976,#45977),.UNSPECIFIED.,.F.,.F.,(4,1,1,1,1,1,
1,4),(109.955742875643,110.428453805312,111.422400473406,112.416347141499,
113.410293809593,114.404240477686,115.39818714578,116.238928182822),
 .UNSPECIFIED.);
#753=B_SPLINE_CURVE_WITH_KNOTS('',3,(#45982,#45983,#45984,#45985,#45986,
#45987,#45988,#45989,#45990,#45991,#45992),.UNSPECIFIED.,.F.,.F.,(4,1,1,
1,1,1,1,1,4),(103.672557568463,103.796088969954,104.790035638047,105.783982306141,
106.777928974234,107.771875642328,108.765822310421,109.759768978515,109.955742875643),
 .UNSPECIFIED.);
#754=B_SPLINE_CURVE_WITH_KNOTS('',3,(#45993,#45994,#45995,#45996,#45997,
#45998,#45999,#46000,#46001,#46002),.UNSPECIFIED.,.F.,.F.,(4,1,1,1,1,1,
1,4),(103.672557568463,104.464773796751,105.458720464845,106.452667132938,
107.446613801032,108.440560469125,109.434507137219,109.955742875643),
 .UNSPECIFIED.);
#755=B_SPLINE_CURVE_WITH_KNOTS('',3,(#46007,#46008,#46009,#46010,#46011,
#46012,#46013,#46014,#46015,#46016),.UNSPECIFIED.,.F.,.F.,(4,1,1,1,1,1,
1,4),(97.3893722612836,97.8324089613926,98.8263556294861,99.8203022975796,
100.814248965673,101.808195633767,102.80214230186,103.672557568463),
 .UNSPECIFIED.);
#756=B_SPLINE_CURVE_WITH_KNOTS('',3,(#46017,#46018,#46019,#46020,#46021,
#46022,#46023,#46024,#46025,#46026,#46027),.UNSPECIFIED.,.F.,.F.,(4,1,1,
1,1,1,1,1,4),(97.3893722612836,97.5071471200969,98.5010937881904,99.4950404562839,
100.488987124377,101.482933792471,102.476880460564,103.470827128658,103.672557568463),
 .UNSPECIFIED.);
#757=B_SPLINE_CURVE_WITH_KNOTS('',3,(#46032,#46033,#46034,#46035,#46036,
#46037,#46038,#46039,#46040,#46041),.UNSPECIFIED.,.F.,.F.,(4,1,1,1,1,1,
1,4),(91.106186954104,91.8687289528317,92.8626756209252,93.8566222890186,
94.8505689571121,95.8445156252056,96.8384622932991,97.3893722612836),
 .UNSPECIFIED.);
#758=B_SPLINE_CURVE_WITH_KNOTS('',3,(#46042,#46043,#46044,#46045,#46046,
#46047,#46048,#46049,#46050,#46051),.UNSPECIFIED.,.F.,.F.,(4,1,1,1,1,1,
1,4),(91.106186954104,91.543467111536,92.5374137796295,93.5313604477229,
94.5253071158164,95.5192537839099,96.5132004520034,97.3893722612836),
 .UNSPECIFIED.);
#759=B_SPLINE_CURVE_WITH_KNOTS('',3,(#46056,#46057,#46058,#46059,#46060,
#46061,#46062,#46063,#46064,#46065,#46066),.UNSPECIFIED.,.F.,.F.,(4,1,1,
1,1,1,1,1,4),(84.8230016469245,84.9111022761772,85.9050489442707,86.8989956123642,
87.8929422804577,88.8868889485512,89.8808356166447,90.8747822847382,91.106186954104),
 .UNSPECIFIED.);
#760=B_SPLINE_CURVE_WITH_KNOTS('',3,(#46067,#46068,#46069,#46070,#46071,
#46072,#46073,#46074,#46075,#46076),.UNSPECIFIED.,.F.,.F.,(4,1,1,1,1,1,
1,4),(84.8230016469245,85.579787102975,86.5737337710685,87.567680439162,
88.5616271072555,89.555573775349,90.5495204434425,91.106186954104),
 .UNSPECIFIED.);
#761=B_SPLINE_CURVE_WITH_KNOTS('',3,(#46081,#46082,#46083,#46084,#46085,
#46086,#46087,#46088,#46089,#46090),.UNSPECIFIED.,.F.,.F.,(4,1,1,1,1,1,
1,4),(78.5398163397449,78.9474222676163,79.9413689357097,80.9353156038032,
81.9292622718967,82.9232089399902,83.9171556080837,84.8230016469245),
 .UNSPECIFIED.);
#762=B_SPLINE_CURVE_WITH_KNOTS('',3,(#46091,#46092,#46093,#46094,#46095,
#46096,#46097,#46098,#46099,#46100,#46101),.UNSPECIFIED.,.F.,.F.,(4,1,1,
1,1,1,1,1,4),(78.5398163397449,78.6221604263205,79.616107094414,80.6100537625075,
81.604000430601,82.5979470986945,83.591893766788,84.5858404348815,84.8230016469245),
 .UNSPECIFIED.);
#763=B_SPLINE_CURVE_WITH_KNOTS('',3,(#46106,#46107,#46108,#46109,#46110,
#46111,#46112,#46113,#46114,#46115),.UNSPECIFIED.,.F.,.F.,(4,1,1,1,1,1,
1,4),(72.2566310325653,72.9837422590553,73.9776889271488,74.9716355952423,
75.9655822633358,76.9595289314293,77.9534755995228,78.5398163397449),
 .UNSPECIFIED.);
#764=B_SPLINE_CURVE_WITH_KNOTS('',3,(#46116,#46117,#46118,#46119,#46120,
#46121,#46122,#46123,#46124,#46125),.UNSPECIFIED.,.F.,.F.,(4,1,1,1,1,1,
1,4),(72.2566310325653,72.6584804177596,73.6524270858531,74.6463737539466,
75.6403204220401,76.6342670901336,77.6282137582271,78.5398163397449),
 .UNSPECIFIED.);
#765=B_SPLINE_CURVE_WITH_KNOTS('',3,(#46130,#46131,#46132,#46133,#46134,
#46135,#46136,#46137,#46138,#46139,#46140),.UNSPECIFIED.,.F.,.F.,(4,1,1,
1,1,1,1,1,4),(65.9734457253857,66.0261155824008,67.0200622504943,68.0140089185878,
69.0079555866813,70.0019022547748,70.9958489228683,71.9897955909618,72.2566310325653),
 .UNSPECIFIED.);
#766=B_SPLINE_CURVE_WITH_KNOTS('',3,(#46141,#46142,#46143,#46144,#46145,
#46146,#46147,#46148,#46149,#46150),.UNSPECIFIED.,.F.,.F.,(4,1,1,1,1,1,
1,4),(65.9734457253857,66.6948004091986,67.6887470772921,68.6826937453856,
69.6766404134791,70.6705870815726,71.6645337496661,72.2566310325653),
 .UNSPECIFIED.);
#767=B_SPLINE_CURVE_WITH_KNOTS('',3,(#46155,#46156,#46157,#46158,#46159,
#46160,#46161,#46162,#46163,#46164),.UNSPECIFIED.,.F.,.F.,(4,1,1,1,1,1,
1,4),(59.6902604182061,60.0624355738399,61.0563822419334,62.0503289100269,
63.0442755781204,64.0382222462139,65.0321689143073,65.9734457253857),
 .UNSPECIFIED.);
#768=B_SPLINE_CURVE_WITH_KNOTS('',3,(#46165,#46166,#46167,#46168,#46169,
#46170,#46171,#46172,#46173,#46174,#46175),.UNSPECIFIED.,.F.,.F.,(4,1,1,
1,1,1,1,1,4),(59.6902604182061,59.7371737325442,60.7311204006377,61.7250670687312,
62.7190137368247,63.7129604049182,64.7069070730116,65.7008537411051,65.9734457253857),
 .UNSPECIFIED.);
#769=B_SPLINE_CURVE_WITH_KNOTS('',3,(#46180,#46181,#46182,#46183,#46184,
#46185,#46186,#46187,#46188,#46189),.UNSPECIFIED.,.F.,.F.,(4,1,1,1,1,1,
1,4),(53.4070751110265,54.0987555652789,55.0927022333724,56.0866489014659,
57.0805955695594,58.0745422376529,59.0684889057464,59.6902604182061),
 .UNSPECIFIED.);
#770=B_SPLINE_CURVE_WITH_KNOTS('',3,(#46190,#46191,#46192,#46193,#46194,
#46195,#46196,#46197,#46198,#46199),.UNSPECIFIED.,.F.,.F.,(4,1,1,1,1,1,
1,4),(53.4070751110265,53.7734937239832,54.7674403920767,55.7613870601702,
56.7553337282637,57.7492803963572,58.7432270644507,59.6902604182061),
 .UNSPECIFIED.);
#771=B_SPLINE_CURVE_WITH_KNOTS('',3,(#46204,#46205,#46206,#46207,#46208,
#46209,#46210,#46211,#46212,#46213,#46214),.UNSPECIFIED.,.F.,.F.,(4,1,1,
1,1,1,1,1,4),(47.1238898038469,47.1411288886245,48.135075556718,49.1290222248115,
50.122968892905,51.1169155609985,52.1108622290919,53.1048088971854,53.4070751110265),
 .UNSPECIFIED.);
#772=B_SPLINE_CURVE_WITH_KNOTS('',3,(#46215,#46216,#46217,#46218,#46219,
#46220,#46221,#46222,#46223,#46224),.UNSPECIFIED.,.F.,.F.,(4,1,1,1,1,1,
1,4),(47.1238898038469,47.8098137154223,48.8037603835158,49.7977070516092,
50.7916537197027,51.7856003877962,52.7795470558897,53.4070751110265),
 .UNSPECIFIED.);
#773=B_SPLINE_CURVE_WITH_KNOTS('',3,(#46229,#46230,#46231,#46232,#46233,
#46234,#46235,#46236,#46237,#46238),.UNSPECIFIED.,.F.,.F.,(4,1,1,1,1,1,
1,4),(40.8407044966673,41.1774488800635,42.171395548157,43.1653422162505,
44.159288884344,45.1532355524375,46.147182220531,47.1238898038469),
 .UNSPECIFIED.);
#774=B_SPLINE_CURVE_WITH_KNOTS('',3,(#46239,#46240,#46241,#46242,#46243,
#46244,#46245,#46246,#46247,#46248,#46249),.UNSPECIFIED.,.F.,.F.,(4,1,1,
1,1,1,1,1,4),(40.8407044966673,40.8521870387678,41.8461337068613,42.8400803749548,
43.8340270430483,44.8279737111418,45.8219203792353,46.8158670473288,47.1238898038469),
 .UNSPECIFIED.);
#775=B_SPLINE_CURVE_WITH_KNOTS('',3,(#46254,#46255,#46256,#46257,#46258,
#46259,#46260,#46261,#46262,#46263),.UNSPECIFIED.,.F.,.F.,(4,1,1,1,1,1,
1,4),(34.5575191894877,35.2137688715026,36.2077155395961,37.2016622076895,
38.195608875783,39.1895555438765,40.18350221197,40.8407044966673),
 .UNSPECIFIED.);
#776=B_SPLINE_CURVE_WITH_KNOTS('',3,(#46264,#46265,#46266,#46267,#46268,
#46269,#46270,#46271,#46272,#46273),.UNSPECIFIED.,.F.,.F.,(4,1,1,1,1,1,
1,4),(34.5575191894877,34.8885070302068,35.8824536983003,36.8764003663938,
37.8703470344873,38.8642937025808,39.8582403706743,40.8407044966673),
 .UNSPECIFIED.);
#777=B_SPLINE_CURVE_WITH_KNOTS('',3,(#46278,#46279,#46280,#46281,#46282,
#46283,#46284,#46285,#46286,#46287),.UNSPECIFIED.,.F.,.F.,(4,1,1,1,1,1,
1,4),(28.2743338823081,29.2500888629416,30.2440355310351,31.2379821991286,
32.2319288672221,33.2258755353156,34.2198222034091,34.5575191894877),
 .UNSPECIFIED.);
#778=B_SPLINE_CURVE_WITH_KNOTS('',3,(#46288,#46289,#46290,#46291,#46292,
#46293,#46294,#46295,#46296,#46297),.UNSPECIFIED.,.F.,.F.,(4,1,1,1,1,1,
1,4),(28.2743338823081,28.9248270216459,29.9187736897394,30.9127203578329,
31.9066670259264,32.9006136940199,33.8945603621134,34.5575191894877),
 .UNSPECIFIED.);
#779=B_SPLINE_CURVE_WITH_KNOTS('',3,(#46302,#46303,#46304,#46305,#46306,
#46307,#46308,#46309,#46310,#46311,#46312),.UNSPECIFIED.,.F.,.F.,(4,1,1,
1,1,1,1,1,4),(21.9911485751285,22.2924621862871,23.2864088543806,24.2803555224741,
25.2743021905676,26.2682488586611,27.2621955267546,28.2561421948481,28.2743338823081),
 .UNSPECIFIED.);
#780=B_SPLINE_CURVE_WITH_KNOTS('',3,(#46313,#46314,#46315,#46316,#46317,
#46318,#46319,#46320,#46321,#46322),.UNSPECIFIED.,.F.,.F.,(4,1,1,1,1,1,
1,4),(21.9911485751285,22.9611470130849,23.9550936811784,24.9490403492719,
25.9429870173654,26.9369336854589,27.9308803535524,28.2743338823081),
 .UNSPECIFIED.);
#781=B_SPLINE_CURVE_WITH_KNOTS('',3,(#46329,#46330,#46331,#46332,#46333,
#46334,#46335,#46336,#46337),.UNSPECIFIED.,.F.,.F.,(4,1,1,1,1,1,4),(16.3287821777262,
17.3227288458197,18.3166755139132,19.3106221820067,20.3045688501002,21.2985155181937,
21.9911485751285),.UNSPECIFIED.);
#782=B_SPLINE_CURVE_WITH_KNOTS('',3,(#46338,#46339,#46340,#46341,#46342,
#46343,#46344,#46345,#46346,#46347,#46348),.UNSPECIFIED.,.F.,.F.,(4,1,1,
1,1,1,1,1,4),(15.707963267949,16.0035203364305,16.997467004524,17.9914136726175,
18.9853603407109,19.9793070088044,20.9732536768979,21.9672003449914,21.9911485751285),
 .UNSPECIFIED.);
#783=B_SPLINE_CURVE_WITH_KNOTS('',3,(#46351,#46352,#46353,#46354,#46355,
#46356,#46357,#46358,#46359,#46360,#46361,#46362,#46363,#46364,#46365,#46366,
#46367,#46368,#46369,#46370,#46371,#46372,#46373,#46374,#46375,#46376,#46377,
#46378,#46379,#46380,#46381,#46382,#46383,#46384,#46385,#46386,#46387,#46388,
#46389,#46390,#46391,#46392,#46393,#46394,#46395,#46396),.UNSPECIFIED.,
 .F.,.F.,(4,3,3,3,3,3,3,3,3,3,3,3,3,3,3,4),(-0.178587760439502,-0.17272415791405,
-0.159234259496745,-0.149955987523703,-0.138284796292971,-0.130233106211232,
-0.109899246057786,-0.100105179624859,-0.091716036524901,-0.0758685250126272,
-0.0664651298683787,-0.049848847401284,-0.0374767593822167,-0.0290667458166763,
-0.00650275602542257,0.),.UNSPECIFIED.);
#784=B_SPLINE_CURVE_WITH_KNOTS('',3,(#46401,#46402,#46403,#46404,#46405,
#46406,#46407,#46408,#46409,#46410,#46411,#46412,#46413,#46414,#46415,#46416,
#46417,#46418,#46419,#46420,#46421,#46422,#46423,#46424,#46425,#46426,#46427,
#46428,#46429,#46430,#46431,#46432,#46433,#46434,#46435,#46436,#46437,#46438,
#46439,#46440,#46441,#46442,#46443,#46444,#46445,#46446),.UNSPECIFIED.,
 .F.,.F.,(4,3,3,3,3,3,3,3,3,3,3,3,3,3,3,4),(-0.177567088092129,-0.170082240150724,
-0.15457601521052,-0.145395130014627,-0.128168571237308,-0.119335659531165,
-0.0984679221196259,-0.0877800536301027,-0.0797891990001937,-0.0653423149591641,
-0.0553291551848597,-0.0414968663886448,-0.0315265905887463,-0.02445163365906,
-0.00608210383285545,0.),.UNSPECIFIED.);
#785=B_SPLINE_CURVE_WITH_KNOTS('',3,(#47059,#47060,#47061,#47062,#47063,
#47064,#47065,#47066,#47067,#47068,#47069,#47070,#47071,#47072,#47073,#47074,
#47075,#47076,#47077,#47078,#47079,#47080),.UNSPECIFIED.,.F.,.F.,(4,3,3,
3,3,3,3,4),(140.91635969375,141.140426869276,142.13437353737,143.128320205463,
144.122266873557,145.11621354165,146.110160209744,147.026536188002),
 .UNSPECIFIED.);
#786=B_SPLINE_CURVE_WITH_KNOTS('',3,(#47082,#47083,#47084,#47085,#47086,
#47087,#47088,#47089,#47090,#47091,#47092,#47093,#47094,#47095,#47096,#47097,
#47098,#47099,#47100,#47101,#47102,#47103,#47104,#47105,#47106,#47107,#47108,
#47109,#47110,#47111,#47112,#47113,#47114,#47115,#47116,#47117,#47118,#47119,
#47120,#47121,#47122,#47123,#47124,#47125,#47126,#47127),.UNSPECIFIED.,
 .F.,.F.,(4,3,3,3,3,3,3,3,3,3,3,3,3,3,3,4),(-0.178587760439499,-0.172724157914047,
-0.159234256607848,-0.149955988339685,-0.138284793408456,-0.13023310313133,
-0.109899242927986,-0.100105179984139,-0.0917160365248915,-0.0758685219321002,
-0.0664651290585325,-0.0498488467938994,-0.0374767514336811,-0.0290667438409786,
-0.00650275235697207,0.),.UNSPECIFIED.);
#787=B_SPLINE_CURVE_WITH_KNOTS('',3,(#47128,#47129,#47130,#47131),
 .UNSPECIFIED.,.F.,.F.,(4,4),(15.0871443581717,15.707963267949),
 .UNSPECIFIED.);
#788=B_SPLINE_CURVE_WITH_KNOTS('',3,(#47133,#47134,#47135,#47136,#47137,
#47138,#47139,#47140,#47141,#47142,#47143,#47144,#47145,#47146,#47147,#47148,
#47149,#47150,#47151,#47152,#47153,#47154,#47155,#47156,#47157,#47158,#47159,
#47160,#47161,#47162,#47163,#47164,#47165,#47166,#47167,#47168,#47169,#47170,
#47171,#47172,#47173,#47174,#47175,#47176,#47177,#47178),.UNSPECIFIED.,
 .F.,.F.,(4,3,3,3,3,3,3,3,3,3,3,3,3,3,3,4),(-0.177567088092154,-0.170082240150739,
-0.154576013989902,-0.14539512805807,-0.12816855715706,-0.119335657029697,
-0.0984679168567635,-0.0877800538914335,-0.079789199000203,-0.0653423499049758,
-0.0553291540771241,-0.0414968655578431,-0.0315265899871487,-0.0244516335344751,
-0.00608210876879094,0.),.UNSPECIFIED.);
#789=B_SPLINE_CURVE_WITH_KNOTS('',3,(#47793,#47794,#47795,#47796,#47797,
#47798,#47799,#47800,#47801,#47802,#47803,#47804,#47805,#47806,#47807,#47808,
#47809,#47810,#47811),.UNSPECIFIED.,.F.,.F.,(4,3,3,3,3,3,4),(-149.092000214024,
-148.098053545931,-147.104106877837,-146.110160209743,-145.11621354165,
-144.122266873557,-143.892443155353),.UNSPECIFIED.);
#790=B_SPLINE_CURVE_WITH_KNOTS('',3,(#48675,#48676,#48677,#48678,#48679,
#48680,#48681,#48682,#48683,#48684,#48685,#48686,#48687,#48688,#48689,#48690),
 .UNSPECIFIED.,.F.,.F.,(4,3,3,3,3,4),(-6.1872247558925,-5.92766547213612,
-4.9397212267801,-3.95177698142408,-2.96383273606806,-2.06974660785395),
 .UNSPECIFIED.);
#791=B_SPLINE_CURVE_WITH_KNOTS('',3,(#48698,#48699,#48700,#48701,#48702,
#48703,#48704,#48705,#48706,#48707,#48708,#48709,#48710),.UNSPECIFIED.,
 .F.,.F.,(4,3,3,3,4),(0.,0.987944245356008,1.97588849071203,2.96383273606806,
3.21290471033757),.UNSPECIFIED.);
#792=B_SPLINE_CURVE_WITH_KNOTS('',3,(#48715,#48716,#48717,#48718,#48719,
#48720,#48721,#48722,#48723,#48724,#48725,#48726,#48727,#48728,#48729,#48730,
#48731,#48732,#48733,#48734,#48735,#48736),.UNSPECIFIED.,.F.,.F.,(4,3,3,
3,3,3,3,4),(-12.4704100630721,-11.8553309442722,-10.8673866989162,-9.8794424535602,
-8.89149820820418,-7.90355396284816,-6.91560971749214,-6.1872247558925),
 .UNSPECIFIED.);
#793=B_SPLINE_CURVE_WITH_KNOTS('',3,(#48737,#48738,#48739,#48740,#48741,
#48742,#48743,#48744,#48745,#48746,#48747,#48748,#48749,#48750,#48751,#48752,
#48753,#48754,#48755,#48756,#48757,#48758),.UNSPECIFIED.,.F.,.F.,(4,3,3,
3,3,3,3,4),(3.21290471033757,3.95177698142408,4.9397212267801,5.92766547213613,
6.91560971749214,7.90355396284817,8.89149820820418,9.49609001751715),
 .UNSPECIFIED.);
#794=B_SPLINE_CURVE_WITH_KNOTS('',3,(#48763,#48764,#48765,#48766,#48767,
#48768,#48769,#48770,#48771,#48772,#48773,#48774,#48775,#48776,#48777,#48778,
#48779,#48780,#48781,#48782,#48783,#48784),.UNSPECIFIED.,.F.,.F.,(4,3,3,
3,3,3,3,4),(-18.7535953702517,-17.7829964164084,-16.7950521710523,-15.8071079256963,
-14.8191636803403,-13.8312194349843,-12.8432751896283,-12.4704100630721),
 .UNSPECIFIED.);
#795=B_SPLINE_CURVE_WITH_KNOTS('',3,(#48785,#48786,#48787,#48788,#48789,
#48790,#48791,#48792,#48793,#48794,#48795,#48796,#48797,#48798,#48799,#48800,
#48801,#48802,#48803,#48804,#48805,#48806),.UNSPECIFIED.,.F.,.F.,(4,3,3,
3,3,3,3,4),(9.49609001751715,9.8794424535602,10.8673866989162,11.8553309442722,
12.8432751896283,13.8312194349843,14.8191636803403,15.7792753246967),
 .UNSPECIFIED.);
#796=B_SPLINE_CURVE_WITH_KNOTS('',3,(#48811,#48812,#48813,#48814,#48815,
#48816,#48817,#48818,#48819,#48820,#48821,#48822,#48823,#48824,#48825,#48826,
#48827,#48828,#48829,#48830,#48831,#48832,#48833,#48834,#48835),
 .UNSPECIFIED.,.F.,.F.,(4,3,3,3,3,3,3,3,4),(-25.0367806774313,-24.6986061339005,
-23.7106618885445,-22.7227176431885,-21.7347733978324,-20.7468291524764,
-19.7588849071204,-18.7709406617644,-18.7535953702517),.UNSPECIFIED.);
#797=B_SPLINE_CURVE_WITH_KNOTS('',3,(#48836,#48837,#48838,#48839,#48840,
#48841,#48842,#48843,#48844,#48845,#48846,#48847,#48848,#48849,#48850,#48851,
#48852,#48853,#48854,#48855,#48856,#48857,#48858,#48859,#48860),
 .UNSPECIFIED.,.F.,.F.,(4,3,3,3,3,3,3,3,4),(15.7792753246967,15.8071079256963,
16.7950521710523,17.7829964164084,18.7709406617644,19.7588849071204,20.7468291524764,
21.7347733978324,22.0624606318763),.UNSPECIFIED.);
#798=B_SPLINE_CURVE_WITH_KNOTS('',3,(#48865,#48866,#48867,#48868,#48869,
#48870,#48871,#48872,#48873,#48874,#48875,#48876,#48877,#48878,#48879,#48880,
#48881,#48882,#48883,#48884,#48885,#48886),.UNSPECIFIED.,.F.,.F.,(4,3,3,
3,3,3,3,4),(-31.3199659846109,-30.6262716060366,-29.6383273606806,-28.6503831153246,
-27.6624388699686,-26.6744946246125,-25.6865503792565,-25.0367806774313),
 .UNSPECIFIED.);
#799=B_SPLINE_CURVE_WITH_KNOTS('',3,(#48887,#48888,#48889,#48890,#48891,
#48892,#48893,#48894,#48895,#48896,#48897,#48898,#48899,#48900,#48901,#48902,
#48903,#48904,#48905,#48906,#48907,#48908),.UNSPECIFIED.,.F.,.F.,(4,3,3,
3,3,3,3,4),(22.0624606318763,22.7227176431885,23.7106618885445,24.6986061339005,
25.6865503792565,26.6744946246125,27.6624388699686,28.3456459390559),
 .UNSPECIFIED.);
#800=B_SPLINE_CURVE_WITH_KNOTS('',3,(#48913,#48914,#48915,#48916,#48917,
#48918,#48919,#48920,#48921,#48922,#48923,#48924,#48925,#48926,#48927,#48928,
#48929,#48930,#48931,#48932,#48933,#48934,#48935,#48936,#48937),
 .UNSPECIFIED.,.F.,.F.,(4,3,3,3,3,3,3,3,4),(-37.6031512917904,-37.5418813235288,
-36.5539370781727,-35.5659928328167,-34.5780485874607,-33.5901043421047,
-32.6021600967487,-31.6142158513926,-31.3199659846109),.UNSPECIFIED.);
#801=B_SPLINE_CURVE_WITH_KNOTS('',3,(#48938,#48939,#48940,#48941,#48942,
#48943,#48944,#48945,#48946,#48947,#48948,#48949,#48950,#48951,#48952,#48953,
#48954,#48955,#48956,#48957,#48958,#48959,#48960,#48961,#48962),
 .UNSPECIFIED.,.F.,.F.,(4,3,3,3,3,3,3,3,4),(28.3456459390559,28.6503831153246,
29.6383273606806,30.6262716060366,31.6142158513926,32.6021600967487,33.5901043421047,
34.5780485874607,34.6288312462355),.UNSPECIFIED.);
#802=B_SPLINE_CURVE_WITH_KNOTS('',3,(#48967,#48968,#48969,#48970,#48971,
#48972,#48973,#48974,#48975,#48976,#48977,#48978,#48979,#48980,#48981,#48982,
#48983,#48984,#48985,#48986,#48987,#48988),.UNSPECIFIED.,.F.,.F.,(4,3,3,
3,3,3,3,4),(-43.88633659897,-43.4695467956649,-42.4816025503089,-41.4936583049528,
-40.5057140595968,-39.5177698142408,-38.5298255688848,-37.6031512917904),
 .UNSPECIFIED.);
#803=B_SPLINE_CURVE_WITH_KNOTS('',3,(#48989,#48990,#48991,#48992,#48993,
#48994,#48995,#48996,#48997,#48998,#48999,#49000,#49001,#49002,#49003,#49004,
#49005,#49006,#49007,#49008,#49009,#49010),.UNSPECIFIED.,.F.,.F.,(4,3,3,
3,3,3,3,4),(34.6288312462355,35.5659928328167,36.5539370781727,37.5418813235288,
38.5298255688848,39.5177698142408,40.5057140595968,40.9120165534151),
 .UNSPECIFIED.);
#804=B_SPLINE_CURVE_WITH_KNOTS('',3,(#49015,#49016,#49017,#49018,#49019,
#49020,#49021,#49022,#49023,#49024,#49025,#49026,#49027,#49028,#49029,#49030,
#49031,#49032,#49033,#49034,#49035,#49036),.UNSPECIFIED.,.F.,.F.,(4,3,3,
3,3,3,3,4),(-50.1695219061496,-49.397212267801,-48.409268022445,-47.421323777089,
-46.4333795317329,-45.4454352863769,-44.4574910410209,-43.88633659897),
 .UNSPECIFIED.);
#805=B_SPLINE_CURVE_WITH_KNOTS('',3,(#49037,#49038,#49039,#49040,#49041,
#49042,#49043,#49044,#49045,#49046,#49047,#49048,#49049,#49050,#49051,#49052,
#49053,#49054,#49055,#49056,#49057,#49058),.UNSPECIFIED.,.F.,.F.,(4,3,3,
3,3,3,3,4),(40.9120165534151,41.4936583049528,42.4816025503089,43.4695467956649,
44.4574910410209,45.4454352863769,46.4333795317329,47.1952018605947),
 .UNSPECIFIED.);
#806=B_SPLINE_CURVE_WITH_KNOTS('',3,(#49063,#49064,#49065,#49066,#49067,
#49068,#49069,#49070,#49071,#49072,#49073,#49074,#49075,#49076,#49077,#49078,
#49079,#49080,#49081,#49082,#49083,#49084,#49085,#49086,#49087),
 .UNSPECIFIED.,.F.,.F.,(4,3,3,3,3,3,3,3,4),(-56.4527072133292,-56.3128219852932,
-55.3248777399371,-54.3369334945811,-53.3489892492251,-52.3610450038691,
-51.373100758513,-50.385156513157,-50.1695219061496),.UNSPECIFIED.);
#807=B_SPLINE_CURVE_WITH_KNOTS('',3,(#49088,#49089,#49090,#49091,#49092,
#49093,#49094,#49095,#49096,#49097,#49098,#49099,#49100,#49101,#49102,#49103,
#49104,#49105,#49106,#49107,#49108,#49109,#49110,#49111,#49112),
 .UNSPECIFIED.,.F.,.F.,(4,3,3,3,3,3,3,3,4),(47.1952018605947,47.421323777089,
48.409268022445,49.397212267801,50.385156513157,51.373100758513,52.3610450038691,
53.3489892492251,53.4783871677743),.UNSPECIFIED.);
#808=B_SPLINE_CURVE_WITH_KNOTS('',3,(#49117,#49118,#49119,#49120,#49121,
#49122,#49123,#49124,#49125,#49126,#49127,#49128,#49129,#49130,#49131,#49132,
#49133,#49134,#49135,#49136,#49137,#49138),.UNSPECIFIED.,.F.,.F.,(4,3,3,
3,3,3,3,4),(-62.7358925205088,-62.2404874574293,-61.2525432120733,-60.2645989667172,
-59.2766547213612,-58.2887104760052,-57.3007662306492,-56.4527072133292),
 .UNSPECIFIED.);
#809=B_SPLINE_CURVE_WITH_KNOTS('',3,(#49139,#49140,#49141,#49142,#49143,
#49144,#49145,#49146,#49147,#49148,#49149,#49150,#49151,#49152,#49153,#49154,
#49155,#49156,#49157,#49158,#49159,#49160),.UNSPECIFIED.,.F.,.F.,(4,3,3,
3,3,3,3,4),(53.4783871677743,54.3369334945811,55.3248777399371,56.3128219852931,
57.3007662306492,58.2887104760052,59.2766547213612,59.7615724749539),
 .UNSPECIFIED.);
#810=B_SPLINE_CURVE_WITH_KNOTS('',3,(#49165,#49166,#49167,#49168,#49169,
#49170,#49171,#49172,#49173,#49174,#49175,#49176,#49177,#49178,#49179,#49180,
#49181,#49182,#49183,#49184,#49185,#49186),.UNSPECIFIED.,.F.,.F.,(4,3,3,
3,3,3,3,4),(-69.0190778276884,-68.1681529295654,-67.1802086842094,-66.1922644388533,
-65.2043201934973,-64.2163759481413,-63.2284317027853,-62.7358925205088),
 .UNSPECIFIED.);
#811=B_SPLINE_CURVE_WITH_KNOTS('',3,(#49187,#49188,#49189,#49190,#49191,
#49192,#49193,#49194,#49195,#49196,#49197,#49198,#49199,#49200,#49201,#49202,
#49203,#49204,#49205,#49206,#49207,#49208),.UNSPECIFIED.,.F.,.F.,(4,3,3,
3,3,3,3,4),(59.7615724749539,60.2645989667172,61.2525432120732,62.2404874574293,
63.2284317027853,64.2163759481413,65.2043201934973,66.0447577821335),
 .UNSPECIFIED.);
#812=B_SPLINE_CURVE_WITH_KNOTS('',3,(#49213,#49214,#49215,#49216,#49217,
#49218,#49219,#49220,#49221,#49222,#49223,#49224,#49225,#49226,#49227,#49228,
#49229,#49230,#49231,#49232,#49233,#49234,#49235,#49236,#49237),
 .UNSPECIFIED.,.F.,.F.,(4,3,3,3,3,3,3,3,4),(-75.302263134868,-75.0837626470575,
-74.0958184017015,-73.1078741563455,-72.1199299109895,-71.1319856656335,
-70.1440414202774,-69.1560971749214,-69.0190778276884),.UNSPECIFIED.);
#813=B_SPLINE_CURVE_WITH_KNOTS('',3,(#49238,#49239,#49240,#49241,#49242,
#49243,#49244,#49245,#49246,#49247,#49248,#49249,#49250,#49251,#49252,#49253,
#49254,#49255,#49256,#49257,#49258,#49259,#49260,#49261,#49262),
 .UNSPECIFIED.,.F.,.F.,(4,3,3,3,3,3,3,3,4),(66.0447577821335,66.1922644388533,
67.1802086842094,68.1681529295654,69.1560971749214,70.1440414202774,71.1319856656334,
72.1199299109894,72.3279430893131),.UNSPECIFIED.);
#814=B_SPLINE_CURVE_WITH_KNOTS('',3,(#49268,#49269,#49270,#49271,#49272,
#49273,#49274,#49275,#49276),.UNSPECIFIED.,.F.,.F.,(4,1,1,1,1,1,4),(84.8230016469244,
84.9600209941574,85.9479652395134,86.9359094848694,87.9238537302254,88.9117979755815,
89.8058841037956),.UNSPECIFIED.);
#815=B_SPLINE_CURVE_WITH_KNOTS('',3,(#49279,#49280,#49281,#49282,#49283,
#49284,#49285),.UNSPECIFIED.,.F.,.F.,(4,1,1,1,4),(84.8230016469244,85.6029327139567,
86.5908769593128,87.5788212046688,88.5667654500248),.UNSPECIFIED.);
#816=B_SPLINE_CURVE_WITH_KNOTS('',3,(#49290,#49291,#49292,#49293,#49294,
#49295,#49296,#49297,#49298,#49299),.UNSPECIFIED.,.F.,.F.,(4,1,1,1,1,1,
1,4),(78.5398163397448,79.0323555220213,80.0202997673773,81.0082440127333,
81.9961882580893,82.9841325034453,83.9720767488014,84.8230016469244),
 .UNSPECIFIED.);
#817=B_SPLINE_CURVE_WITH_KNOTS('',3,(#49300,#49301,#49302,#49303,#49304,
#49305,#49306,#49307,#49308,#49309,#49310),.UNSPECIFIED.,.F.,.F.,(4,1,1,
1,1,1,1,1,4),(78.5398163397448,78.6873229964646,79.6752672418206,80.6632114871766,
81.6511557325327,82.6390999778887,83.6270442232447,84.6149884686007,84.8230016469244),
 .UNSPECIFIED.);
#818=B_SPLINE_CURVE_WITH_KNOTS('',3,(#49315,#49316,#49317,#49318,#49319,
#49320,#49321,#49322,#49323,#49324),.UNSPECIFIED.,.F.,.F.,(4,1,1,1,1,1,
1,4),(72.2566310325652,73.1046900498851,74.0926342952412,75.0805785405972,
76.0685227859532,77.0564670313092,78.0444112766652,78.5398163397448),
 .UNSPECIFIED.);
#819=B_SPLINE_CURVE_WITH_KNOTS('',3,(#49325,#49326,#49327,#49328,#49329,
#49330,#49331,#49332,#49333,#49334),.UNSPECIFIED.,.F.,.F.,(4,1,1,1,1,1,
1,4),(72.2566310325652,72.7596575243285,73.7476017696845,74.7355460150405,
75.7234902603965,76.7114345057526,77.6993787511086,78.5398163397448),
 .UNSPECIFIED.);
#820=B_SPLINE_CURVE_WITH_KNOTS('',3,(#49339,#49340,#49341,#49342,#49343,
#49344,#49345,#49346,#49347,#49348,#49349),.UNSPECIFIED.,.F.,.F.,(4,1,1,
1,1,1,1,1,4),(65.9734457253856,66.189080332393,67.177024577749,68.164968823105,
69.1529130684611,70.1408573138171,71.1288015591731,72.1167458045291,72.2566310325652),
 .UNSPECIFIED.);
#821=B_SPLINE_CURVE_WITH_KNOTS('',3,(#49350,#49351,#49352,#49353,#49354,
#49355,#49356,#49357,#49358,#49359),.UNSPECIFIED.,.F.,.F.,(4,1,1,1,1,1,
1,4),(65.9734457253856,66.8319920521924,67.8199362975484,68.8078805429044,
69.7958247882604,70.7837690336165,71.7717132789725,72.2566310325652),
 .UNSPECIFIED.);
#822=B_SPLINE_CURVE_WITH_KNOTS('',3,(#49364,#49365,#49366,#49367,#49368,
#49369,#49370,#49371,#49372,#49373),.UNSPECIFIED.,.F.,.F.,(4,1,1,1,1,1,
1,4),(59.6902604182061,60.2614148602569,61.2493591056129,62.2373033509689,
63.2252475963249,64.213191841681,65.201136087037,65.9734457253856),
 .UNSPECIFIED.);
#823=B_SPLINE_CURVE_WITH_KNOTS('',3,(#49374,#49375,#49376,#49377,#49378,
#49379,#49380,#49381,#49382,#49383,#49384),.UNSPECIFIED.,.F.,.F.,(4,1,1,
1,1,1,1,1,4),(59.690260418206,59.9163823347002,60.9043265800563,61.8922708254123,
62.8802150707683,63.8681593161243,64.8561035614803,65.8440478068363,65.9734457253856),
 .UNSPECIFIED.);
#824=B_SPLINE_CURVE_WITH_KNOTS('',3,(#49389,#49390,#49391,#49392,#49393,
#49394,#49395,#49396,#49397,#49398),.UNSPECIFIED.,.F.,.F.,(4,1,1,1,1,1,
1,4),(53.4070751110265,54.3337493881208,55.3216936334768,56.3096378788328,
57.2975821241888,58.2855263695448,59.2734706149009,59.6902604182061),
 .UNSPECIFIED.);
#825=B_SPLINE_CURVE_WITH_KNOTS('',3,(#49399,#49400,#49401,#49402,#49403,
#49404,#49405,#49406,#49407,#49408),.UNSPECIFIED.,.F.,.F.,(4,1,1,1,1,1,
1,4),(53.4070751110264,53.9887168625641,54.9766611079201,55.9646053532762,
56.9525495986322,57.9404938439882,58.9284380893442,59.690260418206),
 .UNSPECIFIED.);
#826=B_SPLINE_CURVE_WITH_KNOTS('',3,(#49413,#49414,#49415,#49416,#49417,
#49418,#49419,#49420,#49421,#49422,#49423),.UNSPECIFIED.,.F.,.F.,(4,1,1,
1,1,1,1,1,4),(47.1238898038469,47.4181396706286,48.4060839159846,49.3940281613407,
50.3819724066967,51.3699166520527,52.3578608974087,53.3458051427647,53.4070751110265),
 .UNSPECIFIED.);
#827=B_SPLINE_CURVE_WITH_KNOTS('',3,(#49424,#49425,#49426,#49427,#49428,
#49429,#49430,#49431,#49432,#49433),.UNSPECIFIED.,.F.,.F.,(4,1,1,1,1,1,
1,4),(47.1238898038469,48.061051390428,49.048995635784,50.03693988114,51.0248841264961,
52.0128283718521,53.0007726172081,53.4070751110264),.UNSPECIFIED.);
#828=B_SPLINE_CURVE_WITH_KNOTS('',3,(#49438,#49439,#49440,#49441,#49442,
#49443,#49444,#49445,#49446,#49447),.UNSPECIFIED.,.F.,.F.,(4,1,1,1,1,1,
1,4),(40.8407044966673,41.4904741984925,42.4784184438485,43.4663626892045,
44.4543069345606,45.4422511799166,46.4301954252726,47.1238898038469),
 .UNSPECIFIED.);
#829=B_SPLINE_CURVE_WITH_KNOTS('',3,(#49448,#49449,#49450,#49451,#49452,
#49453,#49454,#49455,#49456,#49457,#49458),.UNSPECIFIED.,.F.,.F.,(4,1,1,
1,1,1,1,1,4),(40.8407044966673,41.1454416729359,42.1333859182919,43.1213301636479,
44.1092744090039,45.0972186543599,46.085162899716,47.073107145072,47.1238898038469),
 .UNSPECIFIED.);
#830=B_SPLINE_CURVE_WITH_KNOTS('',3,(#49463,#49464,#49465,#49466,#49467,
#49468,#49469,#49470,#49471,#49472,#49473),.UNSPECIFIED.,.F.,.F.,(4,1,1,
1,1,1,1,1,4),(34.5575191894877,34.5748644810004,35.5628087263564,36.5507529717124,
37.5386972170684,38.5266414624244,39.5145857077805,40.5025299531365,40.8407044966673),
 .UNSPECIFIED.);
#831=B_SPLINE_CURVE_WITH_KNOTS('',3,(#49474,#49475,#49476,#49477,#49478,
#49479,#49480,#49481,#49482,#49483),.UNSPECIFIED.,.F.,.F.,(4,1,1,1,1,1,
1,4),(34.5575191894877,35.2177762007997,36.2057204461558,37.1936646915118,
38.1816089368678,39.1695531822238,40.1574974275798,40.8407044966673),
 .UNSPECIFIED.);
#832=B_SPLINE_CURVE_WITH_KNOTS('',3,(#49488,#49489,#49490,#49491,#49492,
#49493,#49494,#49495,#49496,#49497),.UNSPECIFIED.,.F.,.F.,(4,1,1,1,1,1,
1,4),(28.2743338823081,28.6471990088642,29.6351432542203,30.6230874995763,
31.6110317449323,32.5989759902883,33.5869202356443,34.5575191894877),
 .UNSPECIFIED.);
#833=B_SPLINE_CURVE_WITH_KNOTS('',3,(#49498,#49499,#49500,#49501,#49502,
#49503,#49504,#49505,#49506,#49507,#49508),.UNSPECIFIED.,.F.,.F.,(4,1,1,
1,1,1,1,1,4),(28.2743338823081,28.3021664833076,29.2901107286636,30.2780549740196,
31.2659992193757,32.2539434647317,33.2418877100877,34.2298319554437,34.5575191894877),
 .UNSPECIFIED.);
#834=B_SPLINE_CURVE_WITH_KNOTS('',3,(#49513,#49514,#49515,#49516,#49517,
#49518,#49519,#49520,#49521,#49522),.UNSPECIFIED.,.F.,.F.,(4,1,1,1,1,1,
1,4),(21.9911485751285,22.7195335367281,23.7074777820841,24.6954220274402,
25.6833662727962,26.6713105181522,27.6592547635082,28.2743338823081),
 .UNSPECIFIED.);
#835=B_SPLINE_CURVE_WITH_KNOTS('',3,(#49523,#49524,#49525,#49526,#49527,
#49528,#49529,#49530,#49531,#49532),.UNSPECIFIED.,.F.,.F.,(4,1,1,1,1,1,
1,4),(21.9911485751285,22.3745010111715,23.3624452565275,24.3503895018835,
25.3383337472395,26.3262779925956,27.3142222379516,28.2743338823081),
 .UNSPECIFIED.);
#836=B_SPLINE_CURVE_WITH_KNOTS('',3,(#49539,#49540,#49541,#49542,#49543,
#49544,#49545,#49546,#49547,#49548),.UNSPECIFIED.,.F.,.F.,(4,1,1,1,1,1,
1,4),(15.803923819236,16.791868064592,17.779812309948,18.767756555304,19.7557008006601,
20.7436450460161,21.7315892913721,21.9911485751285),.UNSPECIFIED.);
#837=B_SPLINE_CURVE_WITH_KNOTS('',3,(#49549,#49550,#49551,#49552,#49553,
#49554,#49555,#49556,#49557,#49558),.UNSPECIFIED.,.F.,.F.,(4,1,1,1,1,1,
1,4),(15.7079632679489,16.4468355390354,17.4347797843914,18.4227240297474,
19.4106682751034,20.3986125204594,21.3865567658155,21.9911485751285),
 .UNSPECIFIED.);
#838=B_SPLINE_CURVE_WITH_KNOTS('',3,(#49561,#49562,#49563,#49564,#49565,
#49566,#49567,#49568,#49569,#49570,#49571,#49572,#49573,#49574,#49575,#49576,
#49577,#49578,#49579,#49580,#49581,#49582,#49583,#49584,#49585,#49586,#49587,
#49588,#49589,#49590,#49591,#49592,#49593,#49594,#49595,#49596,#49597,#49598,
#49599,#49600,#49601,#49602,#49603,#49604,#49605,#49606,#49607,#49608,#49609),
 .UNSPECIFIED.,.F.,.F.,(4,3,3,3,3,3,3,3,3,3,3,3,3,3,3,3,4),(-0.227523845437324,
-0.218350149341661,-0.205842204254971,-0.194305484443851,-0.180954054603224,
-0.167897350901462,-0.143373661203175,-0.133616778871748,-0.125537010422148,
-0.115138897237553,-0.0973810329882545,-0.0847723556366763,-0.0635792667275072,
-0.0502539163266662,-0.0410435569307654,-0.0141179092232515,0.),
 .UNSPECIFIED.);
#839=B_SPLINE_CURVE_WITH_KNOTS('',3,(#49614,#49615,#49616,#49617,#49618,
#49619,#49620,#49621,#49622,#49623,#49624,#49625,#49626,#49627,#49628,#49629,
#49630,#49631,#49632,#49633,#49634,#49635,#49636,#49637,#49638,#49639,#49640,
#49641,#49642,#49643,#49644,#49645,#49646,#49647,#49648,#49649,#49650,#49651,
#49652,#49653,#49654,#49655,#49656,#49657,#49658,#49659,#49660,#49661,#49662),
 .UNSPECIFIED.,.F.,.F.,(4,3,3,3,3,3,3,3,3,3,3,3,3,3,3,3,4),(-0.226379821609596,
-0.215007753384842,-0.195255307837548,-0.183767362539732,-0.169423470115966,
-0.156758753808324,-0.131327701983312,-0.121202735143442,-0.113669834739438,
-0.101656477907397,-0.0859751299016101,-0.0772104628791785,-0.0531806453069207,
-0.0418075009839797,-0.032303590237005,-0.00987926401158647,0.),
 .UNSPECIFIED.);
#840=B_SPLINE_CURVE_WITH_KNOTS('',3,(#49983,#49984,#49985,#49986,#49987,
#49988,#49989),.UNSPECIFIED.,.F.,.F.,(4,3,4),(72.3279430893131,73.1078741563455,
74.0019602845596),.UNSPECIFIED.);
#841=B_SPLINE_CURVE_WITH_KNOTS('',3,(#49991,#49992,#49993,#49994,#49995,
#49996,#49997,#49998,#49999,#50000,#50001,#50002,#50003,#50004,#50005,#50006,
#50007,#50008,#50009,#50010,#50011,#50012,#50013,#50014,#50015,#50016,#50017,
#50018,#50019,#50020,#50021,#50022,#50023,#50024,#50025,#50026,#50027,#50028,
#50029,#50030,#50031,#50032,#50033,#50034,#50035,#50036,#50037,#50038,#50039),
 .UNSPECIFIED.,.F.,.F.,(4,3,3,3,3,3,3,3,3,3,3,3,3,3,3,3,4),(-0.227523845437316,
-0.218350149341655,-0.205842197866321,-0.194305484374478,-0.180954006819641,
-0.167897358466276,-0.143373669279798,-0.133616834209574,-0.125537019650691,
-0.115138897237547,-0.097381026810668,-0.0847723567113073,-0.0635792675334805,
-0.0502539177590211,-0.0410435559730182,-0.0141179048973905,0.),
 .UNSPECIFIED.);
#842=B_SPLINE_CURVE_WITH_KNOTS('',3,(#50040,#50041,#50042,#50043,#50044),
 .UNSPECIFIED.,.F.,.F.,(4,1,4),(14.5648051654652,15.4588912936793,15.7079632679489),
 .UNSPECIFIED.);
#843=B_SPLINE_CURVE_WITH_KNOTS('',3,(#50046,#50047,#50048,#50049,#50050,
#50051,#50052,#50053,#50054,#50055,#50056,#50057,#50058,#50059,#50060,#50061,
#50062,#50063,#50064,#50065,#50066,#50067,#50068,#50069,#50070,#50071,#50072,
#50073,#50074,#50075,#50076,#50077,#50078,#50079,#50080,#50081,#50082,#50083,
#50084,#50085,#50086,#50087,#50088,#50089,#50090,#50091,#50092,#50093,#50094),
 .UNSPECIFIED.,.F.,.F.,(4,3,3,3,3,3,3,3,3,3,3,3,3,3,3,3,4),(-0.226379821609599,
-0.215007753384844,-0.19525530446945,-0.183767359662995,-0.169423451536204,
-0.156758753435164,-0.131327696656529,-0.121202706406611,-0.113669787610754,
-0.101656477907395,-0.0859751252241449,-0.077210461042814,-0.0531806474590482,
-0.0418075086540048,-0.032303593576968,-0.00987927928781002,0.),
 .UNSPECIFIED.);
#844=B_SPLINE_CURVE_WITH_KNOTS('',3,(#50417,#50418,#50419,#50420),
 .UNSPECIFIED.,.F.,.F.,(4,4),(-76.0717068924135,-75.302263134868),
 .UNSPECIFIED.);
#845=B_SPLINE_CURVE_WITH_KNOTS('',3,(#51284,#51285,#51286,#51287,#51288,
#51289,#51290,#51291,#51292,#51293,#51294,#51295,#51296,#51297,#51298,#51299),
 .UNSPECIFIED.,.F.,.F.,(4,3,3,3,3,4),(-6.2359038847334,-5.98672898897424,
-4.9889408241452,-3.99115265931616,-2.99336449448712,-2.07291355912483),
 .UNSPECIFIED.);
#846=B_SPLINE_CURVE_WITH_KNOTS('',3,(#51307,#51308,#51309,#51310,#51311,
#51312,#51313,#51314,#51315,#51316,#51317,#51318,#51319),.UNSPECIFIED.,
 .F.,.F.,(4,3,3,3,4),(0.,0.997788164829036,1.99557632965808,2.99336449448712,
3.26014431587357),.UNSPECIFIED.);
#847=B_SPLINE_CURVE_WITH_KNOTS('',3,(#51324,#51325,#51326,#51327,#51328,
#51329,#51330,#51331,#51332,#51333,#51334,#51335,#51336,#51337,#51338,#51339,
#51340,#51341,#51342,#51343,#51344,#51345),.UNSPECIFIED.,.F.,.F.,(4,3,3,
3,3,3,3,4),(-12.519089191913,-11.9734579779485,-10.9756698131195,-9.97788164829041,
-8.98009348346137,-7.98230531863233,-6.98451715380329,-6.2359038847334),
 .UNSPECIFIED.);
#848=B_SPLINE_CURVE_WITH_KNOTS('',3,(#51346,#51347,#51348,#51349,#51350,
#51351,#51352,#51353,#51354,#51355,#51356,#51357,#51358,#51359,#51360,#51361,
#51362,#51363,#51364,#51365,#51366,#51367),.UNSPECIFIED.,.F.,.F.,(4,3,3,
3,3,3,3,4),(3.26014431587357,3.99115265931617,4.9889408241452,5.98672898897425,
6.98451715380329,7.98230531863232,8.98009348346137,9.54332962305316),
 .UNSPECIFIED.);
#849=B_SPLINE_CURVE_WITH_KNOTS('',3,(#51372,#51373,#51374,#51375,#51376,
#51377,#51378,#51379,#51380,#51381,#51382,#51383,#51384,#51385,#51386,#51387,
#51388,#51389,#51390,#51391,#51392,#51393),.UNSPECIFIED.,.F.,.F.,(4,3,3,
3,3,3,3,4),(-18.8022744990926,-17.9601869669227,-16.9623988020937,-15.9646106372647,
-14.9668224724356,-13.9690343076066,-12.9712461427775,-12.519089191913),
 .UNSPECIFIED.);
#850=B_SPLINE_CURVE_WITH_KNOTS('',3,(#51394,#51395,#51396,#51397,#51398,
#51399,#51400,#51401,#51402,#51403,#51404,#51405,#51406,#51407,#51408,#51409,
#51410,#51411,#51412,#51413,#51414,#51415),.UNSPECIFIED.,.F.,.F.,(4,3,3,
3,3,3,3,4),(9.54332962305316,9.97788164829041,10.9756698131194,11.9734579779485,
12.9712461427775,13.9690343076066,14.9668224724356,15.8265149302327),
 .UNSPECIFIED.);
#851=B_SPLINE_CURVE_WITH_KNOTS('',3,(#51420,#51421,#51422,#51423,#51424,
#51425,#51426,#51427,#51428,#51429,#51430,#51431,#51432,#51433,#51434,#51435,
#51436,#51437,#51438,#51439,#51440,#51441,#51442,#51443,#51444),
 .UNSPECIFIED.,.F.,.F.,(4,3,3,3,3,3,3,3,4),(-25.0854598062722,-24.944704120726,
-23.946915955897,-22.9491277910679,-21.9513396262389,-20.9535514614099,
-19.9557632965808,-18.9579751317518,-18.8022744990926),.UNSPECIFIED.);
#852=B_SPLINE_CURVE_WITH_KNOTS('',3,(#51445,#51446,#51447,#51448,#51449,
#51450,#51451,#51452,#51453,#51454,#51455,#51456,#51457,#51458,#51459,#51460,
#51461,#51462,#51463,#51464,#51465,#51466,#51467,#51468,#51469),
 .UNSPECIFIED.,.F.,.F.,(4,3,3,3,3,3,3,3,4),(15.8265149302327,15.9646106372647,
16.9623988020937,17.9601869669227,18.9579751317518,19.9557632965808,20.9535514614099,
21.9513396262389,22.1097002374123),.UNSPECIFIED.);
#853=B_SPLINE_CURVE_WITH_KNOTS('',3,(#51474,#51475,#51476,#51477,#51478,
#51479,#51480,#51481,#51482,#51483,#51484,#51485,#51486,#51487,#51488,#51489,
#51490,#51491,#51492,#51493,#51494,#51495),.UNSPECIFIED.,.F.,.F.,(4,3,3,
3,3,3,3,4),(-31.3686451134517,-30.9314331097003,-29.9336449448712,-28.9358567800422,
-27.9380686152131,-26.9402804503841,-25.9424922855551,-25.0854598062722),
 .UNSPECIFIED.);
#854=B_SPLINE_CURVE_WITH_KNOTS('',3,(#51496,#51497,#51498,#51499,#51500,
#51501,#51502,#51503,#51504,#51505,#51506,#51507,#51508,#51509,#51510,#51511,
#51512,#51513,#51514,#51515,#51516,#51517),.UNSPECIFIED.,.F.,.F.,(4,3,3,
3,3,3,3,4),(22.1097002374123,22.9491277910679,23.946915955897,24.944704120726,
25.9424922855551,26.9402804503841,27.9380686152131,28.3928855445919),
 .UNSPECIFIED.);
#855=B_SPLINE_CURVE_WITH_KNOTS('',3,(#51522,#51523,#51524,#51525,#51526,
#51527,#51528,#51529,#51530,#51531,#51532,#51533,#51534,#51535,#51536,#51537,
#51538,#51539,#51540,#51541,#51542,#51543),.UNSPECIFIED.,.F.,.F.,(4,3,3,
3,3,3,3,4),(-37.6518304206313,-36.9181620986745,-35.9203739338455,-34.9225857690164,
-33.9247976041874,-32.9270094393584,-31.9292212745293,-31.3686451134517),
 .UNSPECIFIED.);
#856=B_SPLINE_CURVE_WITH_KNOTS('',3,(#51544,#51545,#51546,#51547,#51548,
#51549,#51550,#51551,#51552,#51553,#51554,#51555,#51556,#51557,#51558,#51559,
#51560,#51561,#51562,#51563,#51564,#51565),.UNSPECIFIED.,.F.,.F.,(4,3,3,
3,3,3,3,4),(28.3928855445919,28.9358567800422,29.9336449448712,30.9314331097003,
31.9292212745293,32.9270094393584,33.9247976041874,34.6760708517715),
 .UNSPECIFIED.);
#857=B_SPLINE_CURVE_WITH_KNOTS('',3,(#51570,#51571,#51572,#51573,#51574,
#51575,#51576,#51577,#51578,#51579,#51580,#51581,#51582,#51583,#51584,#51585,
#51586,#51587,#51588,#51589,#51590,#51591,#51592,#51593,#51594),
 .UNSPECIFIED.,.F.,.F.,(4,3,3,3,3,3,3,3,4),(-43.9350157278109,-43.9026792524778,
-42.9048910876488,-41.9071029228197,-40.9093147579907,-39.9115265931616,
-38.9137384283326,-37.9159502635036,-37.6518304206313),.UNSPECIFIED.);
#858=B_SPLINE_CURVE_WITH_KNOTS('',3,(#51595,#51596,#51597,#51598,#51599,
#51600,#51601,#51602,#51603,#51604,#51605,#51606,#51607,#51608,#51609,#51610,
#51611,#51612,#51613,#51614,#51615,#51616,#51617,#51618,#51619),
 .UNSPECIFIED.,.F.,.F.,(4,3,3,3,3,3,3,3,4),(34.6760708517715,34.9225857690164,
35.9203739338455,36.9181620986745,37.9159502635036,38.9137384283326,39.9115265931616,
40.9093147579907,40.9592561589511),.UNSPECIFIED.);
#859=B_SPLINE_CURVE_WITH_KNOTS('',3,(#51625,#51626,#51627,#51628,#51629,
#51630),.UNSPECIFIED.,.F.,.F.,(4,1,1,4),(59.6902604182061,60.655712107702,
61.653500272531,62.5739512078933),.UNSPECIFIED.);
#860=B_SPLINE_CURVE_WITH_KNOTS('',3,(#51633,#51634,#51635,#51636,#51637),
 .UNSPECIFIED.,.F.,.F.,(4,1,4),(59.6902604182061,60.3416508638693,61.3394390286984),
 .UNSPECIFIED.);
#861=B_SPLINE_CURVE_WITH_KNOTS('',3,(#51642,#51643,#51644,#51645,#51646,
#51647,#51648,#51649,#51650,#51651,#51652),.UNSPECIFIED.,.F.,.F.,(4,1,1,
1,1,1,1,1,4),(53.4070751110265,53.6711949538987,54.6689831187277,55.6667712835568,
56.6645594483858,57.6623476132148,58.6601357780439,59.6579239428729,59.6902604182061),
 .UNSPECIFIED.);
#862=B_SPLINE_CURVE_WITH_KNOTS('',3,(#51653,#51654,#51655,#51656,#51657,
#51658,#51659,#51660,#51661,#51662),.UNSPECIFIED.,.F.,.F.,(4,1,1,1,1,1,
1,4),(53.4070751110265,54.3549218748951,55.3527100397241,56.3504982045531,
57.3482863693822,58.3460745342112,59.3438626990403,59.6902604182061),
 .UNSPECIFIED.);
#863=B_SPLINE_CURVE_WITH_KNOTS('',3,(#51667,#51668,#51669,#51670,#51671,
#51672,#51673,#51674,#51675,#51676),.UNSPECIFIED.,.F.,.F.,(4,1,1,1,1,1,
1,4),(47.1238898038469,47.6844659649244,48.6822541297535,49.6800422945825,
50.6778304594116,51.6756186242406,52.6734067890696,53.4070751110265),
 .UNSPECIFIED.);
#864=B_SPLINE_CURVE_WITH_KNOTS('',3,(#51677,#51678,#51679,#51680,#51681,
#51682,#51683,#51684,#51685,#51686,#51687),.UNSPECIFIED.,.F.,.F.,(4,1,1,
1,1,1,1,1,4),(47.1238898038469,47.3704047210918,48.3681928859208,49.3659810507499,
50.3637692155789,51.3615573804079,52.359345545237,53.357133710066,53.4070751110265),
 .UNSPECIFIED.);
#865=B_SPLINE_CURVE_WITH_KNOTS('',3,(#51692,#51693,#51694,#51695,#51696,
#51697,#51698,#51699,#51700,#51701),.UNSPECIFIED.,.F.,.F.,(4,1,1,1,1,1,
1,4),(40.8407044966673,41.6977369759502,42.6955251407792,43.6933133056083,
44.6911014704373,45.6888896352663,46.6866778000954,47.1238898038469),
 .UNSPECIFIED.);
#866=B_SPLINE_CURVE_WITH_KNOTS('',3,(#51702,#51703,#51704,#51705,#51706,
#51707,#51708,#51709,#51710,#51711),.UNSPECIFIED.,.F.,.F.,(4,1,1,1,1,1,
1,4),(40.8407044966673,41.3836757321175,42.3814638969466,43.3792520617756,
44.3770402266046,45.3748283914337,46.3726165562627,47.1238898038469),
 .UNSPECIFIED.);
#867=B_SPLINE_CURVE_WITH_KNOTS('',3,(#51716,#51717,#51718,#51719,#51720,
#51721,#51722,#51723,#51724,#51725,#51726),.UNSPECIFIED.,.F.,.F.,(4,1,1,
1,1,1,1,1,4),(34.5575191894877,34.7132198221469,35.7110079869759,36.708796151805,
37.706584316634,38.7043724814631,39.7021606462921,40.6999488111211,40.8407044966673),
 .UNSPECIFIED.);
#868=B_SPLINE_CURVE_WITH_KNOTS('',3,(#51727,#51728,#51729,#51730,#51731,
#51732,#51733,#51734,#51735,#51736),.UNSPECIFIED.,.F.,.F.,(4,1,1,1,1,1,
1,4),(34.5575191894877,35.3969467431433,36.3947349079723,37.3925230728014,
38.3903112376304,39.3880994024594,40.3858875672885,40.8407044966673),
 .UNSPECIFIED.);
#869=B_SPLINE_CURVE_WITH_KNOTS('',3,(#51741,#51742,#51743,#51744,#51745,
#51746,#51747,#51748,#51749,#51750),.UNSPECIFIED.,.F.,.F.,(4,1,1,1,1,1,
1,4),(28.2743338823081,28.7264908331727,29.7242789980017,30.7220671628307,
31.7198553276598,32.7176434924888,33.7154316573179,34.5575191894877),
 .UNSPECIFIED.);
#870=B_SPLINE_CURVE_WITH_KNOTS('',3,(#51751,#51752,#51753,#51754,#51755,
#51756,#51757,#51758,#51759,#51760,#51761),.UNSPECIFIED.,.F.,.F.,(4,1,1,
1,1,1,1,1,4),(28.2743338823081,28.41242958934,29.410217754169,30.4080059189981,
31.4057940838271,32.4035822486562,33.4013704134852,34.3991585783142,34.5575191894877),
 .UNSPECIFIED.);
#871=B_SPLINE_CURVE_WITH_KNOTS('',3,(#51766,#51767,#51768,#51769,#51770,
#51771,#51772,#51773,#51774,#51775),.UNSPECIFIED.,.F.,.F.,(4,1,1,1,1,1,
1,4),(21.9911485751285,22.7397618441984,23.7375500090275,24.7353381738565,
25.7331263386855,26.7309145035146,27.7287026683436,28.2743338823081),
 .UNSPECIFIED.);
#872=B_SPLINE_CURVE_WITH_KNOTS('',3,(#51776,#51777,#51778,#51779,#51780,
#51781,#51782,#51783,#51784,#51785),.UNSPECIFIED.,.F.,.F.,(4,1,1,1,1,1,
1,4),(21.9911485751285,22.4257006003658,23.4234887651948,24.4212769300238,
25.4190650948529,26.4168532596819,27.414641424511,28.2743338823081),
 .UNSPECIFIED.);
#873=B_SPLINE_CURVE_WITH_KNOTS('',3,(#51792,#51793,#51794,#51795,#51796,
#51797,#51798,#51799,#51800,#51801),.UNSPECIFIED.,.F.,.F.,(4,1,1,1,1,1,
1,4),(15.7552446903951,16.7530328552242,17.7508210200532,18.7486091848822,
19.7463973497113,20.7441855145403,21.7419736793694,21.9911485751285),
 .UNSPECIFIED.);
#874=B_SPLINE_CURVE_WITH_KNOTS('',3,(#51802,#51803,#51804,#51805,#51806,
#51807,#51808,#51809,#51810,#51811),.UNSPECIFIED.,.F.,.F.,(4,1,1,1,1,1,
1,4),(15.7079632679489,16.4389716113915,17.4367597762206,18.4345479410496,
19.4323361058786,20.4301242707077,21.4279124355367,21.9911485751285),
 .UNSPECIFIED.);
#875=B_SPLINE_CURVE_WITH_KNOTS('',3,(#52021,#52022,#52023,#52024,#52025,
#52026,#52027,#52028,#52029,#52030,#52031,#52032,#52033,#52034,#52035,#52036,
#52037,#52038,#52039,#52040,#52041,#52042,#52043,#52044,#52045,#52046,#52047,
#52048,#52049,#52050,#52051,#52052,#52053,#52054,#52055,#52056,#52057,#52058,
#52059,#52060,#52061,#52062,#52063,#52064,#52065,#52066),.UNSPECIFIED.,
 .F.,.F.,(4,3,3,3,3,3,3,3,3,3,3,3,3,3,3,4),(-0.140062757837278,-0.134123173823536,
-0.121523401165327,-0.113447705434834,-0.0990655075399137,-0.0919518085532341,
-0.0750566738033047,-0.0674043852357639,-0.0624390856721942,-0.0527351001118668,
-0.0459772985974198,-0.0296762170335496,-0.0230583683643434,-0.016477620433628,
-0.00151411940223995,0.),.UNSPECIFIED.);
#876=B_SPLINE_CURVE_WITH_KNOTS('',3,(#52067,#52068,#52069,#52070,#52071,
#52072,#52073,#52074,#52075,#52076,#52077,#52078,#52079,#52080,#52081,#52082,
#52083,#52084,#52085),.UNSPECIFIED.,.F.,.F.,(4,3,3,3,3,3,4),(40.9592561589511,
41.9071029228197,42.9048910876487,43.9026792524778,44.9004674173068,45.8982555821359,
46.8187065174982),.UNSPECIFIED.);
#877=B_SPLINE_CURVE_WITH_KNOTS('',3,(#52087,#52088,#52089,#52090,#52091,
#52092,#52093,#52094,#52095,#52096,#52097,#52098,#52099,#52100,#52101,#52102,
#52103,#52104,#52105,#52106,#52107,#52108,#52109,#52110,#52111,#52112,#52113,
#52114,#52115,#52116,#52117,#52118,#52119,#52120,#52121,#52122,#52123,#52124,
#52125,#52126,#52127,#52128,#52129,#52130,#52131,#52132),.UNSPECIFIED.,
 .F.,.F.,(4,3,3,3,3,3,3,3,3,3,3,3,3,3,3,4),(-0.140969988491048,-0.136446439322258,
-0.126660801898424,-0.119269074856758,-0.10953502353942,-0.102598331591438,
-0.0857596038079746,-0.0787758183049045,-0.072931898136125,-0.0587706520901876,
-0.0520483890707233,-0.0380705861802498,-0.0301255169382023,-0.023298848983932,
-0.00434997386540177,0.),.UNSPECIFIED.);
#878=B_SPLINE_CURVE_WITH_KNOTS('',3,(#52133,#52134,#52135,#52136,#52137),
 .UNSPECIFIED.,.F.,.F.,(4,1,4),(14.5207325112002,15.4411834465625,15.7079632679489),
 .UNSPECIFIED.);
#879=B_SPLINE_CURVE_WITH_KNOTS('',3,(#52139,#52140,#52141,#52142,#52143,
#52144,#52145,#52146,#52147,#52148,#52149,#52150,#52151,#52152,#52153,#52154,
#52155,#52156,#52157,#52158,#52159,#52160,#52161,#52162,#52163,#52164,#52165,
#52166,#52167,#52168,#52169,#52170,#52171,#52172,#52173,#52174,#52175,#52176,
#52177,#52178,#52179,#52180,#52181,#52182,#52183,#52184),.UNSPECIFIED.,
 .F.,.F.,(4,3,3,3,3,3,3,3,3,3,3,3,3,3,3,4),(-0.140062757837251,-0.134123173823509,
-0.121523399045325,-0.11344770204781,-0.0990654838477444,-0.0919518011861085,
-0.0750566620112235,-0.0674043807182989,-0.062439085672185,-0.0527351170922762,
-0.0459772905666743,-0.029676213594428,-0.0230583524982984,-0.0164776174494443,
-0.00151412549618594,0.),.UNSPECIFIED.);
#880=B_SPLINE_CURVE_WITH_KNOTS('',3,(#52396,#52397,#52398,#52399,#52400,
#52401,#52402,#52403,#52404,#52405,#52406,#52407,#52408,#52409,#52410,#52411,
#52412,#52413,#52414,#52415,#52416,#52417,#52418,#52419,#52420,#52421,#52422,
#52423,#52424,#52425,#52426,#52427,#52428,#52429,#52430,#52431,#52432,#52433,
#52434,#52435,#52436,#52437,#52438,#52439,#52440,#52441),.UNSPECIFIED.,
 .F.,.F.,(4,3,3,3,3,3,3,3,3,3,3,3,3,3,3,4),(-0.140969988491049,-0.136446439322259,
-0.126660808831101,-0.11926908034975,-0.109535054430385,-0.102598368559059,
-0.0857596411563137,-0.0787758156854511,-0.0729318981361281,-0.0587706585020556,
-0.0520483951910087,-0.0380705929416598,-0.030125518229324,-0.0232988520606989,
-0.00434997944539849,0.),.UNSPECIFIED.);
#881=B_SPLINE_CURVE_WITH_KNOTS('',3,(#52442,#52443,#52444,#52445,#52446,
#52447,#52448,#52449,#52450,#52451,#52452,#52453,#52454,#52455,#52456,#52457),
 .UNSPECIFIED.,.F.,.F.,(4,3,3,3,3,4),(-48.891620076623,-47.893831911794,
-46.8960437469649,-45.8982555821359,-44.9004674173068,-43.9350157278109),
 .UNSPECIFIED.);
#882=B_SPLINE_CURVE_WITH_KNOTS('',3,(#52556,#52557,#52558,#52559,#52560,
#52561,#52562,#52563,#52564,#52565,#52566,#52567,#52568,#52569,#52570,#52571),
 .UNSPECIFIED.,.F.,.F.,(4,3,3,3,3,4),(-6.23590388473343,-5.98529092066965,
-4.98774243389138,-3.9901939471131,-2.99264546033482,-2.07291355912486),
 .UNSPECIFIED.);
#883=B_SPLINE_CURVE_WITH_KNOTS('',3,(#52579,#52580,#52581,#52582,#52583,
#52584,#52585,#52586,#52587,#52588,#52589,#52590,#52591),.UNSPECIFIED.,
 .F.,.F.,(4,3,3,3,4),(0.,0.997548486778257,1.99509697355654,2.99264546033483,
3.26014431587347),.UNSPECIFIED.);
#884=B_SPLINE_CURVE_WITH_KNOTS('',3,(#52596,#52597,#52598,#52599,#52600,
#52601,#52602,#52603,#52604,#52605,#52606,#52607,#52608,#52609,#52610,#52611,
#52612,#52613,#52614,#52615,#52616,#52617),.UNSPECIFIED.,.F.,.F.,(4,3,3,
3,3,3,3,4),(-12.519089191913,-11.9705818413393,-10.973033354561,-9.97548486778276,
-8.97793638100448,-7.9803878942262,-6.98283940744793,-6.23590388473343),
 .UNSPECIFIED.);
#885=B_SPLINE_CURVE_WITH_KNOTS('',3,(#52618,#52619,#52620,#52621,#52622,
#52623,#52624,#52625,#52626,#52627,#52628,#52629,#52630,#52631,#52632,#52633,
#52634,#52635,#52636,#52637,#52638,#52639),.UNSPECIFIED.,.F.,.F.,(4,3,3,
3,3,3,3,4),(3.26014431587347,3.99019394711311,4.98774243389138,5.98529092066965,
6.98283940744792,7.9803878942262,8.97793638100447,9.54332962305307),
 .UNSPECIFIED.);
#886=B_SPLINE_CURVE_WITH_KNOTS('',3,(#52644,#52645,#52646,#52647,#52648,
#52649,#52650,#52651,#52652,#52653,#52654,#52655,#52656,#52657,#52658,#52659,
#52660,#52661,#52662,#52663,#52664,#52665),.UNSPECIFIED.,.F.,.F.,(4,3,3,
3,3,3,3,4),(-18.8022744990926,-17.955872762009,-16.9583242752307,-15.9607757884524,
-14.9632273016741,-13.9656788148959,-12.9681303281176,-12.519089191913),
 .UNSPECIFIED.);
#887=B_SPLINE_CURVE_WITH_KNOTS('',3,(#52666,#52667,#52668,#52669,#52670,
#52671,#52672,#52673,#52674,#52675,#52676,#52677,#52678,#52679,#52680,#52681,
#52682,#52683,#52684,#52685,#52686,#52687),.UNSPECIFIED.,.F.,.F.,(4,3,3,
3,3,3,3,4),(9.54332962305307,9.97548486778275,10.973033354561,11.9705818413393,
12.9681303281176,13.9656788148959,14.9632273016741,15.8265149302327),
 .UNSPECIFIED.);
#888=B_SPLINE_CURVE_WITH_KNOTS('',3,(#52692,#52693,#52694,#52695,#52696,
#52697,#52698,#52699,#52700,#52701,#52702,#52703,#52704,#52705,#52706,#52707,
#52708,#52709,#52710,#52711,#52712,#52713,#52714,#52715,#52716),
 .UNSPECIFIED.,.F.,.F.,(4,3,3,3,3,3,3,3,4),(-25.0854598062722,-24.9387121694569,
-23.9411636826786,-22.9436151959003,-21.9460667091221,-20.9485182223438,
-19.9509697355655,-18.9534212487872,-18.8022744990926),.UNSPECIFIED.);
#889=B_SPLINE_CURVE_WITH_KNOTS('',3,(#52717,#52718,#52719,#52720,#52721,
#52722,#52723,#52724,#52725,#52726,#52727,#52728,#52729,#52730,#52731,#52732,
#52733,#52734,#52735,#52736,#52737,#52738,#52739,#52740,#52741),
 .UNSPECIFIED.,.F.,.F.,(4,3,3,3,3,3,3,3,4),(15.8265149302327,15.9607757884524,
16.9583242752307,17.955872762009,18.9534212487872,19.9509697355655,20.9485182223438,
21.9460667091221,22.1097002374122),.UNSPECIFIED.);
#890=B_SPLINE_CURVE_WITH_KNOTS('',3,(#52746,#52747,#52748,#52749,#52750,
#52751,#52752,#52753,#52754,#52755,#52756,#52757,#52758,#52759,#52760,#52761,
#52762,#52763,#52764,#52765,#52766,#52767),.UNSPECIFIED.,.F.,.F.,(4,3,3,
3,3,3,3,4),(-31.3686451134518,-30.9240030901265,-29.9264546033483,-28.92890611657,
-27.9313576297917,-26.9338091430134,-25.9362606562352,-25.0854598062722),
 .UNSPECIFIED.);
#891=B_SPLINE_CURVE_WITH_KNOTS('',3,(#52768,#52769,#52770,#52771,#52772,
#52773,#52774,#52775,#52776,#52777,#52778,#52779,#52780,#52781,#52782,#52783,
#52784,#52785,#52786,#52787,#52788,#52789),.UNSPECIFIED.,.F.,.F.,(4,3,3,
3,3,3,3,4),(22.1097002374122,22.9436151959003,23.9411636826786,24.9387121694569,
25.9362606562352,26.9338091430134,27.9313576297917,28.3928855445918),
 .UNSPECIFIED.);
#892=B_SPLINE_CURVE_WITH_KNOTS('',3,(#52794,#52795,#52796,#52797,#52798,
#52799,#52800,#52801,#52802,#52803,#52804,#52805,#52806,#52807,#52808,#52809,
#52810,#52811,#52812,#52813,#52814,#52815),.UNSPECIFIED.,.F.,.F.,(4,3,3,
3,3,3,3,4),(-37.6518304206314,-36.9092940107962,-35.9117455240179,-34.9141970372396,
-33.9166485504614,-32.9191000636831,-31.9215515769048,-31.3686451134518),
 .UNSPECIFIED.);
#893=B_SPLINE_CURVE_WITH_KNOTS('',3,(#52816,#52817,#52818,#52819,#52820,
#52821,#52822,#52823,#52824,#52825,#52826,#52827,#52828,#52829,#52830,#52831,
#52832,#52833,#52834,#52835,#52836,#52837),.UNSPECIFIED.,.F.,.F.,(4,3,3,
3,3,3,3,4),(28.3928855445918,28.92890611657,29.9264546033483,30.9240030901265,
31.9215515769048,32.9191000636831,33.9166485504614,34.6760708517714),
 .UNSPECIFIED.);
#894=B_SPLINE_CURVE_WITH_KNOTS('',3,(#52842,#52843,#52844,#52845,#52846,
#52847,#52848,#52849,#52850,#52851,#52852,#52853,#52854,#52855,#52856,#52857,
#52858,#52859,#52860,#52861,#52862,#52863,#52864,#52865,#52866),
 .UNSPECIFIED.,.F.,.F.,(4,3,3,3,3,3,3,3,4),(-43.9350157278109,-43.8921334182441,
-42.8945849314659,-41.8970364446876,-40.8994879579093,-39.901939471131,
-38.9043909843527,-37.9068424975745,-37.6518304206314),.UNSPECIFIED.);
#895=B_SPLINE_CURVE_WITH_KNOTS('',3,(#52867,#52868,#52869,#52870,#52871,
#52872,#52873,#52874,#52875,#52876,#52877,#52878,#52879,#52880,#52881,#52882,
#52883,#52884,#52885,#52886,#52887,#52888,#52889,#52890,#52891),
 .UNSPECIFIED.,.F.,.F.,(4,3,3,3,3,3,3,3,4),(34.6760708517714,34.9141970372396,
35.9117455240179,36.9092940107962,37.9068424975745,38.9043909843527,39.901939471131,
40.8994879579093,40.959256158951),.UNSPECIFIED.);
#896=B_SPLINE_CURVE_WITH_KNOTS('',3,(#52896,#52897,#52898,#52899,#52900,
#52901,#52902,#52903,#52904,#52905,#52906,#52907,#52908,#52909,#52910,#52911,
#52912,#52913,#52914,#52915,#52916,#52917),.UNSPECIFIED.,.F.,.F.,(4,3,3,
3,3,3,3,4),(-50.2182010349905,-49.8774243389138,-48.8798758521355,-47.8823273653572,
-46.8847788785789,-45.8872303918007,-44.8896819050224,-43.9350157278109),
 .UNSPECIFIED.);
#897=B_SPLINE_CURVE_WITH_KNOTS('',3,(#52918,#52919,#52920,#52921,#52922,
#52923,#52924,#52925,#52926,#52927,#52928,#52929,#52930,#52931,#52932,#52933,
#52934,#52935,#52936,#52937,#52938,#52939),.UNSPECIFIED.,.F.,.F.,(4,3,3,
3,3,3,3,4),(40.959256158951,41.8970364446876,42.8945849314658,43.8921334182441,
44.8896819050224,45.8872303918007,46.8847788785789,47.2424414661306),
 .UNSPECIFIED.);
#898=B_SPLINE_CURVE_WITH_KNOTS('',3,(#52944,#52945,#52946,#52947,#52948,
#52949,#52950,#52951,#52952,#52953,#52954,#52955,#52956,#52957,#52958,#52959,
#52960,#52961,#52962,#52963,#52964,#52965),.UNSPECIFIED.,.F.,.F.,(4,3,3,
3,3,3,3,4),(-56.5013863421701,-55.8627152595834,-54.8651667728052,-53.8676182860269,
-52.8700697992486,-51.8725213124703,-50.874972825692,-50.2182010349905),
 .UNSPECIFIED.);
#899=B_SPLINE_CURVE_WITH_KNOTS('',3,(#52966,#52967,#52968,#52969,#52970,
#52971,#52972,#52973,#52974,#52975,#52976,#52977,#52978,#52979,#52980,#52981,
#52982,#52983,#52984,#52985,#52986,#52987),.UNSPECIFIED.,.F.,.F.,(4,3,3,
3,3,3,3,4),(47.2424414661306,47.8823273653572,48.8798758521355,49.8774243389137,
50.874972825692,51.8725213124703,52.8700697992486,53.5256267733102),
 .UNSPECIFIED.);
#900=B_SPLINE_CURVE_WITH_KNOTS('',3,(#52992,#52993,#52994,#52995,#52996,
#52997,#52998,#52999,#53000,#53001,#53002,#53003,#53004,#53005,#53006,#53007,
#53008,#53009,#53010,#53011,#53012,#53013),.UNSPECIFIED.,.F.,.F.,(4,3,3,
3,3,3,3,4),(-62.7845716493497,-61.8480061802531,-60.8504576934748,-59.8529092066965,
-58.8553607199183,-57.85781223314,-56.8602637463617,-56.5013863421701),
 .UNSPECIFIED.);
#901=B_SPLINE_CURVE_WITH_KNOTS('',3,(#53014,#53015,#53016,#53017,#53018,
#53019,#53020,#53021,#53022,#53023,#53024,#53025,#53026,#53027,#53028,#53029,
#53030,#53031,#53032,#53033,#53034,#53035),.UNSPECIFIED.,.F.,.F.,(4,3,3,
3,3,3,3,4),(53.5256267733102,53.8676182860269,54.8651667728051,55.8627152595834,
56.8602637463617,57.85781223314,58.8553607199182,59.8088120804898),
 .UNSPECIFIED.);
#902=B_SPLINE_CURVE_WITH_KNOTS('',3,(#53040,#53041,#53042,#53043,#53044,
#53045,#53046,#53047,#53048,#53049,#53050,#53051,#53052,#53053,#53054,#53055,
#53056,#53057,#53058,#53059,#53060,#53061,#53062,#53063,#53064),
 .UNSPECIFIED.,.F.,.F.,(4,3,3,3,3,3,3,3,4),(-69.0677569565293,-68.830845587701,
-67.8332971009227,-66.8357486141444,-65.8382001273662,-64.8406516405879,
-63.8431031538096,-62.8455546670314,-62.7845716493497),.UNSPECIFIED.);
#903=B_SPLINE_CURVE_WITH_KNOTS('',3,(#53065,#53066,#53067,#53068,#53069,
#53070,#53071,#53072,#53073,#53074,#53075,#53076,#53077,#53078,#53079,#53080,
#53081,#53082,#53083,#53084,#53085,#53086,#53087,#53088,#53089),
 .UNSPECIFIED.,.F.,.F.,(4,3,3,3,3,3,3,3,4),(59.8088120804898,59.8529092066965,
60.8504576934748,61.8480061802531,62.8455546670313,63.8431031538096,64.8406516405879,
65.8382001273662,66.0919973876694),.UNSPECIFIED.);
#904=B_SPLINE_CURVE_WITH_KNOTS('',3,(#53094,#53095,#53096,#53097,#53098,
#53099,#53100,#53101,#53102,#53103,#53104,#53105,#53106,#53107,#53108,#53109,
#53110,#53111,#53112,#53113,#53114,#53115),.UNSPECIFIED.,.F.,.F.,(4,3,3,
3,3,3,3,4),(-75.3509422637089,-74.8161365083707,-73.8185880215924,-72.8210395348141,
-71.8234910480358,-70.8259425612576,-69.8283940744793,-69.0677569565293),
 .UNSPECIFIED.);
#905=B_SPLINE_CURVE_WITH_KNOTS('',3,(#53116,#53117,#53118,#53119,#53120,
#53121,#53122,#53123,#53124,#53125,#53126,#53127,#53128,#53129,#53130,#53131,
#53132,#53133,#53134,#53135,#53136,#53137),.UNSPECIFIED.,.F.,.F.,(4,3,3,
3,3,3,3,4),(66.0919973876694,66.8357486141444,67.8332971009227,68.830845587701,
69.8283940744792,70.8259425612575,71.8234910480358,72.375182694849),
 .UNSPECIFIED.);
#906=B_SPLINE_CURVE_WITH_KNOTS('',3,(#53142,#53143,#53144,#53145,#53146,
#53147,#53148,#53149,#53150,#53151,#53152,#53153,#53154,#53155,#53156,#53157,
#53158,#53159,#53160,#53161,#53162,#53163),.UNSPECIFIED.,.F.,.F.,(4,3,3,
3,3,3,3,4),(-81.6341275708885,-80.8014274290403,-79.803878942262,-78.8063304554838,
-77.8087819687055,-76.8112334819272,-75.8136849951489,-75.3509422637089),
 .UNSPECIFIED.);
#907=B_SPLINE_CURVE_WITH_KNOTS('',3,(#53164,#53165,#53166,#53167,#53168,
#53169,#53170,#53171,#53172,#53173,#53174,#53175,#53176,#53177,#53178,#53179,
#53180,#53181,#53182,#53183,#53184,#53185),.UNSPECIFIED.,.F.,.F.,(4,3,3,
3,3,3,3,4),(72.375182694849,72.8210395348141,73.8185880215924,74.8161365083706,
75.8136849951489,76.8112334819272,77.8087819687055,78.6583680020286),
 .UNSPECIFIED.);
#908=B_SPLINE_CURVE_WITH_KNOTS('',3,(#53190,#53191,#53192,#53193,#53194,
#53195,#53196,#53197,#53198,#53199,#53200,#53201,#53202,#53203,#53204,#53205,
#53206,#53207,#53208,#53209,#53210,#53211,#53212,#53213,#53214),
 .UNSPECIFIED.,.F.,.F.,(4,3,3,3,3,3,3,3,4),(-87.9173128780681,-87.7842668364882,
-86.78671834971,-85.7891698629317,-84.7916213761534,-83.7940728893752,-82.7965244025969,
-81.7989759158186,-81.6341275708885),.UNSPECIFIED.);
#909=B_SPLINE_CURVE_WITH_KNOTS('',3,(#53215,#53216,#53217,#53218,#53219,
#53220,#53221,#53222,#53223,#53224,#53225,#53226,#53227,#53228,#53229,#53230,
#53231,#53232,#53233,#53234,#53235,#53236,#53237,#53238,#53239),
 .UNSPECIFIED.,.F.,.F.,(4,3,3,3,3,3,3,3,4),(78.6583680020286,78.8063304554837,
79.803878942262,80.8014274290403,81.7989759158185,82.7965244025968,83.7940728893751,
84.7916213761534,84.9415533092082),.UNSPECIFIED.);
#910=B_SPLINE_CURVE_WITH_KNOTS('',3,(#53244,#53245,#53246,#53247,#53248,
#53249,#53250,#53251,#53252,#53253,#53254,#53255,#53256,#53257,#53258,#53259,
#53260,#53261,#53262,#53263,#53264,#53265),.UNSPECIFIED.,.F.,.F.,(4,3,3,
3,3,3,3,4),(-94.2004981852477,-93.7695577571579,-92.7720092703796,-91.7744607836013,
-90.7769122968231,-89.7793638100448,-88.7818153232665,-87.9173128780681),
 .UNSPECIFIED.);
#911=B_SPLINE_CURVE_WITH_KNOTS('',3,(#53266,#53267,#53268,#53269,#53270,
#53271,#53272,#53273,#53274,#53275,#53276,#53277,#53278,#53279,#53280,#53281,
#53282,#53283,#53284,#53285,#53286,#53287),.UNSPECIFIED.,.F.,.F.,(4,3,3,
3,3,3,3,4),(84.9415533092082,85.7891698629316,86.7867183497099,87.7842668364882,
88.7818153232665,89.7793638100448,90.776912296823,91.2247386163878),
 .UNSPECIFIED.);
#912=B_SPLINE_CURVE_WITH_KNOTS('',3,(#53292,#53293,#53294,#53295,#53296,
#53297,#53298,#53299,#53300,#53301,#53302,#53303,#53304,#53305,#53306,#53307,
#53308,#53309,#53310,#53311,#53312,#53313),.UNSPECIFIED.,.F.,.F.,(4,3,3,
3,3,3,3,4),(-100.483683492427,-99.7548486778276,-98.7573001910493,-97.759751704271,
-96.7622032174927,-95.7646547307145,-94.7671062439362,-94.2004981852477),
 .UNSPECIFIED.);
#913=B_SPLINE_CURVE_WITH_KNOTS('',3,(#53314,#53315,#53316,#53317,#53318,
#53319,#53320,#53321,#53322,#53323,#53324,#53325,#53326,#53327,#53328,#53329,
#53330,#53331,#53332,#53333,#53334,#53335),.UNSPECIFIED.,.F.,.F.,(4,3,3,
3,3,3,3,4),(91.2247386163878,91.7744607836013,92.7720092703796,93.7695577571579,
94.7671062439361,95.7646547307144,96.7622032174927,97.5079239235673),
 .UNSPECIFIED.);
#914=B_SPLINE_CURVE_WITH_KNOTS('',3,(#53341,#53342,#53343,#53344),
 .UNSPECIFIED.,.F.,.F.,(4,4),(116.238928182822,116.429825269433),
 .UNSPECIFIED.);
#915=B_SPLINE_CURVE_WITH_KNOTS('',3,(#53350,#53351,#53352,#53353,#53354,
#53355,#53356,#53357,#53358,#53359),.UNSPECIFIED.,.F.,.F.,(4,1,1,1,1,1,
1,4),(109.955742875643,110.522350934331,111.519899421109,112.517447907888,
113.514996394666,114.512544881444,115.510093368223,116.238928182822),
 .UNSPECIFIED.);
#916=B_SPLINE_CURVE_WITH_KNOTS('',3,(#53362,#53363,#53364,#53365,#53366,
#53367,#53368,#53369,#53370),.UNSPECIFIED.,.F.,.F.,(4,1,1,1,1,1,4),(109.955742875643,
110.207570656346,111.205119143125,112.202667629903,113.200216116681,114.197764603459,
115.195313090238),.UNSPECIFIED.);
#917=B_SPLINE_CURVE_WITH_KNOTS('',3,(#53375,#53376,#53377,#53378,#53379,
#53380,#53381,#53382,#53383,#53384),.UNSPECIFIED.,.F.,.F.,(4,1,1,1,1,1,
1,4),(103.672557568463,104.537060013662,105.53460850044,106.532156987218,
107.529705473996,108.527253960775,109.524802447553,109.955742875643),
 .UNSPECIFIED.);
#918=B_SPLINE_CURVE_WITH_KNOTS('',3,(#53385,#53386,#53387,#53388,#53389,
#53390,#53391,#53392,#53393,#53394),.UNSPECIFIED.,.F.,.F.,(4,1,1,1,1,1,
1,4),(103.672557568463,104.222279735677,105.219828222455,106.217376709233,
107.214925196011,108.21247368279,109.210022169568,109.955742875643),
 .UNSPECIFIED.);
#919=B_SPLINE_CURVE_WITH_KNOTS('',3,(#53399,#53400,#53401,#53402,#53403,
#53404,#53405,#53406,#53407,#53408,#53409),.UNSPECIFIED.,.F.,.F.,(4,1,1,
1,1,1,1,1,4),(97.3893722612836,97.5542206062136,98.5517690929919,99.5493175797702,
100.546866066548,101.544414553327,102.541963040105,103.539511526883,103.672557568463),
 .UNSPECIFIED.);
#920=B_SPLINE_CURVE_WITH_KNOTS('',3,(#53410,#53411,#53412,#53413,#53414,
#53415,#53416,#53417,#53418,#53419),.UNSPECIFIED.,.F.,.F.,(4,1,1,1,1,1,
1,4),(97.3893722612836,98.236988815007,99.2345373017852,100.232085788564,
101.229634275342,102.22718276212,103.224731248898,103.672557568463),
 .UNSPECIFIED.);
#921=B_SPLINE_CURVE_WITH_KNOTS('',3,(#53424,#53425,#53426,#53427,#53428,
#53429,#53430,#53431,#53432,#53433),.UNSPECIFIED.,.F.,.F.,(4,1,1,1,1,1,
1,4),(91.106186954104,91.568929685544,92.5664781723222,93.5640266591005,
94.5615751458788,95.5591236326571,96.5566721194354,97.3893722612836),
 .UNSPECIFIED.);
#922=B_SPLINE_CURVE_WITH_KNOTS('',3,(#53434,#53435,#53436,#53437,#53438,
#53439,#53440,#53441,#53442,#53443,#53444),.UNSPECIFIED.,.F.,.F.,(4,1,1,
1,1,1,1,1,4),(91.106186954104,91.254149407559,92.2516978943373,93.2492463811156,
94.2467948678939,95.2443433546721,96.2418918414504,97.2394403282287,97.3893722612836),
 .UNSPECIFIED.);
#923=B_SPLINE_CURVE_WITH_KNOTS('',3,(#53449,#53450,#53451,#53452,#53453,
#53454,#53455,#53456,#53457,#53458),.UNSPECIFIED.,.F.,.F.,(4,1,1,1,1,1,
1,4),(84.8230016469244,85.5836387648743,86.5811872516526,87.5787357384309,
88.5762842252092,89.5738327119874,90.5713811987657,91.106186954104),
 .UNSPECIFIED.);
#924=B_SPLINE_CURVE_WITH_KNOTS('',3,(#53459,#53460,#53461,#53462,#53463,
#53464,#53465,#53466,#53467,#53468),.UNSPECIFIED.,.F.,.F.,(4,1,1,1,1,1,
1,4),(84.8230016469244,85.2688584868894,86.2664069736677,87.2639554604459,
88.2615039472242,89.2590524340025,90.2566009207808,91.106186954104),
 .UNSPECIFIED.);
#925=B_SPLINE_CURVE_WITH_KNOTS('',3,(#53473,#53474,#53475,#53476,#53477,
#53478,#53479,#53480,#53481,#53482,#53483),.UNSPECIFIED.,.F.,.F.,(4,1,1,
1,1,1,1,1,4),(78.5398163397448,78.6007993574264,79.5983478442047,80.595896330983,
81.5934448177612,82.5909933045395,83.5885417913178,84.5860902780961,84.8230016469244),
 .UNSPECIFIED.);
#926=B_SPLINE_CURVE_WITH_KNOTS('',3,(#53484,#53485,#53486,#53487,#53488,
#53489,#53490,#53491,#53492,#53493),.UNSPECIFIED.,.F.,.F.,(4,1,1,1,1,1,
1,4),(78.5398163397448,79.2835675662197,80.281116052998,81.2786645397763,
82.2762130265546,83.2737615133328,84.2713100001111,84.8230016469244),
 .UNSPECIFIED.);
#927=B_SPLINE_CURVE_WITH_KNOTS('',3,(#53498,#53499,#53500,#53501,#53502,
#53503,#53504,#53505,#53506,#53507),.UNSPECIFIED.,.F.,.F.,(4,1,1,1,1,1,
1,4),(72.2566310325652,72.6155084367567,73.613056923535,74.6106054103133,
75.6081538970916,76.6057023838698,77.6032508706481,78.5398163397448),
 .UNSPECIFIED.);
#928=B_SPLINE_CURVE_WITH_KNOTS('',3,(#53508,#53509,#53510,#53511,#53512,
#53513,#53514,#53515,#53516,#53517,#53518),.UNSPECIFIED.,.F.,.F.,(4,1,1,
1,1,1,1,1,4),(72.2566310325652,72.3007281587718,73.2982766455501,74.2958251323284,
75.2933736191066,76.2909221058849,77.2884705926632,78.2860190794415,78.5398163397448),
 .UNSPECIFIED.);
#929=B_SPLINE_CURVE_WITH_KNOTS('',3,(#53523,#53524,#53525,#53526,#53527,
#53528,#53529,#53530,#53531,#53532),.UNSPECIFIED.,.F.,.F.,(4,1,1,1,1,1,
1,4),(65.9734457253856,66.6302175160871,67.6277660028654,68.6253144896436,
69.6228629764219,70.6204114632002,71.6179599499785,72.2566310325652),
 .UNSPECIFIED.);
#930=B_SPLINE_CURVE_WITH_KNOTS('',3,(#53533,#53534,#53535,#53536,#53537,
#53538,#53539,#53540,#53541,#53542),.UNSPECIFIED.,.F.,.F.,(4,1,1,1,1,1,
1,4),(65.9734457253856,66.3154372381021,67.3129857248804,68.3105342116587,
69.308082698437,70.3056311852153,71.3031796719935,72.2566310325652),
 .UNSPECIFIED.);
#931=B_SPLINE_CURVE_WITH_KNOTS('',3,(#53547,#53548,#53549,#53550,#53551,
#53552,#53553,#53554,#53555,#53556),.UNSPECIFIED.,.F.,.F.,(4,1,1,1,1,1,
1,4),(59.690260418206,60.6449265954174,61.6424750821957,62.640023568974,
63.6375720557523,64.6351205425305,65.6326690293088,65.9734457253856),
 .UNSPECIFIED.);
#932=B_SPLINE_CURVE_WITH_KNOTS('',3,(#53557,#53558,#53559,#53560,#53561,
#53562,#53563,#53564,#53565,#53566),.UNSPECIFIED.,.F.,.F.,(4,1,1,1,1,1,
1,4),(59.690260418206,60.3301463174325,61.3276948042108,62.3252432909891,
63.3227917777673,64.3203402645456,65.3178887513239,65.9734457253856),
 .UNSPECIFIED.);
#933=B_SPLINE_CURVE_WITH_KNOTS('',3,(#53571,#53572,#53573,#53574,#53575,
#53576,#53577,#53578,#53579,#53580,#53581),.UNSPECIFIED.,.F.,.F.,(4,1,1,
1,1,1,1,1,4),(53.4070751110265,53.6620871879695,54.6596356747478,55.6571841615261,
56.6547326483043,57.6522811350826,58.6498296218609,59.6473781086392,59.690260418206),
 .UNSPECIFIED.);
#934=B_SPLINE_CURVE_WITH_KNOTS('',3,(#53582,#53583,#53584,#53585,#53586,
#53587,#53588,#53589,#53590,#53591),.UNSPECIFIED.,.F.,.F.,(4,1,1,1,1,1,
1,4),(53.4070751110264,54.3448553967629,55.3424038835411,56.3399523703194,
57.3375008570977,58.335049343876,59.3325978306542,59.690260418206),
 .UNSPECIFIED.);
#935=B_SPLINE_CURVE_WITH_KNOTS('',3,(#53596,#53597,#53598,#53599,#53600,
#53601,#53602,#53603,#53604,#53605),.UNSPECIFIED.,.F.,.F.,(4,1,1,1,1,1,
1,4),(47.1238898038469,47.6767962672999,48.6743447540781,49.6718932408564,
50.6694417276347,51.666990214413,52.6645387011912,53.4070751110265),
 .UNSPECIFIED.);
#936=B_SPLINE_CURVE_WITH_KNOTS('',3,(#53606,#53607,#53608,#53609,#53610,
#53611,#53612,#53613,#53614,#53615,#53616),.UNSPECIFIED.,.F.,.F.,(4,1,1,
1,1,1,1,1,4),(47.1238898038468,47.3620159893149,48.3595644760932,49.3571129628715,
50.3546614496498,51.352209936428,52.3497584232063,53.3473069099846,53.4070751110264),
 .UNSPECIFIED.);
#937=B_SPLINE_CURVE_WITH_KNOTS('',3,(#53621,#53622,#53623,#53624,#53625,
#53626,#53627,#53628,#53629,#53630),.UNSPECIFIED.,.F.,.F.,(4,1,1,1,1,1,
1,4),(40.8407044966673,41.6915053466302,42.6890538334085,43.6866023201868,
44.684150806965,45.6816992937433,46.6792477805216,47.1238898038469),
 .UNSPECIFIED.);
#938=B_SPLINE_CURVE_WITH_KNOTS('',3,(#53631,#53632,#53633,#53634,#53635,
#53636,#53637,#53638,#53639,#53640),.UNSPECIFIED.,.F.,.F.,(4,1,1,1,1,1,
1,4),(40.8407044966672,41.3767250686453,42.3742735554236,43.3718220422018,
44.3693705289801,45.3669190157584,46.3644675025367,47.1238898038468),
 .UNSPECIFIED.);
#939=B_SPLINE_CURVE_WITH_KNOTS('',3,(#53645,#53646,#53647,#53648,#53649,
#53650,#53651,#53652,#53653,#53654,#53655),.UNSPECIFIED.,.F.,.F.,(4,1,1,
1,1,1,1,1,4),(34.5575191894877,34.7086659391823,35.7062144259606,36.7037629127388,
37.7013113995171,38.6988598862954,39.6964083730737,40.6939568598519,40.8407044966673),
 .UNSPECIFIED.);
#940=B_SPLINE_CURVE_WITH_KNOTS('',3,(#53656,#53657,#53658,#53659,#53660,
#53661,#53662,#53663,#53664,#53665),.UNSPECIFIED.,.F.,.F.,(4,1,1,1,1,1,
1,4),(34.5575191894876,35.3914341479756,36.3889826347539,37.3865311215322,
38.3840796083105,39.3816280950887,40.379176581867,40.8407044966672),
 .UNSPECIFIED.);
#941=B_SPLINE_CURVE_WITH_KNOTS('',3,(#53670,#53671,#53672,#53673,#53674,
#53675,#53676,#53677,#53678,#53679),.UNSPECIFIED.,.F.,.F.,(4,1,1,1,1,1,
1,4),(28.2743338823081,28.7233750185126,29.7209235052909,30.7184719920692,
31.7160204788475,32.7135689656257,33.711117452404,34.5575191894877),
 .UNSPECIFIED.);
#942=B_SPLINE_CURVE_WITH_KNOTS('',3,(#53680,#53681,#53682,#53683,#53684,
#53685,#53686,#53687,#53688,#53689,#53690),.UNSPECIFIED.,.F.,.F.,(4,1,1,
1,1,1,1,1,4),(28.274333882308,28.4085947405277,29.406143227306,30.4036917140842,
31.4012402008625,32.3987886876408,33.3963371744191,34.3938856611974,34.5575191894876),
 .UNSPECIFIED.);
#943=B_SPLINE_CURVE_WITH_KNOTS('',3,(#53695,#53696,#53697,#53698,#53699,
#53700,#53701,#53702,#53703,#53704),.UNSPECIFIED.,.F.,.F.,(4,1,1,1,1,1,
1,4),(21.9911485751285,22.738084097843,23.7356325846212,24.7331810713995,
25.7307295581778,26.7282780449561,27.7258265317343,28.2743338823081),
 .UNSPECIFIED.);
#944=B_SPLINE_CURVE_WITH_KNOTS('',3,(#53705,#53706,#53707,#53708,#53709,
#53710,#53711,#53712,#53713,#53714),.UNSPECIFIED.,.F.,.F.,(4,1,1,1,1,1,
1,4),(21.9911485751285,22.423303819858,23.4208523066363,24.4184007934146,
25.4159492801929,26.4134977669712,27.4110462537494,28.274333882308),
 .UNSPECIFIED.);
#945=B_SPLINE_CURVE_WITH_KNOTS('',3,(#53721,#53722,#53723,#53724,#53725,
#53726,#53727,#53728,#53729,#53730),.UNSPECIFIED.,.F.,.F.,(4,1,1,1,1,1,
1,4),(15.755244690395,16.7527931771733,17.7503416639516,18.7478901507299,
19.7454386375081,20.7429871242864,21.7405356110647,21.9911485751285),
 .UNSPECIFIED.);
#946=B_SPLINE_CURVE_WITH_KNOTS('',3,(#53731,#53732,#53733,#53734,#53735,
#53736,#53737,#53738,#53739,#53740),.UNSPECIFIED.,.F.,.F.,(4,1,1,1,1,1,
1,4),(15.7079632679489,16.4380128991884,17.4355613859667,18.433109872745,
19.4306583595232,20.4282068463015,21.4257553330798,21.9911485751285),
 .UNSPECIFIED.);
#947=B_SPLINE_CURVE_WITH_KNOTS('',3,(#54166,#54167,#54168,#54169,#54170,
#54171,#54172,#54173,#54174,#54175,#54176,#54177,#54178,#54179,#54180,#54181,
#54182,#54183,#54184,#54185,#54186,#54187,#54188,#54189,#54190,#54191,#54192,
#54193,#54194,#54195,#54196,#54197,#54198,#54199,#54200,#54201,#54202,#54203,
#54204,#54205,#54206,#54207,#54208,#54209,#54210,#54211),.UNSPECIFIED.,
 .F.,.F.,(4,3,3,3,3,3,3,3,3,3,3,3,3,3,3,4),(-0.140062757837262,-0.134086502655375,
-0.12147120271553,-0.113407421882847,-0.103769248913591,-0.0940394054438087,
-0.077137461601402,-0.0675091408822671,-0.0624229504780978,-0.0526720700183036,
-0.045988001471802,-0.0296865557803863,-0.0231241453191696,-0.0164915301952035,
-0.00152741804160966,0.),.UNSPECIFIED.);
#948=B_SPLINE_CURVE_WITH_KNOTS('',3,(#54212,#54213,#54214,#54215,#54216,
#54217,#54218,#54219,#54220,#54221,#54222,#54223,#54224),.UNSPECIFIED.,
 .F.,.F.,(4,3,3,3,4),(97.5079239235673,97.759751704271,98.7573001910492,
99.7548486778275,100.674580579037),.UNSPECIFIED.);
#949=B_SPLINE_CURVE_WITH_KNOTS('',3,(#54226,#54227,#54228,#54229,#54230,
#54231,#54232,#54233,#54234,#54235,#54236,#54237,#54238,#54239,#54240,#54241,
#54242,#54243,#54244,#54245,#54246,#54247,#54248,#54249,#54250,#54251,#54252,
#54253,#54254,#54255,#54256,#54257,#54258,#54259,#54260,#54261,#54262,#54263,
#54264,#54265,#54266,#54267,#54268,#54269,#54270,#54271,#54272,#54273,#54274),
 .UNSPECIFIED.,.F.,.F.,(4,3,3,3,3,3,3,3,3,3,3,3,3,3,3,3,4),(-0.140969988491055,
-0.136418201281803,-0.126519129074011,-0.119862943924149,-0.108023198611015,
-0.101287865761346,-0.090139871551597,-0.0833947080504807,-0.0768589146704996,
-0.0729154820906274,-0.0587558950229259,-0.0520363404538416,-0.0380581629180643,
-0.0301338231072477,-0.0233108653882379,-0.00436182509706893,0.),
 .UNSPECIFIED.);
#950=B_SPLINE_CURVE_WITH_KNOTS('',3,(#54275,#54276,#54277,#54278,#54279),
 .UNSPECIFIED.,.F.,.F.,(4,1,4),(14.5207325112001,15.4404644124101,15.7079632679489),
 .UNSPECIFIED.);
#951=B_SPLINE_CURVE_WITH_KNOTS('',3,(#54281,#54282,#54283,#54284,#54285,
#54286,#54287,#54288,#54289,#54290,#54291,#54292,#54293,#54294,#54295,#54296,
#54297,#54298,#54299,#54300,#54301,#54302,#54303,#54304,#54305,#54306,#54307,
#54308,#54309,#54310,#54311,#54312,#54313,#54314,#54315,#54316,#54317,#54318,
#54319,#54320,#54321,#54322,#54323,#54324,#54325,#54326),.UNSPECIFIED.,
 .F.,.F.,(4,3,3,3,3,3,3,3,3,3,3,3,3,3,3,4),(-0.140062757837253,-0.134086502655363,
-0.121471201692539,-0.113407420189978,-0.103769238848968,-0.0940394045173825,
-0.077137458468192,-0.0675091411229651,-0.0624229504780945,-0.0526720783361747,
-0.0459880025256372,-0.0296865588875043,-0.0231241679347418,-0.0164915350738677,
-0.00152742707365775,0.),.UNSPECIFIED.);
#952=B_SPLINE_CURVE_WITH_KNOTS('',3,(#54754,#54755,#54756,#54757,#54758,
#54759,#54760,#54761,#54762,#54763,#54764,#54765,#54766,#54767,#54768,#54769,
#54770,#54771,#54772,#54773,#54774,#54775,#54776,#54777,#54778,#54779,#54780,
#54781,#54782,#54783,#54784,#54785,#54786,#54787,#54788,#54789,#54790,#54791,
#54792,#54793,#54794,#54795,#54796,#54797,#54798,#54799,#54800,#54801,#54802),
 .UNSPECIFIED.,.F.,.F.,(4,3,3,3,3,3,3,3,3,3,3,3,3,3,3,3,4),(-0.140969988491055,
-0.136418201281804,-0.12651913264835,-0.119862947097551,-0.108023216524302,
-0.101287867723297,-0.0901398753013339,-0.0833947302596222,-0.0768589166211874,
-0.0729154820906318,-0.0587558981038184,-0.0520363434544736,-0.0380581662283503,
-0.0301338238248305,-0.0233108669968244,-0.00436182790272715,0.),
 .UNSPECIFIED.);
#953=B_SPLINE_CURVE_WITH_KNOTS('',3,(#54803,#54804,#54805,#54806,#54807,
#54808,#54809,#54810,#54811,#54812),.UNSPECIFIED.,.F.,.F.,(4,3,3,4),(-102.747494138162,
-101.749945651384,-100.752397164606,-100.483683492427),.UNSPECIFIED.);
#954=TOROIDAL_SURFACE('',#25670,1.1,0.1);
#955=TOROIDAL_SURFACE('',#25675,1.1,0.1);
#956=SHAPE_REPRESENTATION_RELATIONSHIP('SRR','None',#55104,#976);
#957=SHAPE_REPRESENTATION_RELATIONSHIP('SRR','None',#55105,#977);
#958=SHAPE_REPRESENTATION_RELATIONSHIP('SRR','None',#55106,#978);
#959=SHAPE_REPRESENTATION_RELATIONSHIP('SRR','None',#55107,#979);
#960=SHAPE_REPRESENTATION_RELATIONSHIP('SRR','None',#55108,#980);
#961=SHAPE_REPRESENTATION_RELATIONSHIP('SRR','None',#55109,#981);
#962=SHAPE_REPRESENTATION_RELATIONSHIP('SRR','None',#55110,#982);
#963=SHAPE_REPRESENTATION_RELATIONSHIP('SRR','None',#55111,#983);
#964=SHAPE_REPRESENTATION_RELATIONSHIP('SRR','None',#55112,#984);
#965=SHAPE_REPRESENTATION_RELATIONSHIP('SRR','None',#55113,#985);
#966=SHAPE_REPRESENTATION_RELATIONSHIP('SRR','None',#55114,#986);
#967=SHAPE_REPRESENTATION_RELATIONSHIP('SRR','None',#55115,#987);
#968=SHAPE_REPRESENTATION_RELATIONSHIP('SRR','None',#55116,#988);
#969=SHAPE_REPRESENTATION_RELATIONSHIP('SRR','None',#55117,#989);
#970=SHAPE_REPRESENTATION_RELATIONSHIP('SRR','None',#55118,#990);
#971=SHAPE_REPRESENTATION_RELATIONSHIP('SRR','None',#55119,#991);
#972=SHAPE_REPRESENTATION_RELATIONSHIP('SRR','None',#55120,#992);
#973=SHAPE_REPRESENTATION_RELATIONSHIP('SRR','None',#55121,#993);
#974=SHAPE_REPRESENTATION_RELATIONSHIP('SRR','None',#55122,#994);
#975=SHAPE_REPRESENTATION_RELATIONSHIP('SRR','None',#55123,#995);
#976=ADVANCED_BREP_SHAPE_REPRESENTATION('',(#1016),#54982);
#977=ADVANCED_BREP_SHAPE_REPRESENTATION('',(#1017),#54983);
#978=ADVANCED_BREP_SHAPE_REPRESENTATION('',(#1018),#54984);
#979=ADVANCED_BREP_SHAPE_REPRESENTATION('',(#1019),#54985);
#980=ADVANCED_BREP_SHAPE_REPRESENTATION('',(#1020),#54986);
#981=ADVANCED_BREP_SHAPE_REPRESENTATION('',(#1021),#54987);
#982=ADVANCED_BREP_SHAPE_REPRESENTATION('',(#1022),#54988);
#983=ADVANCED_BREP_SHAPE_REPRESENTATION('',(#1023),#54989);
#984=ADVANCED_BREP_SHAPE_REPRESENTATION('',(#1024),#54990);
#985=ADVANCED_BREP_SHAPE_REPRESENTATION('',(#1025),#54991);
#986=ADVANCED_BREP_SHAPE_REPRESENTATION('',(#1026),#54992);
#987=ADVANCED_BREP_SHAPE_REPRESENTATION('',(#1027),#54993);
#988=ADVANCED_BREP_SHAPE_REPRESENTATION('',(#1028),#54994);
#989=ADVANCED_BREP_SHAPE_REPRESENTATION('',(#1029),#54995);
#990=ADVANCED_BREP_SHAPE_REPRESENTATION('',(#1030),#54996);
#991=ADVANCED_BREP_SHAPE_REPRESENTATION('',(#1031),#54997);
#992=ADVANCED_BREP_SHAPE_REPRESENTATION('',(#1032),#54998);
#993=ADVANCED_BREP_SHAPE_REPRESENTATION('',(#1033),#54999);
#994=ADVANCED_BREP_SHAPE_REPRESENTATION('',(#1034),#55000);
#995=ADVANCED_BREP_SHAPE_REPRESENTATION('',(#1035),#55001);
#996=STYLED_ITEM('',(#55372),#1016);
#997=STYLED_ITEM('',(#55379),#1017);
#998=STYLED_ITEM('',(#55400),#1018);
#999=STYLED_ITEM('',(#55400),#1019);
#1000=STYLED_ITEM('',(#55379),#1020);
#1001=STYLED_ITEM('',(#55372),#1021);
#1002=STYLED_ITEM('',(#55372),#1022);
#1003=STYLED_ITEM('',(#55372),#1023);
#1004=STYLED_ITEM('',(#55400),#1024);
#1005=STYLED_ITEM('',(#55379),#1025);
#1006=STYLED_ITEM('',(#55379),#1026);
#1007=STYLED_ITEM('',(#55365),#1027);
#1008=STYLED_ITEM('',(#55379),#1028);
#1009=STYLED_ITEM('',(#55393),#1029);
#1010=STYLED_ITEM('',(#55379),#1030);
#1011=STYLED_ITEM('',(#55393),#1031);
#1012=STYLED_ITEM('',(#55393),#1032);
#1013=STYLED_ITEM('',(#55393),#1033);
#1014=STYLED_ITEM('',(#55400),#1034);
#1015=STYLED_ITEM('',(#55400),#1035);
#1016=MANIFOLD_SOLID_BREP('Rear End Cap',#24529);
#1017=MANIFOLD_SOLID_BREP('Enclosure Guard Shield',#24530);
#1018=MANIFOLD_SOLID_BREP('Isogrid Faceplate',#24531);
#1019=MANIFOLD_SOLID_BREP('Beam Port Tube',#24532);
#1020=MANIFOLD_SOLID_BREP('Port Clamp Collar',#24533);
#1021=MANIFOLD_SOLID_BREP('Motor Mount Bulkhead',#24534);
#1022=MANIFOLD_SOLID_BREP('BLDC Motor',#24535);
#1023=MANIFOLD_SOLID_BREP('Hub Clamp Adapter',#24536);
#1024=MANIFOLD_SOLID_BREP('Disc Clamp Ring',#24537);
#1025=MANIFOLD_SOLID_BREP('Chopper Disc',#24538);
#1026=MANIFOLD_SOLID_BREP('Slot Sensor PCB',#24539);
#1027=MANIFOLD_SOLID_BREP('Sensor Bracket',#24540);
#1028=MANIFOLD_SOLID_BREP('Controller Board',#24541);
#1029=MANIFOLD_SOLID_BREP('Set Screw M2x2',#24542);
#1030=MANIFOLD_SOLID_BREP('Hex Standoff',#24543);
#1031=MANIFOLD_SOLID_BREP('ISO_4762_M2x12_A2',#24544);
#1032=MANIFOLD_SOLID_BREP('ISO_4762_M2x10_A2',#24545);
#1033=MANIFOLD_SOLID_BREP('ISO_4762_M2.5x6_A2',#24546);
#1034=MANIFOLD_SOLID_BREP('ISO_7045_M1.6x3_A2',#24547);
#1035=MANIFOLD_SOLID_BREP('ISO_7045_M1.6x6_A2',#24548);
#1036=FACE_BOUND('',#3782,.T.);
#1037=FACE_BOUND('',#3783,.T.);
#1038=FACE_BOUND('',#3784,.T.);
#1039=FACE_BOUND('',#3785,.T.);
#1040=FACE_BOUND('',#3786,.T.);
#1041=FACE_BOUND('',#3787,.T.);
#1042=FACE_BOUND('',#3788,.T.);
#1043=FACE_BOUND('',#3791,.T.);
#1044=FACE_BOUND('',#3792,.T.);
#1045=FACE_BOUND('',#3793,.T.);
#1046=FACE_BOUND('',#3794,.T.);
#1047=FACE_BOUND('',#3795,.T.);
#1048=FACE_BOUND('',#3796,.T.);
#1049=FACE_BOUND('',#3797,.T.);
#1050=FACE_BOUND('',#3806,.T.);
#1051=FACE_BOUND('',#3807,.T.);
#1052=FACE_BOUND('',#3808,.T.);
#1053=FACE_BOUND('',#3809,.T.);
#1054=FACE_BOUND('',#3826,.T.);
#1055=FACE_BOUND('',#3829,.T.);
#1056=FACE_BOUND('',#3844,.T.);
#1057=FACE_BOUND('',#3849,.T.);
#1058=FACE_BOUND('',#3854,.T.);
#1059=FACE_BOUND('',#3859,.T.);
#1060=FACE_BOUND('',#3864,.T.);
#1061=FACE_BOUND('',#3869,.T.);
#1062=FACE_BOUND('',#3929,.T.);
#1063=FACE_BOUND('',#3930,.T.);
#1064=FACE_BOUND('',#3931,.T.);
#1065=FACE_BOUND('',#3932,.T.);
#1066=FACE_BOUND('',#3933,.T.);
#1067=FACE_BOUND('',#3934,.T.);
#1068=FACE_BOUND('',#3935,.T.);
#1069=FACE_BOUND('',#3938,.T.);
#1070=FACE_BOUND('',#3939,.T.);
#1071=FACE_BOUND('',#3940,.T.);
#1072=FACE_BOUND('',#3941,.T.);
#1073=FACE_BOUND('',#3942,.T.);
#1074=FACE_BOUND('',#3943,.T.);
#1075=FACE_BOUND('',#3944,.T.);
#1076=FACE_BOUND('',#3945,.T.);
#1077=FACE_BOUND('',#3946,.T.);
#1078=FACE_BOUND('',#3947,.T.);
#1079=FACE_BOUND('',#3948,.T.);
#1080=FACE_BOUND('',#3949,.T.);
#1081=FACE_BOUND('',#3950,.T.);
#1082=FACE_BOUND('',#3973,.T.);
#1083=FACE_BOUND('',#3979,.T.);
#1084=FACE_BOUND('',#3985,.T.);
#1085=FACE_BOUND('',#3991,.T.);
#1086=FACE_BOUND('',#3997,.T.);
#1087=FACE_BOUND('',#4003,.T.);
#1088=FACE_BOUND('',#4009,.T.);
#1089=FACE_BOUND('',#4015,.T.);
#1090=FACE_BOUND('',#4021,.T.);
#1091=FACE_BOUND('',#4027,.T.);
#1092=FACE_BOUND('',#4033,.T.);
#1093=FACE_BOUND('',#4039,.T.);
#1094=FACE_BOUND('',#4044,.T.);
#1095=FACE_BOUND('',#4045,.T.);
#1096=FACE_BOUND('',#4046,.T.);
#1097=FACE_BOUND('',#4047,.T.);
#1098=FACE_BOUND('',#4050,.T.);
#1099=FACE_BOUND('',#4054,.T.);
#1100=FACE_BOUND('',#4055,.T.);
#1101=FACE_BOUND('',#4056,.T.);
#1102=FACE_BOUND('',#4057,.T.);
#1103=FACE_BOUND('',#4058,.T.);
#1104=FACE_BOUND('',#4059,.T.);
#1105=FACE_BOUND('',#4060,.T.);
#1106=FACE_BOUND('',#4061,.T.);
#1107=FACE_BOUND('',#4062,.T.);
#1108=FACE_BOUND('',#4063,.T.);
#1109=FACE_BOUND('',#4064,.T.);
#1110=FACE_BOUND('',#4065,.T.);
#1111=FACE_BOUND('',#4066,.T.);
#1112=FACE_BOUND('',#4069,.T.);
#1113=FACE_BOUND('',#4070,.T.);
#1114=FACE_BOUND('',#4071,.T.);
#1115=FACE_BOUND('',#4072,.T.);
#1116=FACE_BOUND('',#4073,.T.);
#1117=FACE_BOUND('',#4074,.T.);
#1118=FACE_BOUND('',#4075,.T.);
#1119=FACE_BOUND('',#4076,.T.);
#1120=FACE_BOUND('',#4077,.T.);
#1121=FACE_BOUND('',#4078,.T.);
#1122=FACE_BOUND('',#4079,.T.);
#1123=FACE_BOUND('',#4080,.T.);
#1124=FACE_BOUND('',#4081,.T.);
#1125=FACE_BOUND('',#4082,.T.);
#1126=FACE_BOUND('',#4083,.T.);
#1127=FACE_BOUND('',#4084,.T.);
#1128=FACE_BOUND('',#4085,.T.);
#1129=FACE_BOUND('',#4086,.T.);
#1130=FACE_BOUND('',#4087,.T.);
#1131=FACE_BOUND('',#4088,.T.);
#1132=FACE_BOUND('',#4089,.T.);
#1133=FACE_BOUND('',#4090,.T.);
#1134=FACE_BOUND('',#4091,.T.);
#1135=FACE_BOUND('',#4092,.T.);
#1136=FACE_BOUND('',#4093,.T.);
#1137=FACE_BOUND('',#4094,.T.);
#1138=FACE_BOUND('',#4095,.T.);
#1139=FACE_BOUND('',#4096,.T.);
#1140=FACE_BOUND('',#4097,.T.);
#1141=FACE_BOUND('',#4098,.T.);
#1142=FACE_BOUND('',#4099,.T.);
#1143=FACE_BOUND('',#4100,.T.);
#1144=FACE_BOUND('',#4101,.T.);
#1145=FACE_BOUND('',#4102,.T.);
#1146=FACE_BOUND('',#4103,.T.);
#1147=FACE_BOUND('',#4104,.T.);
#1148=FACE_BOUND('',#4105,.T.);
#1149=FACE_BOUND('',#4106,.T.);
#1150=FACE_BOUND('',#4107,.T.);
#1151=FACE_BOUND('',#4108,.T.);
#1152=FACE_BOUND('',#4109,.T.);
#1153=FACE_BOUND('',#4110,.T.);
#1154=FACE_BOUND('',#4111,.T.);
#1155=FACE_BOUND('',#4112,.T.);
#1156=FACE_BOUND('',#4113,.T.);
#1157=FACE_BOUND('',#4314,.T.);
#1158=FACE_BOUND('',#4320,.T.);
#1159=FACE_BOUND('',#4323,.T.);
#1160=FACE_BOUND('',#4327,.T.);
#1161=FACE_BOUND('',#4334,.T.);
#1162=FACE_BOUND('',#4344,.T.);
#1163=FACE_BOUND('',#4345,.T.);
#1164=FACE_BOUND('',#4346,.T.);
#1165=FACE_BOUND('',#4357,.T.);
#1166=FACE_BOUND('',#4367,.T.);
#1167=FACE_BOUND('',#4372,.T.);
#1168=FACE_BOUND('',#4375,.T.);
#1169=FACE_BOUND('',#4389,.T.);
#1170=FACE_BOUND('',#4390,.T.);
#1171=FACE_BOUND('',#4391,.T.);
#1172=FACE_BOUND('',#4392,.T.);
#1173=FACE_BOUND('',#4393,.T.);
#1174=FACE_BOUND('',#4394,.T.);
#1175=FACE_BOUND('',#4395,.T.);
#1176=FACE_BOUND('',#4396,.T.);
#1177=FACE_BOUND('',#4397,.T.);
#1178=FACE_BOUND('',#4398,.T.);
#1179=FACE_BOUND('',#4401,.T.);
#1180=FACE_BOUND('',#4402,.T.);
#1181=FACE_BOUND('',#4403,.T.);
#1182=FACE_BOUND('',#4404,.T.);
#1183=FACE_BOUND('',#4405,.T.);
#1184=FACE_BOUND('',#4406,.T.);
#1185=FACE_BOUND('',#4407,.T.);
#1186=FACE_BOUND('',#4408,.T.);
#1187=FACE_BOUND('',#4409,.T.);
#1188=FACE_BOUND('',#4410,.T.);
#1189=FACE_BOUND('',#4421,.T.);
#1190=FACE_BOUND('',#4426,.T.);
#1191=FACE_BOUND('',#4428,.T.);
#1192=FACE_BOUND('',#4431,.T.);
#1193=FACE_BOUND('',#4436,.T.);
#1194=FACE_BOUND('',#4437,.T.);
#1195=FACE_BOUND('',#4438,.T.);
#1196=FACE_BOUND('',#4441,.T.);
#1197=FACE_BOUND('',#4447,.T.);
#1198=FACE_BOUND('',#4454,.T.);
#1199=FACE_BOUND('',#4463,.T.);
#1200=FACE_BOUND('',#4464,.T.);
#1201=FACE_BOUND('',#4465,.T.);
#1202=FACE_BOUND('',#4466,.T.);
#1203=FACE_BOUND('',#4469,.T.);
#1204=FACE_BOUND('',#4470,.T.);
#1205=FACE_BOUND('',#4471,.T.);
#1206=FACE_BOUND('',#4472,.T.);
#1207=FACE_BOUND('',#4487,.T.);
#1208=FACE_BOUND('',#4490,.T.);
#1209=FACE_BOUND('',#4491,.T.);
#1210=FACE_BOUND('',#4492,.T.);
#1211=FACE_BOUND('',#4493,.T.);
#1212=FACE_BOUND('',#4510,.T.);
#1213=FACE_BOUND('',#4511,.T.);
#1214=FACE_BOUND('',#4512,.T.);
#1215=FACE_BOUND('',#4513,.T.);
#1216=FACE_BOUND('',#4514,.T.);
#1217=FACE_BOUND('',#4515,.T.);
#1218=FACE_BOUND('',#4516,.T.);
#1219=FACE_BOUND('',#4517,.T.);
#1220=FACE_BOUND('',#4518,.T.);
#1221=FACE_BOUND('',#4519,.T.);
#1222=FACE_BOUND('',#4550,.T.);
#1223=FACE_BOUND('',#4551,.T.);
#1224=FACE_BOUND('',#4552,.T.);
#1225=FACE_BOUND('',#4553,.T.);
#1226=FACE_BOUND('',#4554,.T.);
#1227=FACE_BOUND('',#4555,.T.);
#1228=FACE_BOUND('',#4556,.T.);
#1229=FACE_BOUND('',#4557,.T.);
#1230=FACE_BOUND('',#4558,.T.);
#1231=FACE_BOUND('',#4559,.T.);
#1232=FACE_BOUND('',#4568,.T.);
#1233=FACE_BOUND('',#4573,.T.);
#1234=FACE_BOUND('',#4577,.T.);
#1235=FACE_BOUND('',#4578,.T.);
#1236=FACE_BOUND('',#4579,.T.);
#1237=FACE_BOUND('',#4586,.T.);
#1238=FACE_BOUND('',#4587,.T.);
#1239=FACE_BOUND('',#4618,.T.);
#1240=FACE_BOUND('',#4619,.T.);
#1241=FACE_BOUND('',#4622,.T.);
#1242=FACE_BOUND('',#4623,.T.);
#1243=FACE_BOUND('',#4626,.T.);
#1244=FACE_BOUND('',#4664,.T.);
#1245=FACE_BOUND('',#4665,.T.);
#1246=FACE_BOUND('',#4666,.T.);
#1247=FACE_BOUND('',#4667,.T.);
#1248=FACE_BOUND('',#4670,.T.);
#1249=FACE_BOUND('',#4671,.T.);
#1250=FACE_BOUND('',#4672,.T.);
#1251=FACE_BOUND('',#4673,.T.);
#1252=FACE_BOUND('',#4674,.T.);
#1253=FACE_BOUND('',#4675,.T.);
#1254=FACE_BOUND('',#4676,.T.);
#1255=FACE_BOUND('',#4677,.T.);
#1256=FACE_BOUND('',#4678,.T.);
#1257=FACE_BOUND('',#4679,.T.);
#1258=FACE_BOUND('',#4680,.T.);
#1259=FACE_BOUND('',#4702,.T.);
#1260=FACE_BOUND('',#4707,.T.);
#1261=FACE_BOUND('',#4742,.T.);
#1262=FACE_BOUND('',#4755,.T.);
#1263=FACE_BOUND('',#4936,.T.);
#1264=FACE_BOUND('',#4942,.T.);
#1265=FACE_BOUND('',#4944,.T.);
#1266=FACE_BOUND('',#5115,.T.);
#1267=FACE_BOUND('',#5121,.T.);
#1268=FACE_BOUND('',#5123,.T.);
#1269=FACE_BOUND('',#5272,.T.);
#1270=FACE_BOUND('',#5277,.T.);
#1271=FACE_BOUND('',#5279,.T.);
#1272=FACE_BOUND('',#5306,.T.);
#1273=FACE_BOUND('',#5318,.T.);
#1274=FACE_BOUND('',#5366,.T.);
#1275=FACE_BOUND('',#5377,.T.);
#1276=PLANE('',#24785);
#1277=PLANE('',#24795);
#1278=PLANE('',#24819);
#1279=PLANE('',#24861);
#1280=PLANE('',#24865);
#1281=PLANE('',#24889);
#1282=PLANE('',#24896);
#1283=PLANE('',#24903);
#1284=PLANE('',#24910);
#1285=PLANE('',#24917);
#1286=PLANE('',#24924);
#1287=PLANE('',#25045);
#1288=PLANE('',#25049);
#1289=PLANE('',#25096);
#1290=PLANE('',#25107);
#1291=PLANE('',#25118);
#1292=PLANE('',#25129);
#1293=PLANE('',#25140);
#1294=PLANE('',#25151);
#1295=PLANE('',#25162);
#1296=PLANE('',#25173);
#1297=PLANE('',#25184);
#1298=PLANE('',#25195);
#1299=PLANE('',#25206);
#1300=PLANE('',#25217);
#1301=PLANE('',#25228);
#1302=PLANE('',#25232);
#1303=PLANE('',#25241);
#1304=PLANE('',#25245);
#1305=PLANE('',#25341);
#1306=PLANE('',#25344);
#1307=PLANE('',#25348);
#1308=PLANE('',#25351);
#1309=PLANE('',#25353);
#1310=PLANE('',#25357);
#1311=PLANE('',#25360);
#1312=PLANE('',#25362);
#1313=PLANE('',#25368);
#1314=PLANE('',#25371);
#1315=PLANE('',#25373);
#1316=PLANE('',#25377);
#1317=PLANE('',#25380);
#1318=PLANE('',#25382);
#1319=PLANE('',#25386);
#1320=PLANE('',#25389);
#1321=PLANE('',#25392);
#1322=PLANE('',#25396);
#1323=PLANE('',#25399);
#1324=PLANE('',#25401);
#1325=PLANE('',#25405);
#1326=PLANE('',#25408);
#1327=PLANE('',#25410);
#1328=PLANE('',#25414);
#1329=PLANE('',#25417);
#1330=PLANE('',#25419);
#1331=PLANE('',#25422);
#1332=PLANE('',#25425);
#1333=PLANE('',#25427);
#1334=PLANE('',#25431);
#1335=PLANE('',#25434);
#1336=PLANE('',#25436);
#1337=PLANE('',#25440);
#1338=PLANE('',#25443);
#1339=PLANE('',#25446);
#1340=PLANE('',#25450);
#1341=PLANE('',#25453);
#1342=PLANE('',#25455);
#1343=PLANE('',#25459);
#1344=PLANE('',#25462);
#1345=PLANE('',#25464);
#1346=PLANE('',#25468);
#1347=PLANE('',#25471);
#1348=PLANE('',#25473);
#1349=PLANE('',#25479);
#1350=PLANE('',#25482);
#1351=PLANE('',#25484);
#1352=PLANE('',#25488);
#1353=PLANE('',#25491);
#1354=PLANE('',#25493);
#1355=PLANE('',#25497);
#1356=PLANE('',#25500);
#1357=PLANE('',#25502);
#1358=PLANE('',#25505);
#1359=PLANE('',#25508);
#1360=PLANE('',#25510);
#1361=PLANE('',#25514);
#1362=PLANE('',#25517);
#1363=PLANE('',#25519);
#1364=PLANE('',#25525);
#1365=PLANE('',#25527);
#1366=PLANE('',#25530);
#1367=PLANE('',#25533);
#1368=PLANE('',#25535);
#1369=PLANE('',#25539);
#1370=PLANE('',#25542);
#1371=PLANE('',#25544);
#1372=PLANE('',#25548);
#1373=PLANE('',#25551);
#1374=PLANE('',#25553);
#1375=PLANE('',#25557);
#1376=PLANE('',#25559);
#1377=PLANE('',#25562);
#1378=PLANE('',#25565);
#1379=PLANE('',#25569);
#1380=PLANE('',#25571);
#1381=PLANE('',#25574);
#1382=PLANE('',#25578);
#1383=PLANE('',#25580);
#1384=PLANE('',#25583);
#1385=PLANE('',#25597);
#1386=PLANE('',#25598);
#1387=PLANE('',#25599);
#1388=PLANE('',#25600);
#1389=PLANE('',#25601);
#1390=PLANE('',#25602);
#1391=PLANE('',#25603);
#1392=PLANE('',#25604);
#1393=PLANE('',#25605);
#1394=PLANE('',#25606);
#1395=PLANE('',#25607);
#1396=PLANE('',#25608);
#1397=PLANE('',#25609);
#1398=PLANE('',#25610);
#1399=PLANE('',#25611);
#1400=PLANE('',#25612);
#1401=PLANE('',#25613);
#1402=PLANE('',#25614);
#1403=PLANE('',#25615);
#1404=PLANE('',#25616);
#1405=PLANE('',#25617);
#1406=PLANE('',#25618);
#1407=PLANE('',#25619);
#1408=PLANE('',#25620);
#1409=PLANE('',#25621);
#1410=PLANE('',#25622);
#1411=PLANE('',#25623);
#1412=PLANE('',#25624);
#1413=PLANE('',#25627);
#1414=PLANE('',#25639);
#1415=PLANE('',#25643);
#1416=PLANE('',#25650);
#1417=PLANE('',#25664);
#1418=PLANE('',#25686);
#1419=PLANE('',#25713);
#1420=PLANE('',#25738);
#1421=PLANE('',#25745);
#1422=PLANE('',#25748);
#1423=PLANE('',#25786);
#1424=PLANE('',#25790);
#1425=PLANE('',#25811);
#1426=PLANE('',#25812);
#1427=PLANE('',#25821);
#1428=PLANE('',#25823);
#1429=PLANE('',#25827);
#1430=PLANE('',#25834);
#1431=PLANE('',#25838);
#1432=PLANE('',#25844);
#1433=PLANE('',#25850);
#1434=PLANE('',#25862);
#1435=PLANE('',#25877);
#1436=PLANE('',#25883);
#1437=PLANE('',#25897);
#1438=PLANE('',#25898);
#1439=PLANE('',#25914);
#1440=PLANE('',#25926);
#1441=PLANE('',#25954);
#1442=PLANE('',#25955);
#1443=PLANE('',#25956);
#1444=PLANE('',#25957);
#1445=PLANE('',#25983);
#1446=PLANE('',#25986);
#1447=PLANE('',#25989);
#1448=PLANE('',#25992);
#1449=PLANE('',#25995);
#1450=PLANE('',#25998);
#1451=PLANE('',#26001);
#1452=PLANE('',#26004);
#1453=PLANE('',#26007);
#1454=PLANE('',#26010);
#1455=PLANE('',#26013);
#1456=PLANE('',#26016);
#1457=PLANE('',#26021);
#1458=PLANE('',#26023);
#1459=PLANE('',#26024);
#1460=PLANE('',#26025);
#1461=PLANE('',#26026);
#1462=PLANE('',#26027);
#1463=PLANE('',#26028);
#1464=PLANE('',#26029);
#1465=PLANE('',#26030);
#1466=PLANE('',#26031);
#1467=PLANE('',#26032);
#1468=PLANE('',#26033);
#1469=PLANE('',#26034);
#1470=PLANE('',#26035);
#1471=PLANE('',#26036);
#1472=PLANE('',#26037);
#1473=PLANE('',#26040);
#1474=PLANE('',#26041);
#1475=PLANE('',#26046);
#1476=PLANE('',#26047);
#1477=PLANE('',#26048);
#1478=PLANE('',#26049);
#1479=PLANE('',#26050);
#1480=PLANE('',#26051);
#1481=PLANE('',#26052);
#1482=PLANE('',#26053);
#1483=PLANE('',#26054);
#1484=PLANE('',#26055);
#1485=PLANE('',#26056);
#1486=PLANE('',#26057);
#1487=PLANE('',#26058);
#1488=PLANE('',#26059);
#1489=PLANE('',#26060);
#1490=PLANE('',#26061);
#1491=PLANE('',#26066);
#1492=PLANE('',#26071);
#1493=PLANE('',#26080);
#1494=PLANE('',#26083);
#1495=PLANE('',#26087);
#1496=PLANE('',#26091);
#1497=PLANE('',#26092);
#1498=PLANE('',#26093);
#1499=PLANE('',#26094);
#1500=PLANE('',#26095);
#1501=PLANE('',#26096);
#1502=PLANE('',#26097);
#1503=PLANE('',#26098);
#1504=PLANE('',#26100);
#1505=PLANE('',#26101);
#1506=PLANE('',#26102);
#1507=PLANE('',#26103);
#1508=PLANE('',#26104);
#1509=PLANE('',#26105);
#1510=PLANE('',#26106);
#1511=PLANE('',#26107);
#1512=PLANE('',#26108);
#1513=PLANE('',#26109);
#1514=PLANE('',#26113);
#1515=PLANE('',#26114);
#1516=PLANE('',#26115);
#1517=PLANE('',#26116);
#1518=PLANE('',#26117);
#1519=PLANE('',#26118);
#1520=PLANE('',#26119);
#1521=PLANE('',#26120);
#1522=PLANE('',#26121);
#1523=PLANE('',#26122);
#1524=PLANE('',#26123);
#1525=PLANE('',#26124);
#1526=PLANE('',#26125);
#1527=PLANE('',#26126);
#1528=PLANE('',#26127);
#1529=PLANE('',#26128);
#1530=PLANE('',#26129);
#1531=PLANE('',#26130);
#1532=PLANE('',#26131);
#1533=PLANE('',#26132);
#1534=PLANE('',#26133);
#1535=PLANE('',#26146);
#1536=PLANE('',#26150);
#1537=PLANE('',#26162);
#1538=PLANE('',#26165);
#1539=PLANE('',#26172);
#1540=PLANE('',#26173);
#1541=PLANE('',#26174);
#1542=PLANE('',#26175);
#1543=PLANE('',#26176);
#1544=PLANE('',#26177);
#1545=PLANE('',#26178);
#1546=PLANE('',#26179);
#1547=PLANE('',#26184);
#1548=PLANE('',#26206);
#1549=PLANE('',#26229);
#1550=PLANE('',#26230);
#1551=PLANE('',#26231);
#1552=PLANE('',#26232);
#1553=PLANE('',#26233);
#1554=PLANE('',#26246);
#1555=PLANE('',#26247);
#1556=PLANE('',#26250);
#1557=PLANE('',#26251);
#1558=PLANE('',#26315);
#1559=PLANE('',#26318);
#1560=PLANE('',#26321);
#1561=PLANE('',#26323);
#1562=PLANE('',#26324);
#1563=PLANE('',#26325);
#1564=PLANE('',#26327);
#1565=PLANE('',#26328);
#1566=PLANE('',#26329);
#1567=PLANE('',#26331);
#1568=PLANE('',#26332);
#1569=PLANE('',#26333);
#1570=PLANE('',#26335);
#1571=PLANE('',#26336);
#1572=PLANE('',#26337);
#1573=PLANE('',#26339);
#1574=PLANE('',#26340);
#1575=PLANE('',#26341);
#1576=PLANE('',#26343);
#1577=PLANE('',#26344);
#1578=PLANE('',#26345);
#1579=PLANE('',#26347);
#1580=PLANE('',#26348);
#1581=PLANE('',#26349);
#1582=PLANE('',#26351);
#1583=PLANE('',#26352);
#1584=PLANE('',#26353);
#1585=PLANE('',#26355);
#1586=PLANE('',#26356);
#1587=PLANE('',#26357);
#1588=PLANE('',#26359);
#1589=PLANE('',#26360);
#1590=PLANE('',#26361);
#1591=PLANE('',#26363);
#1592=PLANE('',#26364);
#1593=PLANE('',#26365);
#1594=PLANE('',#26367);
#1595=PLANE('',#26368);
#1596=PLANE('',#26369);
#1597=PLANE('',#26371);
#1598=PLANE('',#26372);
#1599=PLANE('',#26373);
#1600=PLANE('',#26375);
#1601=PLANE('',#26376);
#1602=PLANE('',#26377);
#1603=PLANE('',#26379);
#1604=PLANE('',#26380);
#1605=PLANE('',#26381);
#1606=PLANE('',#26383);
#1607=PLANE('',#26384);
#1608=PLANE('',#26385);
#1609=PLANE('',#26387);
#1610=PLANE('',#26388);
#1611=PLANE('',#26389);
#1612=PLANE('',#26392);
#1613=PLANE('',#26393);
#1614=PLANE('',#26394);
#1615=PLANE('',#26396);
#1616=PLANE('',#26397);
#1617=PLANE('',#26398);
#1618=PLANE('',#26400);
#1619=PLANE('',#26401);
#1620=PLANE('',#26402);
#1621=PLANE('',#26404);
#1622=PLANE('',#26405);
#1623=PLANE('',#26406);
#1624=PLANE('',#26408);
#1625=PLANE('',#26409);
#1626=PLANE('',#26410);
#1627=PLANE('',#26412);
#1628=PLANE('',#26413);
#1629=PLANE('',#26414);
#1630=PLANE('',#26416);
#1631=PLANE('',#26417);
#1632=PLANE('',#26418);
#1633=PLANE('',#26420);
#1634=PLANE('',#26421);
#1635=PLANE('',#26422);
#1636=PLANE('',#26424);
#1637=PLANE('',#26425);
#1638=PLANE('',#26426);
#1639=PLANE('',#26428);
#1640=PLANE('',#26429);
#1641=PLANE('',#26430);
#1642=PLANE('',#26432);
#1643=PLANE('',#26433);
#1644=PLANE('',#26434);
#1645=PLANE('',#26436);
#1646=PLANE('',#26437);
#1647=PLANE('',#26438);
#1648=PLANE('',#26440);
#1649=PLANE('',#26441);
#1650=PLANE('',#26442);
#1651=PLANE('',#26444);
#1652=PLANE('',#26445);
#1653=PLANE('',#26446);
#1654=PLANE('',#26448);
#1655=PLANE('',#26449);
#1656=PLANE('',#26450);
#1657=PLANE('',#26452);
#1658=PLANE('',#26453);
#1659=PLANE('',#26454);
#1660=PLANE('',#26456);
#1661=PLANE('',#26457);
#1662=PLANE('',#26458);
#1663=PLANE('',#26460);
#1664=PLANE('',#26461);
#1665=PLANE('',#26501);
#1666=PLANE('',#26502);
#1667=PLANE('',#26503);
#1668=PLANE('',#26508);
#1669=PLANE('',#26509);
#1670=PLANE('',#26510);
#1671=PLANE('',#26511);
#1672=PLANE('',#26512);
#1673=PLANE('',#26513);
#1674=PLANE('',#26514);
#1675=PLANE('',#26515);
#1676=PLANE('',#26522);
#1677=PLANE('',#26523);
#1678=PLANE('',#26577);
#1679=PLANE('',#26580);
#1680=PLANE('',#26583);
#1681=PLANE('',#26585);
#1682=PLANE('',#26586);
#1683=PLANE('',#26587);
#1684=PLANE('',#26589);
#1685=PLANE('',#26590);
#1686=PLANE('',#26591);
#1687=PLANE('',#26593);
#1688=PLANE('',#26594);
#1689=PLANE('',#26595);
#1690=PLANE('',#26597);
#1691=PLANE('',#26598);
#1692=PLANE('',#26599);
#1693=PLANE('',#26601);
#1694=PLANE('',#26602);
#1695=PLANE('',#26603);
#1696=PLANE('',#26605);
#1697=PLANE('',#26606);
#1698=PLANE('',#26607);
#1699=PLANE('',#26609);
#1700=PLANE('',#26610);
#1701=PLANE('',#26611);
#1702=PLANE('',#26613);
#1703=PLANE('',#26614);
#1704=PLANE('',#26615);
#1705=PLANE('',#26617);
#1706=PLANE('',#26618);
#1707=PLANE('',#26619);
#1708=PLANE('',#26621);
#1709=PLANE('',#26622);
#1710=PLANE('',#26623);
#1711=PLANE('',#26625);
#1712=PLANE('',#26626);
#1713=PLANE('',#26627);
#1714=PLANE('',#26629);
#1715=PLANE('',#26630);
#1716=PLANE('',#26631);
#1717=PLANE('',#26633);
#1718=PLANE('',#26634);
#1719=PLANE('',#26635);
#1720=PLANE('',#26637);
#1721=PLANE('',#26638);
#1722=PLANE('',#26639);
#1723=PLANE('',#26641);
#1724=PLANE('',#26642);
#1725=PLANE('',#26643);
#1726=PLANE('',#26645);
#1727=PLANE('',#26646);
#1728=PLANE('',#26647);
#1729=PLANE('',#26649);
#1730=PLANE('',#26650);
#1731=PLANE('',#26651);
#1732=PLANE('',#26654);
#1733=PLANE('',#26655);
#1734=PLANE('',#26656);
#1735=PLANE('',#26658);
#1736=PLANE('',#26659);
#1737=PLANE('',#26660);
#1738=PLANE('',#26662);
#1739=PLANE('',#26663);
#1740=PLANE('',#26664);
#1741=PLANE('',#26666);
#1742=PLANE('',#26667);
#1743=PLANE('',#26668);
#1744=PLANE('',#26670);
#1745=PLANE('',#26671);
#1746=PLANE('',#26672);
#1747=PLANE('',#26674);
#1748=PLANE('',#26675);
#1749=PLANE('',#26676);
#1750=PLANE('',#26678);
#1751=PLANE('',#26679);
#1752=PLANE('',#26680);
#1753=PLANE('',#26682);
#1754=PLANE('',#26683);
#1755=PLANE('',#26684);
#1756=PLANE('',#26686);
#1757=PLANE('',#26687);
#1758=PLANE('',#26688);
#1759=PLANE('',#26690);
#1760=PLANE('',#26691);
#1761=PLANE('',#26692);
#1762=PLANE('',#26694);
#1763=PLANE('',#26695);
#1764=PLANE('',#26696);
#1765=PLANE('',#26698);
#1766=PLANE('',#26699);
#1767=PLANE('',#26700);
#1768=PLANE('',#26702);
#1769=PLANE('',#26703);
#1770=PLANE('',#26704);
#1771=PLANE('',#26706);
#1772=PLANE('',#26707);
#1773=PLANE('',#26708);
#1774=PLANE('',#26710);
#1775=PLANE('',#26711);
#1776=PLANE('',#26712);
#1777=PLANE('',#26714);
#1778=PLANE('',#26715);
#1779=PLANE('',#26716);
#1780=PLANE('',#26718);
#1781=PLANE('',#26719);
#1782=PLANE('',#26720);
#1783=PLANE('',#26722);
#1784=PLANE('',#26723);
#1785=PLANE('',#26763);
#1786=PLANE('',#26764);
#1787=PLANE('',#26765);
#1788=PLANE('',#26770);
#1789=PLANE('',#26771);
#1790=PLANE('',#26772);
#1791=PLANE('',#26773);
#1792=PLANE('',#26774);
#1793=PLANE('',#26775);
#1794=PLANE('',#26776);
#1795=PLANE('',#26777);
#1796=PLANE('',#26784);
#1797=PLANE('',#26785);
#1798=PLANE('',#26816);
#1799=PLANE('',#26819);
#1800=PLANE('',#26824);
#1801=PLANE('',#26826);
#1802=PLANE('',#26827);
#1803=PLANE('',#26828);
#1804=PLANE('',#26830);
#1805=PLANE('',#26831);
#1806=PLANE('',#26832);
#1807=PLANE('',#26834);
#1808=PLANE('',#26835);
#1809=PLANE('',#26836);
#1810=PLANE('',#26838);
#1811=PLANE('',#26839);
#1812=PLANE('',#26840);
#1813=PLANE('',#26842);
#1814=PLANE('',#26843);
#1815=PLANE('',#26844);
#1816=PLANE('',#26846);
#1817=PLANE('',#26847);
#1818=PLANE('',#26848);
#1819=PLANE('',#26850);
#1820=PLANE('',#26851);
#1821=PLANE('',#26852);
#1822=PLANE('',#26854);
#1823=PLANE('',#26855);
#1824=PLANE('',#26856);
#1825=PLANE('',#26858);
#1826=PLANE('',#26859);
#1827=PLANE('',#26860);
#1828=PLANE('',#26862);
#1829=PLANE('',#26863);
#1830=PLANE('',#26864);
#1831=PLANE('',#26866);
#1832=PLANE('',#26867);
#1833=PLANE('',#26868);
#1834=PLANE('',#26870);
#1835=PLANE('',#26871);
#1836=PLANE('',#26872);
#1837=PLANE('',#26874);
#1838=PLANE('',#26875);
#1839=PLANE('',#26876);
#1840=PLANE('',#26878);
#1841=PLANE('',#26879);
#1842=PLANE('',#26880);
#1843=PLANE('',#26882);
#1844=PLANE('',#26883);
#1845=PLANE('',#26884);
#1846=PLANE('',#26886);
#1847=PLANE('',#26887);
#1848=PLANE('',#26888);
#1849=PLANE('',#26890);
#1850=PLANE('',#26891);
#1851=PLANE('',#26892);
#1852=PLANE('',#26895);
#1853=PLANE('',#26896);
#1854=PLANE('',#26897);
#1855=PLANE('',#26899);
#1856=PLANE('',#26900);
#1857=PLANE('',#26901);
#1858=PLANE('',#26903);
#1859=PLANE('',#26904);
#1860=PLANE('',#26905);
#1861=PLANE('',#26907);
#1862=PLANE('',#26908);
#1863=PLANE('',#26909);
#1864=PLANE('',#26911);
#1865=PLANE('',#26912);
#1866=PLANE('',#26913);
#1867=PLANE('',#26915);
#1868=PLANE('',#26916);
#1869=PLANE('',#26917);
#1870=PLANE('',#26919);
#1871=PLANE('',#26920);
#1872=PLANE('',#26921);
#1873=PLANE('',#26923);
#1874=PLANE('',#26924);
#1875=PLANE('',#26925);
#1876=PLANE('',#26927);
#1877=PLANE('',#26928);
#1878=PLANE('',#26929);
#1879=PLANE('',#26931);
#1880=PLANE('',#26932);
#1881=PLANE('',#26933);
#1882=PLANE('',#26935);
#1883=PLANE('',#26936);
#1884=PLANE('',#26937);
#1885=PLANE('',#26939);
#1886=PLANE('',#26940);
#1887=PLANE('',#26941);
#1888=PLANE('',#26943);
#1889=PLANE('',#26944);
#1890=PLANE('',#26945);
#1891=PLANE('',#26947);
#1892=PLANE('',#26948);
#1893=PLANE('',#26949);
#1894=PLANE('',#26951);
#1895=PLANE('',#26952);
#1896=PLANE('',#26953);
#1897=PLANE('',#26955);
#1898=PLANE('',#26956);
#1899=PLANE('',#26957);
#1900=PLANE('',#26959);
#1901=PLANE('',#26960);
#1902=PLANE('',#26961);
#1903=PLANE('',#26963);
#1904=PLANE('',#26964);
#1905=PLANE('',#27004);
#1906=PLANE('',#27005);
#1907=PLANE('',#27006);
#1908=PLANE('',#27011);
#1909=PLANE('',#27012);
#1910=PLANE('',#27013);
#1911=PLANE('',#27014);
#1912=PLANE('',#27015);
#1913=PLANE('',#27016);
#1914=PLANE('',#27017);
#1915=PLANE('',#27018);
#1916=PLANE('',#27023);
#1917=PLANE('',#27024);
#1918=PLANE('',#27046);
#1919=PLANE('',#27049);
#1920=PLANE('',#27050);
#1921=PLANE('',#27051);
#1922=PLANE('',#27052);
#1923=PLANE('',#27053);
#1924=PLANE('',#27054);
#1925=PLANE('',#27055);
#1926=PLANE('',#27057);
#1927=PLANE('',#27058);
#1928=PLANE('',#27059);
#1929=PLANE('',#27060);
#1930=PLANE('',#27061);
#1931=PLANE('',#27062);
#1932=PLANE('',#27063);
#1933=PLANE('',#27064);
#1934=PLANE('',#27069);
#1935=PLANE('',#27114);
#1936=PLANE('',#27119);
#1937=PLANE('',#27120);
#1938=PLANE('',#27121);
#1939=PLANE('',#27122);
#1940=PLANE('',#27123);
#1941=PLANE('',#27124);
#1942=PLANE('',#27125);
#1943=PLANE('',#27127);
#1944=PLANE('',#27128);
#1945=PLANE('',#27129);
#1946=PLANE('',#27130);
#1947=PLANE('',#27131);
#1948=PLANE('',#27132);
#1949=PLANE('',#27133);
#1950=PLANE('',#27134);
#1951=PLANE('',#27137);
#1952=CYLINDRICAL_SURFACE('',#24778,4.75);
#1953=CYLINDRICAL_SURFACE('',#24810,0.7);
#1954=CYLINDRICAL_SURFACE('',#24827,0.21);
#1955=CYLINDRICAL_SURFACE('',#24832,0.21);
#1956=CYLINDRICAL_SURFACE('',#24837,0.21);
#1957=CYLINDRICAL_SURFACE('',#24842,0.21);
#1958=CYLINDRICAL_SURFACE('',#24847,0.21);
#1959=CYLINDRICAL_SURFACE('',#24852,0.21);
#1960=CYLINDRICAL_SURFACE('',#24857,4.75);
#1961=CYLINDRICAL_SURFACE('',#24867,4.66);
#1962=CYLINDRICAL_SURFACE('',#24870,0.13);
#1963=CYLINDRICAL_SURFACE('',#24875,0.13);
#1964=CYLINDRICAL_SURFACE('',#24880,0.13);
#1965=CYLINDRICAL_SURFACE('',#24885,0.12);
#1966=CYLINDRICAL_SURFACE('',#24892,0.12);
#1967=CYLINDRICAL_SURFACE('',#24899,0.12);
#1968=CYLINDRICAL_SURFACE('',#24906,0.12);
#1969=CYLINDRICAL_SURFACE('',#24913,0.12);
#1970=CYLINDRICAL_SURFACE('',#24920,0.12);
#1971=CYLINDRICAL_SURFACE('',#24928,4.095);
#1972=CYLINDRICAL_SURFACE('',#24932,0.105);
#1973=CYLINDRICAL_SURFACE('',#24938,0.105);
#1974=CYLINDRICAL_SURFACE('',#24944,0.105);
#1975=CYLINDRICAL_SURFACE('',#24950,0.105);
#1976=CYLINDRICAL_SURFACE('',#24956,0.105);
#1977=CYLINDRICAL_SURFACE('',#24962,0.105);
#1978=CYLINDRICAL_SURFACE('',#24968,0.105);
#1979=CYLINDRICAL_SURFACE('',#24974,0.105);
#1980=CYLINDRICAL_SURFACE('',#24980,0.105);
#1981=CYLINDRICAL_SURFACE('',#24986,0.105);
#1982=CYLINDRICAL_SURFACE('',#24992,0.105);
#1983=CYLINDRICAL_SURFACE('',#24998,0.105);
#1984=CYLINDRICAL_SURFACE('',#25004,0.105);
#1985=CYLINDRICAL_SURFACE('',#25010,0.105);
#1986=CYLINDRICAL_SURFACE('',#25016,0.105);
#1987=CYLINDRICAL_SURFACE('',#25022,0.105);
#1988=CYLINDRICAL_SURFACE('',#25028,0.105);
#1989=CYLINDRICAL_SURFACE('',#25034,0.105);
#1990=CYLINDRICAL_SURFACE('',#25042,4.1);
#1991=CYLINDRICAL_SURFACE('',#25054,4.6);
#1992=CYLINDRICAL_SURFACE('',#25061,0.105);
#1993=CYLINDRICAL_SURFACE('',#25067,0.105);
#1994=CYLINDRICAL_SURFACE('',#25073,0.13);
#1995=CYLINDRICAL_SURFACE('',#25079,0.13);
#1996=CYLINDRICAL_SURFACE('',#25085,0.13);
#1997=CYLINDRICAL_SURFACE('',#25092,0.12);
#1998=CYLINDRICAL_SURFACE('',#25098,0.21);
#1999=CYLINDRICAL_SURFACE('',#25103,0.12);
#2000=CYLINDRICAL_SURFACE('',#25109,0.21);
#2001=CYLINDRICAL_SURFACE('',#25114,0.12);
#2002=CYLINDRICAL_SURFACE('',#25120,0.21);
#2003=CYLINDRICAL_SURFACE('',#25125,0.12);
#2004=CYLINDRICAL_SURFACE('',#25131,0.21);
#2005=CYLINDRICAL_SURFACE('',#25136,0.12);
#2006=CYLINDRICAL_SURFACE('',#25142,0.21);
#2007=CYLINDRICAL_SURFACE('',#25147,0.120000000000001);
#2008=CYLINDRICAL_SURFACE('',#25153,0.21);
#2009=CYLINDRICAL_SURFACE('',#25158,0.12);
#2010=CYLINDRICAL_SURFACE('',#25164,0.21);
#2011=CYLINDRICAL_SURFACE('',#25169,0.12);
#2012=CYLINDRICAL_SURFACE('',#25175,0.21);
#2013=CYLINDRICAL_SURFACE('',#25180,0.12);
#2014=CYLINDRICAL_SURFACE('',#25186,0.21);
#2015=CYLINDRICAL_SURFACE('',#25191,0.12);
#2016=CYLINDRICAL_SURFACE('',#25197,0.21);
#2017=CYLINDRICAL_SURFACE('',#25202,0.12);
#2018=CYLINDRICAL_SURFACE('',#25208,0.21);
#2019=CYLINDRICAL_SURFACE('',#25213,0.12);
#2020=CYLINDRICAL_SURFACE('',#25219,0.21);
#2021=CYLINDRICAL_SURFACE('',#25225,0.7);
#2022=CYLINDRICAL_SURFACE('',#25238,4.6);
#2023=CYLINDRICAL_SURFACE('',#25337,0.12);
#2024=CYLINDRICAL_SURFACE('',#25339,0.12);
#2025=CYLINDRICAL_SURFACE('',#25342,0.12);
#2026=CYLINDRICAL_SURFACE('',#25346,0.12);
#2027=CYLINDRICAL_SURFACE('',#25349,0.12);
#2028=CYLINDRICAL_SURFACE('',#25354,0.12);
#2029=CYLINDRICAL_SURFACE('',#25355,0.12);
#2030=CYLINDRICAL_SURFACE('',#25358,0.12);
#2031=CYLINDRICAL_SURFACE('',#25363,0.12);
#2032=CYLINDRICAL_SURFACE('',#25364,0.12);
#2033=CYLINDRICAL_SURFACE('',#25366,0.12);
#2034=CYLINDRICAL_SURFACE('',#25369,0.12);
#2035=CYLINDRICAL_SURFACE('',#25374,0.12);
#2036=CYLINDRICAL_SURFACE('',#25375,0.12);
#2037=CYLINDRICAL_SURFACE('',#25378,0.12);
#2038=CYLINDRICAL_SURFACE('',#25383,0.12);
#2039=CYLINDRICAL_SURFACE('',#25384,0.12);
#2040=CYLINDRICAL_SURFACE('',#25387,0.12);
#2041=CYLINDRICAL_SURFACE('',#25393,0.12);
#2042=CYLINDRICAL_SURFACE('',#25394,0.12);
#2043=CYLINDRICAL_SURFACE('',#25397,0.12);
#2044=CYLINDRICAL_SURFACE('',#25402,0.12);
#2045=CYLINDRICAL_SURFACE('',#25403,0.12);
#2046=CYLINDRICAL_SURFACE('',#25406,0.12);
#2047=CYLINDRICAL_SURFACE('',#25411,0.12);
#2048=CYLINDRICAL_SURFACE('',#25412,0.12);
#2049=CYLINDRICAL_SURFACE('',#25418,0.12);
#2050=CYLINDRICAL_SURFACE('',#25420,0.12);
#2051=CYLINDRICAL_SURFACE('',#25423,0.12);
#2052=CYLINDRICAL_SURFACE('',#25428,0.12);
#2053=CYLINDRICAL_SURFACE('',#25429,0.12);
#2054=CYLINDRICAL_SURFACE('',#25432,0.12);
#2055=CYLINDRICAL_SURFACE('',#25437,0.12);
#2056=CYLINDRICAL_SURFACE('',#25438,0.12);
#2057=CYLINDRICAL_SURFACE('',#25441,0.12);
#2058=CYLINDRICAL_SURFACE('',#25447,0.12);
#2059=CYLINDRICAL_SURFACE('',#25448,0.12);
#2060=CYLINDRICAL_SURFACE('',#25451,0.12);
#2061=CYLINDRICAL_SURFACE('',#25456,0.12);
#2062=CYLINDRICAL_SURFACE('',#25457,0.12);
#2063=CYLINDRICAL_SURFACE('',#25460,0.12);
#2064=CYLINDRICAL_SURFACE('',#25465,0.12);
#2065=CYLINDRICAL_SURFACE('',#25466,0.12);
#2066=CYLINDRICAL_SURFACE('',#25469,0.12);
#2067=CYLINDRICAL_SURFACE('',#25474,0.12);
#2068=CYLINDRICAL_SURFACE('',#25475,0.12);
#2069=CYLINDRICAL_SURFACE('',#25477,0.12);
#2070=CYLINDRICAL_SURFACE('',#25480,0.12);
#2071=CYLINDRICAL_SURFACE('',#25485,0.12);
#2072=CYLINDRICAL_SURFACE('',#25486,0.12);
#2073=CYLINDRICAL_SURFACE('',#25489,0.12);
#2074=CYLINDRICAL_SURFACE('',#25494,0.12);
#2075=CYLINDRICAL_SURFACE('',#25495,0.12);
#2076=CYLINDRICAL_SURFACE('',#25501,0.12);
#2077=CYLINDRICAL_SURFACE('',#25503,0.12);
#2078=CYLINDRICAL_SURFACE('',#25506,0.12);
#2079=CYLINDRICAL_SURFACE('',#25511,0.12);
#2080=CYLINDRICAL_SURFACE('',#25512,0.12);
#2081=CYLINDRICAL_SURFACE('',#25515,0.12);
#2082=CYLINDRICAL_SURFACE('',#25520,0.12);
#2083=CYLINDRICAL_SURFACE('',#25521,0.12);
#2084=CYLINDRICAL_SURFACE('',#25523,0.12);
#2085=CYLINDRICAL_SURFACE('',#25528,0.12);
#2086=CYLINDRICAL_SURFACE('',#25531,0.12);
#2087=CYLINDRICAL_SURFACE('',#25536,0.12);
#2088=CYLINDRICAL_SURFACE('',#25537,0.12);
#2089=CYLINDRICAL_SURFACE('',#25540,0.12);
#2090=CYLINDRICAL_SURFACE('',#25545,0.12);
#2091=CYLINDRICAL_SURFACE('',#25546,0.12);
#2092=CYLINDRICAL_SURFACE('',#25549,0.12);
#2093=CYLINDRICAL_SURFACE('',#25554,0.12);
#2094=CYLINDRICAL_SURFACE('',#25555,0.12);
#2095=CYLINDRICAL_SURFACE('',#25560,0.12);
#2096=CYLINDRICAL_SURFACE('',#25563,0.12);
#2097=CYLINDRICAL_SURFACE('',#25567,0.12);
#2098=CYLINDRICAL_SURFACE('',#25572,0.12);
#2099=CYLINDRICAL_SURFACE('',#25576,0.12);
#2100=CYLINDRICAL_SURFACE('',#25581,0.12);
#2101=CYLINDRICAL_SURFACE('',#25585,4.);
#2102=CYLINDRICAL_SURFACE('',#25586,4.);
#2103=CYLINDRICAL_SURFACE('',#25587,4.);
#2104=CYLINDRICAL_SURFACE('',#25588,4.);
#2105=CYLINDRICAL_SURFACE('',#25589,4.);
#2106=CYLINDRICAL_SURFACE('',#25590,4.);
#2107=CYLINDRICAL_SURFACE('',#25591,4.);
#2108=CYLINDRICAL_SURFACE('',#25592,4.);
#2109=CYLINDRICAL_SURFACE('',#25593,4.);
#2110=CYLINDRICAL_SURFACE('',#25594,4.);
#2111=CYLINDRICAL_SURFACE('',#25595,4.);
#2112=CYLINDRICAL_SURFACE('',#25596,4.);
#2113=CYLINDRICAL_SURFACE('',#25625,3.8);
#2114=CYLINDRICAL_SURFACE('',#25629,4.095);
#2115=CYLINDRICAL_SURFACE('',#25630,0.9025);
#2116=CYLINDRICAL_SURFACE('',#25636,1.05);
#2117=CYLINDRICAL_SURFACE('',#25655,0.6);
#2118=CYLINDRICAL_SURFACE('',#25669,0.9);
#2119=CYLINDRICAL_SURFACE('',#25673,1.2);
#2120=CYLINDRICAL_SURFACE('',#25680,0.9);
#2121=CYLINDRICAL_SURFACE('',#25690,1.065);
#2122=CYLINDRICAL_SURFACE('',#25699,1.55);
#2123=CYLINDRICAL_SURFACE('',#25710,0.91);
#2124=CYLINDRICAL_SURFACE('',#25723,0.21);
#2125=CYLINDRICAL_SURFACE('',#25730,0.21);
#2126=CYLINDRICAL_SURFACE('',#25734,0.12);
#2127=CYLINDRICAL_SURFACE('',#25741,0.12);
#2128=CYLINDRICAL_SURFACE('',#25750,0.45);
#2129=CYLINDRICAL_SURFACE('',#25753,0.45);
#2130=CYLINDRICAL_SURFACE('',#25756,0.13);
#2131=CYLINDRICAL_SURFACE('',#25761,0.145);
#2132=CYLINDRICAL_SURFACE('',#25764,0.145);
#2133=CYLINDRICAL_SURFACE('',#25767,0.145);
#2134=CYLINDRICAL_SURFACE('',#25770,0.0950000000000001);
#2135=CYLINDRICAL_SURFACE('',#25773,0.095);
#2136=CYLINDRICAL_SURFACE('',#25776,0.305);
#2137=CYLINDRICAL_SURFACE('',#25783,0.8);
#2138=CYLINDRICAL_SURFACE('',#25795,4.);
#2139=CYLINDRICAL_SURFACE('',#25802,0.085);
#2140=CYLINDRICAL_SURFACE('',#25806,0.085);
#2141=CYLINDRICAL_SURFACE('',#25808,0.14);
#2142=CYLINDRICAL_SURFACE('',#25816,0.54);
#2143=CYLINDRICAL_SURFACE('',#25818,0.78);
#2144=CYLINDRICAL_SURFACE('',#25825,0.8);
#2145=CYLINDRICAL_SURFACE('',#25831,0.8);
#2146=CYLINDRICAL_SURFACE('',#25836,0.3);
#2147=CYLINDRICAL_SURFACE('',#25840,0.1);
#2148=CYLINDRICAL_SURFACE('',#25852,0.2);
#2149=CYLINDRICAL_SURFACE('',#25857,0.1);
#2150=CYLINDRICAL_SURFACE('',#25864,0.4);
#2151=CYLINDRICAL_SURFACE('',#25868,0.105);
#2152=CYLINDRICAL_SURFACE('',#25875,0.085);
#2153=CYLINDRICAL_SURFACE('',#25889,0.085);
#2154=CYLINDRICAL_SURFACE('',#25894,0.085);
#2155=CYLINDRICAL_SURFACE('',#25902,0.7);
#2156=CYLINDRICAL_SURFACE('',#25911,0.2025);
#2157=CYLINDRICAL_SURFACE('',#25934,0.7);
#2158=CYLINDRICAL_SURFACE('',#25939,0.09);
#2159=CYLINDRICAL_SURFACE('',#25944,0.09);
#2160=CYLINDRICAL_SURFACE('',#25949,0.09);
#2161=CYLINDRICAL_SURFACE('',#25975,2.35);
#2162=CYLINDRICAL_SURFACE('',#25977,0.09);
#2163=CYLINDRICAL_SURFACE('',#25979,0.09);
#2164=CYLINDRICAL_SURFACE('',#25981,0.0900000000000001);
#2165=CYLINDRICAL_SURFACE('',#25984,1.1);
#2166=CYLINDRICAL_SURFACE('',#25987,2.15);
#2167=CYLINDRICAL_SURFACE('',#25990,1.1);
#2168=CYLINDRICAL_SURFACE('',#25993,2.15);
#2169=CYLINDRICAL_SURFACE('',#25996,1.1);
#2170=CYLINDRICAL_SURFACE('',#25999,2.15);
#2171=CYLINDRICAL_SURFACE('',#26002,1.1);
#2172=CYLINDRICAL_SURFACE('',#26005,2.15);
#2173=CYLINDRICAL_SURFACE('',#26008,1.1);
#2174=CYLINDRICAL_SURFACE('',#26011,2.15);
#2175=CYLINDRICAL_SURFACE('',#26014,1.1);
#2176=CYLINDRICAL_SURFACE('',#26017,2.15);
#2177=CYLINDRICAL_SURFACE('',#26019,0.2025);
#2178=CYLINDRICAL_SURFACE('',#26042,0.0900000000000001);
#2179=CYLINDRICAL_SURFACE('',#26044,0.09);
#2180=CYLINDRICAL_SURFACE('',#26063,0.15);
#2181=CYLINDRICAL_SURFACE('',#26072,0.15);
#2182=CYLINDRICAL_SURFACE('',#26074,0.085);
#2183=CYLINDRICAL_SURFACE('',#26077,0.085);
#2184=CYLINDRICAL_SURFACE('',#26081,0.145);
#2185=CYLINDRICAL_SURFACE('',#26084,0.145);
#2186=CYLINDRICAL_SURFACE('',#26088,0.06);
#2187=CYLINDRICAL_SURFACE('',#26110,0.3);
#2188=CYLINDRICAL_SURFACE('',#26134,0.135);
#2189=CYLINDRICAL_SURFACE('',#26137,0.135);
#2190=CYLINDRICAL_SURFACE('',#26140,0.135);
#2191=CYLINDRICAL_SURFACE('',#26143,0.8);
#2192=CYLINDRICAL_SURFACE('',#26148,3.8);
#2193=CYLINDRICAL_SURFACE('',#26152,0.096675);
#2194=CYLINDRICAL_SURFACE('',#26155,0.096675);
#2195=CYLINDRICAL_SURFACE('',#26156,0.096675);
#2196=CYLINDRICAL_SURFACE('',#26157,0.0739);
#2197=CYLINDRICAL_SURFACE('',#26159,0.0739);
#2198=CYLINDRICAL_SURFACE('',#26160,0.0739);
#2199=CYLINDRICAL_SURFACE('',#26161,0.0739);
#2200=CYLINDRICAL_SURFACE('',#26167,0.0739);
#2201=CYLINDRICAL_SURFACE('',#26168,0.096675);
#2202=CYLINDRICAL_SURFACE('',#26186,0.1215);
#2203=CYLINDRICAL_SURFACE('',#26190,0.1215);
#2204=CYLINDRICAL_SURFACE('',#26191,0.1215);
#2205=CYLINDRICAL_SURFACE('',#26192,0.1215);
#2206=CYLINDRICAL_SURFACE('',#26193,0.1215);
#2207=CYLINDRICAL_SURFACE('',#26194,0.1215);
#2208=CYLINDRICAL_SURFACE('',#26195,0.1215);
#2209=CYLINDRICAL_SURFACE('',#26196,0.1215);
#2210=CYLINDRICAL_SURFACE('',#26197,0.095825);
#2211=CYLINDRICAL_SURFACE('',#26199,0.095825);
#2212=CYLINDRICAL_SURFACE('',#26200,0.095825);
#2213=CYLINDRICAL_SURFACE('',#26201,0.095825);
#2214=CYLINDRICAL_SURFACE('',#26202,0.095825);
#2215=CYLINDRICAL_SURFACE('',#26203,0.095825);
#2216=CYLINDRICAL_SURFACE('',#26204,0.095825);
#2217=CYLINDRICAL_SURFACE('',#26205,0.095825);
#2218=CYLINDRICAL_SURFACE('',#26208,0.095825);
#2219=CYLINDRICAL_SURFACE('',#26209,0.1215);
#2220=CYLINDRICAL_SURFACE('',#26213,0.13);
#2221=CYLINDRICAL_SURFACE('',#26253,0.096675);
#2222=CYLINDRICAL_SURFACE('',#26257,0.096675);
#2223=CYLINDRICAL_SURFACE('',#26258,0.096675);
#2224=CYLINDRICAL_SURFACE('',#26259,0.096675);
#2225=CYLINDRICAL_SURFACE('',#26260,0.096675);
#2226=CYLINDRICAL_SURFACE('',#26261,0.096675);
#2227=CYLINDRICAL_SURFACE('',#26262,0.096675);
#2228=CYLINDRICAL_SURFACE('',#26263,0.096675);
#2229=CYLINDRICAL_SURFACE('',#26264,0.096675);
#2230=CYLINDRICAL_SURFACE('',#26265,0.096675);
#2231=CYLINDRICAL_SURFACE('',#26266,0.096675);
#2232=CYLINDRICAL_SURFACE('',#26267,0.096675);
#2233=CYLINDRICAL_SURFACE('',#26268,0.096675);
#2234=CYLINDRICAL_SURFACE('',#26269,0.096675);
#2235=CYLINDRICAL_SURFACE('',#26270,0.096675);
#2236=CYLINDRICAL_SURFACE('',#26271,0.096675);
#2237=CYLINDRICAL_SURFACE('',#26272,0.096675);
#2238=CYLINDRICAL_SURFACE('',#26273,0.096675);
#2239=CYLINDRICAL_SURFACE('',#26274,0.096675);
#2240=CYLINDRICAL_SURFACE('',#26275,0.096675);
#2241=CYLINDRICAL_SURFACE('',#26276,0.096675);
#2242=CYLINDRICAL_SURFACE('',#26277,0.096675);
#2243=CYLINDRICAL_SURFACE('',#26278,0.096675);
#2244=CYLINDRICAL_SURFACE('',#26279,0.096675);
#2245=CYLINDRICAL_SURFACE('',#26280,0.096675);
#2246=CYLINDRICAL_SURFACE('',#26281,0.096675);
#2247=CYLINDRICAL_SURFACE('',#26282,0.096675);
#2248=CYLINDRICAL_SURFACE('',#26283,0.096675);
#2249=CYLINDRICAL_SURFACE('',#26284,0.0739);
#2250=CYLINDRICAL_SURFACE('',#26286,0.0739);
#2251=CYLINDRICAL_SURFACE('',#26287,0.0739);
#2252=CYLINDRICAL_SURFACE('',#26288,0.0739);
#2253=CYLINDRICAL_SURFACE('',#26289,0.0739);
#2254=CYLINDRICAL_SURFACE('',#26290,0.0739);
#2255=CYLINDRICAL_SURFACE('',#26291,0.0739);
#2256=CYLINDRICAL_SURFACE('',#26292,0.0739);
#2257=CYLINDRICAL_SURFACE('',#26293,0.0739);
#2258=CYLINDRICAL_SURFACE('',#26294,0.0739);
#2259=CYLINDRICAL_SURFACE('',#26295,0.0739);
#2260=CYLINDRICAL_SURFACE('',#26296,0.0739);
#2261=CYLINDRICAL_SURFACE('',#26297,0.0739);
#2262=CYLINDRICAL_SURFACE('',#26298,0.0739);
#2263=CYLINDRICAL_SURFACE('',#26299,0.0739);
#2264=CYLINDRICAL_SURFACE('',#26300,0.0739);
#2265=CYLINDRICAL_SURFACE('',#26301,0.0739);
#2266=CYLINDRICAL_SURFACE('',#26302,0.0739);
#2267=CYLINDRICAL_SURFACE('',#26303,0.0739);
#2268=CYLINDRICAL_SURFACE('',#26304,0.0739);
#2269=CYLINDRICAL_SURFACE('',#26305,0.0739);
#2270=CYLINDRICAL_SURFACE('',#26306,0.0739);
#2271=CYLINDRICAL_SURFACE('',#26307,0.0739);
#2272=CYLINDRICAL_SURFACE('',#26308,0.0739);
#2273=CYLINDRICAL_SURFACE('',#26309,0.0739);
#2274=CYLINDRICAL_SURFACE('',#26310,0.0739);
#2275=CYLINDRICAL_SURFACE('',#26311,0.0739);
#2276=CYLINDRICAL_SURFACE('',#26312,0.0739);
#2277=CYLINDRICAL_SURFACE('',#26313,0.0739);
#2278=CYLINDRICAL_SURFACE('',#26320,0.0739);
#2279=CYLINDRICAL_SURFACE('',#26462,0.19);
#2280=CYLINDRICAL_SURFACE('',#26518,0.096675);
#2281=CYLINDRICAL_SURFACE('',#26525,0.096675);
#2282=CYLINDRICAL_SURFACE('',#26529,0.096675);
#2283=CYLINDRICAL_SURFACE('',#26530,0.096675);
#2284=CYLINDRICAL_SURFACE('',#26531,0.096675);
#2285=CYLINDRICAL_SURFACE('',#26532,0.096675);
#2286=CYLINDRICAL_SURFACE('',#26533,0.096675);
#2287=CYLINDRICAL_SURFACE('',#26534,0.096675);
#2288=CYLINDRICAL_SURFACE('',#26535,0.096675);
#2289=CYLINDRICAL_SURFACE('',#26536,0.096675);
#2290=CYLINDRICAL_SURFACE('',#26537,0.096675);
#2291=CYLINDRICAL_SURFACE('',#26538,0.096675);
#2292=CYLINDRICAL_SURFACE('',#26539,0.096675);
#2293=CYLINDRICAL_SURFACE('',#26540,0.096675);
#2294=CYLINDRICAL_SURFACE('',#26541,0.096675);
#2295=CYLINDRICAL_SURFACE('',#26542,0.096675);
#2296=CYLINDRICAL_SURFACE('',#26543,0.096675);
#2297=CYLINDRICAL_SURFACE('',#26544,0.096675);
#2298=CYLINDRICAL_SURFACE('',#26545,0.096675);
#2299=CYLINDRICAL_SURFACE('',#26546,0.096675);
#2300=CYLINDRICAL_SURFACE('',#26547,0.096675);
#2301=CYLINDRICAL_SURFACE('',#26548,0.096675);
#2302=CYLINDRICAL_SURFACE('',#26549,0.096675);
#2303=CYLINDRICAL_SURFACE('',#26550,0.096675);
#2304=CYLINDRICAL_SURFACE('',#26551,0.0739);
#2305=CYLINDRICAL_SURFACE('',#26553,0.0739);
#2306=CYLINDRICAL_SURFACE('',#26554,0.0739);
#2307=CYLINDRICAL_SURFACE('',#26555,0.0739);
#2308=CYLINDRICAL_SURFACE('',#26556,0.0739);
#2309=CYLINDRICAL_SURFACE('',#26557,0.0739);
#2310=CYLINDRICAL_SURFACE('',#26558,0.0739);
#2311=CYLINDRICAL_SURFACE('',#26559,0.0739);
#2312=CYLINDRICAL_SURFACE('',#26560,0.0739);
#2313=CYLINDRICAL_SURFACE('',#26561,0.0739);
#2314=CYLINDRICAL_SURFACE('',#26562,0.0739);
#2315=CYLINDRICAL_SURFACE('',#26563,0.0739);
#2316=CYLINDRICAL_SURFACE('',#26564,0.0739);
#2317=CYLINDRICAL_SURFACE('',#26565,0.0739);
#2318=CYLINDRICAL_SURFACE('',#26566,0.0739);
#2319=CYLINDRICAL_SURFACE('',#26567,0.0739);
#2320=CYLINDRICAL_SURFACE('',#26568,0.0739);
#2321=CYLINDRICAL_SURFACE('',#26569,0.0739);
#2322=CYLINDRICAL_SURFACE('',#26570,0.0739);
#2323=CYLINDRICAL_SURFACE('',#26571,0.0739);
#2324=CYLINDRICAL_SURFACE('',#26572,0.0739);
#2325=CYLINDRICAL_SURFACE('',#26573,0.0739);
#2326=CYLINDRICAL_SURFACE('',#26574,0.0739);
#2327=CYLINDRICAL_SURFACE('',#26575,0.0739);
#2328=CYLINDRICAL_SURFACE('',#26582,0.0739);
#2329=CYLINDRICAL_SURFACE('',#26724,0.19);
#2330=CYLINDRICAL_SURFACE('',#26780,0.096675);
#2331=CYLINDRICAL_SURFACE('',#26787,0.1215);
#2332=CYLINDRICAL_SURFACE('',#26791,0.1215);
#2333=CYLINDRICAL_SURFACE('',#26792,0.1215);
#2334=CYLINDRICAL_SURFACE('',#26793,0.1215);
#2335=CYLINDRICAL_SURFACE('',#26794,0.1215);
#2336=CYLINDRICAL_SURFACE('',#26795,0.1215);
#2337=CYLINDRICAL_SURFACE('',#26796,0.1215);
#2338=CYLINDRICAL_SURFACE('',#26797,0.1215);
#2339=CYLINDRICAL_SURFACE('',#26798,0.1215);
#2340=CYLINDRICAL_SURFACE('',#26799,0.1215);
#2341=CYLINDRICAL_SURFACE('',#26800,0.1215);
#2342=CYLINDRICAL_SURFACE('',#26801,0.1215);
#2343=CYLINDRICAL_SURFACE('',#26802,0.095825);
#2344=CYLINDRICAL_SURFACE('',#26804,0.095825);
#2345=CYLINDRICAL_SURFACE('',#26805,0.095825);
#2346=CYLINDRICAL_SURFACE('',#26806,0.095825);
#2347=CYLINDRICAL_SURFACE('',#26807,0.095825);
#2348=CYLINDRICAL_SURFACE('',#26808,0.095825);
#2349=CYLINDRICAL_SURFACE('',#26809,0.095825);
#2350=CYLINDRICAL_SURFACE('',#26810,0.095825);
#2351=CYLINDRICAL_SURFACE('',#26811,0.095825);
#2352=CYLINDRICAL_SURFACE('',#26812,0.095825);
#2353=CYLINDRICAL_SURFACE('',#26813,0.095825);
#2354=CYLINDRICAL_SURFACE('',#26814,0.095825);
#2355=CYLINDRICAL_SURFACE('',#26821,0.095825);
#2356=CYLINDRICAL_SURFACE('',#26822,0.1215);
#2357=CYLINDRICAL_SURFACE('',#26965,0.225);
#2358=CYLINDRICAL_SURFACE('',#27026,0.076925);
#2359=CYLINDRICAL_SURFACE('',#27030,0.076925);
#2360=CYLINDRICAL_SURFACE('',#27031,0.076925);
#2361=CYLINDRICAL_SURFACE('',#27032,0.076925);
#2362=CYLINDRICAL_SURFACE('',#27033,0.076925);
#2363=CYLINDRICAL_SURFACE('',#27034,0.076925);
#2364=CYLINDRICAL_SURFACE('',#27035,0.076925);
#2365=CYLINDRICAL_SURFACE('',#27036,0.056925);
#2366=CYLINDRICAL_SURFACE('',#27038,0.056925);
#2367=CYLINDRICAL_SURFACE('',#27039,0.056925);
#2368=CYLINDRICAL_SURFACE('',#27040,0.056925);
#2369=CYLINDRICAL_SURFACE('',#27041,0.056925);
#2370=CYLINDRICAL_SURFACE('',#27042,0.056925);
#2371=CYLINDRICAL_SURFACE('',#27043,0.056925);
#2372=CYLINDRICAL_SURFACE('',#27044,0.056925);
#2373=CYLINDRICAL_SURFACE('',#27048,0.056925);
#2374=CYLINDRICAL_SURFACE('',#27067,0.076925);
#2375=CYLINDRICAL_SURFACE('',#27071,0.16);
#2376=CYLINDRICAL_SURFACE('',#27075,0.076925);
#2377=CYLINDRICAL_SURFACE('',#27079,0.076925);
#2378=CYLINDRICAL_SURFACE('',#27080,0.076925);
#2379=CYLINDRICAL_SURFACE('',#27081,0.076925);
#2380=CYLINDRICAL_SURFACE('',#27082,0.076925);
#2381=CYLINDRICAL_SURFACE('',#27083,0.076925);
#2382=CYLINDRICAL_SURFACE('',#27084,0.076925);
#2383=CYLINDRICAL_SURFACE('',#27085,0.076925);
#2384=CYLINDRICAL_SURFACE('',#27086,0.076925);
#2385=CYLINDRICAL_SURFACE('',#27087,0.076925);
#2386=CYLINDRICAL_SURFACE('',#27088,0.076925);
#2387=CYLINDRICAL_SURFACE('',#27089,0.076925);
#2388=CYLINDRICAL_SURFACE('',#27090,0.076925);
#2389=CYLINDRICAL_SURFACE('',#27091,0.076925);
#2390=CYLINDRICAL_SURFACE('',#27092,0.076925);
#2391=CYLINDRICAL_SURFACE('',#27093,0.076925);
#2392=CYLINDRICAL_SURFACE('',#27094,0.056925);
#2393=CYLINDRICAL_SURFACE('',#27096,0.056925);
#2394=CYLINDRICAL_SURFACE('',#27098,0.056925);
#2395=CYLINDRICAL_SURFACE('',#27099,0.056925);
#2396=CYLINDRICAL_SURFACE('',#27100,0.056925);
#2397=CYLINDRICAL_SURFACE('',#27101,0.056925);
#2398=CYLINDRICAL_SURFACE('',#27102,0.056925);
#2399=CYLINDRICAL_SURFACE('',#27103,0.056925);
#2400=CYLINDRICAL_SURFACE('',#27104,0.056925);
#2401=CYLINDRICAL_SURFACE('',#27105,0.056925);
#2402=CYLINDRICAL_SURFACE('',#27106,0.056925);
#2403=CYLINDRICAL_SURFACE('',#27107,0.056925);
#2404=CYLINDRICAL_SURFACE('',#27108,0.056925);
#2405=CYLINDRICAL_SURFACE('',#27109,0.056925);
#2406=CYLINDRICAL_SURFACE('',#27110,0.056925);
#2407=CYLINDRICAL_SURFACE('',#27111,0.056925);
#2408=CYLINDRICAL_SURFACE('',#27112,0.056925);
#2409=CYLINDRICAL_SURFACE('',#27116,0.056925);
#2410=CYLINDRICAL_SURFACE('',#27117,0.076925);
#2411=CYLINDRICAL_SURFACE('',#27139,0.16);
#2412=FACE_OUTER_BOUND('',#3776,.T.);
#2413=FACE_OUTER_BOUND('',#3777,.T.);
#2414=FACE_OUTER_BOUND('',#3778,.T.);
#2415=FACE_OUTER_BOUND('',#3779,.T.);
#2416=FACE_OUTER_BOUND('',#3780,.T.);
#2417=FACE_OUTER_BOUND('',#3781,.T.);
#2418=FACE_OUTER_BOUND('',#3789,.T.);
#2419=FACE_OUTER_BOUND('',#3790,.T.);
#2420=FACE_OUTER_BOUND('',#3798,.T.);
#2421=FACE_OUTER_BOUND('',#3799,.T.);
#2422=FACE_OUTER_BOUND('',#3800,.T.);
#2423=FACE_OUTER_BOUND('',#3801,.T.);
#2424=FACE_OUTER_BOUND('',#3802,.T.);
#2425=FACE_OUTER_BOUND('',#3803,.T.);
#2426=FACE_OUTER_BOUND('',#3804,.T.);
#2427=FACE_OUTER_BOUND('',#3805,.T.);
#2428=FACE_OUTER_BOUND('',#3810,.T.);
#2429=FACE_OUTER_BOUND('',#3811,.T.);
#2430=FACE_OUTER_BOUND('',#3812,.T.);
#2431=FACE_OUTER_BOUND('',#3813,.T.);
#2432=FACE_OUTER_BOUND('',#3814,.T.);
#2433=FACE_OUTER_BOUND('',#3815,.T.);
#2434=FACE_OUTER_BOUND('',#3816,.T.);
#2435=FACE_OUTER_BOUND('',#3817,.T.);
#2436=FACE_OUTER_BOUND('',#3818,.T.);
#2437=FACE_OUTER_BOUND('',#3819,.T.);
#2438=FACE_OUTER_BOUND('',#3820,.T.);
#2439=FACE_OUTER_BOUND('',#3821,.T.);
#2440=FACE_OUTER_BOUND('',#3822,.T.);
#2441=FACE_OUTER_BOUND('',#3823,.T.);
#2442=FACE_OUTER_BOUND('',#3824,.T.);
#2443=FACE_OUTER_BOUND('',#3825,.T.);
#2444=FACE_OUTER_BOUND('',#3827,.T.);
#2445=FACE_OUTER_BOUND('',#3828,.T.);
#2446=FACE_OUTER_BOUND('',#3830,.T.);
#2447=FACE_OUTER_BOUND('',#3831,.T.);
#2448=FACE_OUTER_BOUND('',#3832,.T.);
#2449=FACE_OUTER_BOUND('',#3833,.T.);
#2450=FACE_OUTER_BOUND('',#3834,.T.);
#2451=FACE_OUTER_BOUND('',#3835,.T.);
#2452=FACE_OUTER_BOUND('',#3836,.T.);
#2453=FACE_OUTER_BOUND('',#3837,.T.);
#2454=FACE_OUTER_BOUND('',#3838,.T.);
#2455=FACE_OUTER_BOUND('',#3839,.T.);
#2456=FACE_OUTER_BOUND('',#3840,.T.);
#2457=FACE_OUTER_BOUND('',#3841,.T.);
#2458=FACE_OUTER_BOUND('',#3842,.T.);
#2459=FACE_OUTER_BOUND('',#3843,.T.);
#2460=FACE_OUTER_BOUND('',#3845,.T.);
#2461=FACE_OUTER_BOUND('',#3846,.T.);
#2462=FACE_OUTER_BOUND('',#3847,.T.);
#2463=FACE_OUTER_BOUND('',#3848,.T.);
#2464=FACE_OUTER_BOUND('',#3850,.T.);
#2465=FACE_OUTER_BOUND('',#3851,.T.);
#2466=FACE_OUTER_BOUND('',#3852,.T.);
#2467=FACE_OUTER_BOUND('',#3853,.T.);
#2468=FACE_OUTER_BOUND('',#3855,.T.);
#2469=FACE_OUTER_BOUND('',#3856,.T.);
#2470=FACE_OUTER_BOUND('',#3857,.T.);
#2471=FACE_OUTER_BOUND('',#3858,.T.);
#2472=FACE_OUTER_BOUND('',#3860,.T.);
#2473=FACE_OUTER_BOUND('',#3861,.T.);
#2474=FACE_OUTER_BOUND('',#3862,.T.);
#2475=FACE_OUTER_BOUND('',#3863,.T.);
#2476=FACE_OUTER_BOUND('',#3865,.T.);
#2477=FACE_OUTER_BOUND('',#3866,.T.);
#2478=FACE_OUTER_BOUND('',#3867,.T.);
#2479=FACE_OUTER_BOUND('',#3868,.T.);
#2480=FACE_OUTER_BOUND('',#3870,.T.);
#2481=FACE_OUTER_BOUND('',#3871,.T.);
#2482=FACE_OUTER_BOUND('',#3872,.T.);
#2483=FACE_OUTER_BOUND('',#3873,.T.);
#2484=FACE_OUTER_BOUND('',#3874,.T.);
#2485=FACE_OUTER_BOUND('',#3875,.T.);
#2486=FACE_OUTER_BOUND('',#3876,.T.);
#2487=FACE_OUTER_BOUND('',#3877,.T.);
#2488=FACE_OUTER_BOUND('',#3878,.T.);
#2489=FACE_OUTER_BOUND('',#3879,.T.);
#2490=FACE_OUTER_BOUND('',#3880,.T.);
#2491=FACE_OUTER_BOUND('',#3881,.T.);
#2492=FACE_OUTER_BOUND('',#3882,.T.);
#2493=FACE_OUTER_BOUND('',#3883,.T.);
#2494=FACE_OUTER_BOUND('',#3884,.T.);
#2495=FACE_OUTER_BOUND('',#3885,.T.);
#2496=FACE_OUTER_BOUND('',#3886,.T.);
#2497=FACE_OUTER_BOUND('',#3887,.T.);
#2498=FACE_OUTER_BOUND('',#3888,.T.);
#2499=FACE_OUTER_BOUND('',#3889,.T.);
#2500=FACE_OUTER_BOUND('',#3890,.T.);
#2501=FACE_OUTER_BOUND('',#3891,.T.);
#2502=FACE_OUTER_BOUND('',#3892,.T.);
#2503=FACE_OUTER_BOUND('',#3893,.T.);
#2504=FACE_OUTER_BOUND('',#3894,.T.);
#2505=FACE_OUTER_BOUND('',#3895,.T.);
#2506=FACE_OUTER_BOUND('',#3896,.T.);
#2507=FACE_OUTER_BOUND('',#3897,.T.);
#2508=FACE_OUTER_BOUND('',#3898,.T.);
#2509=FACE_OUTER_BOUND('',#3899,.T.);
#2510=FACE_OUTER_BOUND('',#3900,.T.);
#2511=FACE_OUTER_BOUND('',#3901,.T.);
#2512=FACE_OUTER_BOUND('',#3902,.T.);
#2513=FACE_OUTER_BOUND('',#3903,.T.);
#2514=FACE_OUTER_BOUND('',#3904,.T.);
#2515=FACE_OUTER_BOUND('',#3905,.T.);
#2516=FACE_OUTER_BOUND('',#3906,.T.);
#2517=FACE_OUTER_BOUND('',#3907,.T.);
#2518=FACE_OUTER_BOUND('',#3908,.T.);
#2519=FACE_OUTER_BOUND('',#3909,.T.);
#2520=FACE_OUTER_BOUND('',#3910,.T.);
#2521=FACE_OUTER_BOUND('',#3911,.T.);
#2522=FACE_OUTER_BOUND('',#3912,.T.);
#2523=FACE_OUTER_BOUND('',#3913,.T.);
#2524=FACE_OUTER_BOUND('',#3914,.T.);
#2525=FACE_OUTER_BOUND('',#3915,.T.);
#2526=FACE_OUTER_BOUND('',#3916,.T.);
#2527=FACE_OUTER_BOUND('',#3917,.T.);
#2528=FACE_OUTER_BOUND('',#3918,.T.);
#2529=FACE_OUTER_BOUND('',#3919,.T.);
#2530=FACE_OUTER_BOUND('',#3920,.T.);
#2531=FACE_OUTER_BOUND('',#3921,.T.);
#2532=FACE_OUTER_BOUND('',#3922,.T.);
#2533=FACE_OUTER_BOUND('',#3923,.T.);
#2534=FACE_OUTER_BOUND('',#3924,.T.);
#2535=FACE_OUTER_BOUND('',#3925,.T.);
#2536=FACE_OUTER_BOUND('',#3926,.T.);
#2537=FACE_OUTER_BOUND('',#3927,.T.);
#2538=FACE_OUTER_BOUND('',#3928,.T.);
#2539=FACE_OUTER_BOUND('',#3936,.T.);
#2540=FACE_OUTER_BOUND('',#3937,.T.);
#2541=FACE_OUTER_BOUND('',#3951,.T.);
#2542=FACE_OUTER_BOUND('',#3952,.T.);
#2543=FACE_OUTER_BOUND('',#3953,.T.);
#2544=FACE_OUTER_BOUND('',#3954,.T.);
#2545=FACE_OUTER_BOUND('',#3955,.T.);
#2546=FACE_OUTER_BOUND('',#3956,.T.);
#2547=FACE_OUTER_BOUND('',#3957,.T.);
#2548=FACE_OUTER_BOUND('',#3958,.T.);
#2549=FACE_OUTER_BOUND('',#3959,.T.);
#2550=FACE_OUTER_BOUND('',#3960,.T.);
#2551=FACE_OUTER_BOUND('',#3961,.T.);
#2552=FACE_OUTER_BOUND('',#3962,.T.);
#2553=FACE_OUTER_BOUND('',#3963,.T.);
#2554=FACE_OUTER_BOUND('',#3964,.T.);
#2555=FACE_OUTER_BOUND('',#3965,.T.);
#2556=FACE_OUTER_BOUND('',#3966,.T.);
#2557=FACE_OUTER_BOUND('',#3967,.T.);
#2558=FACE_OUTER_BOUND('',#3968,.T.);
#2559=FACE_OUTER_BOUND('',#3969,.T.);
#2560=FACE_OUTER_BOUND('',#3970,.T.);
#2561=FACE_OUTER_BOUND('',#3971,.T.);
#2562=FACE_OUTER_BOUND('',#3972,.T.);
#2563=FACE_OUTER_BOUND('',#3974,.T.);
#2564=FACE_OUTER_BOUND('',#3975,.T.);
#2565=FACE_OUTER_BOUND('',#3976,.T.);
#2566=FACE_OUTER_BOUND('',#3977,.T.);
#2567=FACE_OUTER_BOUND('',#3978,.T.);
#2568=FACE_OUTER_BOUND('',#3980,.T.);
#2569=FACE_OUTER_BOUND('',#3981,.T.);
#2570=FACE_OUTER_BOUND('',#3982,.T.);
#2571=FACE_OUTER_BOUND('',#3983,.T.);
#2572=FACE_OUTER_BOUND('',#3984,.T.);
#2573=FACE_OUTER_BOUND('',#3986,.T.);
#2574=FACE_OUTER_BOUND('',#3987,.T.);
#2575=FACE_OUTER_BOUND('',#3988,.T.);
#2576=FACE_OUTER_BOUND('',#3989,.T.);
#2577=FACE_OUTER_BOUND('',#3990,.T.);
#2578=FACE_OUTER_BOUND('',#3992,.T.);
#2579=FACE_OUTER_BOUND('',#3993,.T.);
#2580=FACE_OUTER_BOUND('',#3994,.T.);
#2581=FACE_OUTER_BOUND('',#3995,.T.);
#2582=FACE_OUTER_BOUND('',#3996,.T.);
#2583=FACE_OUTER_BOUND('',#3998,.T.);
#2584=FACE_OUTER_BOUND('',#3999,.T.);
#2585=FACE_OUTER_BOUND('',#4000,.T.);
#2586=FACE_OUTER_BOUND('',#4001,.T.);
#2587=FACE_OUTER_BOUND('',#4002,.T.);
#2588=FACE_OUTER_BOUND('',#4004,.T.);
#2589=FACE_OUTER_BOUND('',#4005,.T.);
#2590=FACE_OUTER_BOUND('',#4006,.T.);
#2591=FACE_OUTER_BOUND('',#4007,.T.);
#2592=FACE_OUTER_BOUND('',#4008,.T.);
#2593=FACE_OUTER_BOUND('',#4010,.T.);
#2594=FACE_OUTER_BOUND('',#4011,.T.);
#2595=FACE_OUTER_BOUND('',#4012,.T.);
#2596=FACE_OUTER_BOUND('',#4013,.T.);
#2597=FACE_OUTER_BOUND('',#4014,.T.);
#2598=FACE_OUTER_BOUND('',#4016,.T.);
#2599=FACE_OUTER_BOUND('',#4017,.T.);
#2600=FACE_OUTER_BOUND('',#4018,.T.);
#2601=FACE_OUTER_BOUND('',#4019,.T.);
#2602=FACE_OUTER_BOUND('',#4020,.T.);
#2603=FACE_OUTER_BOUND('',#4022,.T.);
#2604=FACE_OUTER_BOUND('',#4023,.T.);
#2605=FACE_OUTER_BOUND('',#4024,.T.);
#2606=FACE_OUTER_BOUND('',#4025,.T.);
#2607=FACE_OUTER_BOUND('',#4026,.T.);
#2608=FACE_OUTER_BOUND('',#4028,.T.);
#2609=FACE_OUTER_BOUND('',#4029,.T.);
#2610=FACE_OUTER_BOUND('',#4030,.T.);
#2611=FACE_OUTER_BOUND('',#4031,.T.);
#2612=FACE_OUTER_BOUND('',#4032,.T.);
#2613=FACE_OUTER_BOUND('',#4034,.T.);
#2614=FACE_OUTER_BOUND('',#4035,.T.);
#2615=FACE_OUTER_BOUND('',#4036,.T.);
#2616=FACE_OUTER_BOUND('',#4037,.T.);
#2617=FACE_OUTER_BOUND('',#4038,.T.);
#2618=FACE_OUTER_BOUND('',#4040,.T.);
#2619=FACE_OUTER_BOUND('',#4041,.T.);
#2620=FACE_OUTER_BOUND('',#4042,.T.);
#2621=FACE_OUTER_BOUND('',#4043,.T.);
#2622=FACE_OUTER_BOUND('',#4048,.T.);
#2623=FACE_OUTER_BOUND('',#4049,.T.);
#2624=FACE_OUTER_BOUND('',#4051,.T.);
#2625=FACE_OUTER_BOUND('',#4052,.T.);
#2626=FACE_OUTER_BOUND('',#4053,.T.);
#2627=FACE_OUTER_BOUND('',#4067,.T.);
#2628=FACE_OUTER_BOUND('',#4068,.T.);
#2629=FACE_OUTER_BOUND('',#4114,.T.);
#2630=FACE_OUTER_BOUND('',#4115,.T.);
#2631=FACE_OUTER_BOUND('',#4116,.T.);
#2632=FACE_OUTER_BOUND('',#4117,.T.);
#2633=FACE_OUTER_BOUND('',#4118,.T.);
#2634=FACE_OUTER_BOUND('',#4119,.T.);
#2635=FACE_OUTER_BOUND('',#4120,.T.);
#2636=FACE_OUTER_BOUND('',#4121,.T.);
#2637=FACE_OUTER_BOUND('',#4122,.T.);
#2638=FACE_OUTER_BOUND('',#4123,.T.);
#2639=FACE_OUTER_BOUND('',#4124,.T.);
#2640=FACE_OUTER_BOUND('',#4125,.T.);
#2641=FACE_OUTER_BOUND('',#4126,.T.);
#2642=FACE_OUTER_BOUND('',#4127,.T.);
#2643=FACE_OUTER_BOUND('',#4128,.T.);
#2644=FACE_OUTER_BOUND('',#4129,.T.);
#2645=FACE_OUTER_BOUND('',#4130,.T.);
#2646=FACE_OUTER_BOUND('',#4131,.T.);
#2647=FACE_OUTER_BOUND('',#4132,.T.);
#2648=FACE_OUTER_BOUND('',#4133,.T.);
#2649=FACE_OUTER_BOUND('',#4134,.T.);
#2650=FACE_OUTER_BOUND('',#4135,.T.);
#2651=FACE_OUTER_BOUND('',#4136,.T.);
#2652=FACE_OUTER_BOUND('',#4137,.T.);
#2653=FACE_OUTER_BOUND('',#4138,.T.);
#2654=FACE_OUTER_BOUND('',#4139,.T.);
#2655=FACE_OUTER_BOUND('',#4140,.T.);
#2656=FACE_OUTER_BOUND('',#4141,.T.);
#2657=FACE_OUTER_BOUND('',#4142,.T.);
#2658=FACE_OUTER_BOUND('',#4143,.T.);
#2659=FACE_OUTER_BOUND('',#4144,.T.);
#2660=FACE_OUTER_BOUND('',#4145,.T.);
#2661=FACE_OUTER_BOUND('',#4146,.T.);
#2662=FACE_OUTER_BOUND('',#4147,.T.);
#2663=FACE_OUTER_BOUND('',#4148,.T.);
#2664=FACE_OUTER_BOUND('',#4149,.T.);
#2665=FACE_OUTER_BOUND('',#4150,.T.);
#2666=FACE_OUTER_BOUND('',#4151,.T.);
#2667=FACE_OUTER_BOUND('',#4152,.T.);
#2668=FACE_OUTER_BOUND('',#4153,.T.);
#2669=FACE_OUTER_BOUND('',#4154,.T.);
#2670=FACE_OUTER_BOUND('',#4155,.T.);
#2671=FACE_OUTER_BOUND('',#4156,.T.);
#2672=FACE_OUTER_BOUND('',#4157,.T.);
#2673=FACE_OUTER_BOUND('',#4158,.T.);
#2674=FACE_OUTER_BOUND('',#4159,.T.);
#2675=FACE_OUTER_BOUND('',#4160,.T.);
#2676=FACE_OUTER_BOUND('',#4161,.T.);
#2677=FACE_OUTER_BOUND('',#4162,.T.);
#2678=FACE_OUTER_BOUND('',#4163,.T.);
#2679=FACE_OUTER_BOUND('',#4164,.T.);
#2680=FACE_OUTER_BOUND('',#4165,.T.);
#2681=FACE_OUTER_BOUND('',#4166,.T.);
#2682=FACE_OUTER_BOUND('',#4167,.T.);
#2683=FACE_OUTER_BOUND('',#4168,.T.);
#2684=FACE_OUTER_BOUND('',#4169,.T.);
#2685=FACE_OUTER_BOUND('',#4170,.T.);
#2686=FACE_OUTER_BOUND('',#4171,.T.);
#2687=FACE_OUTER_BOUND('',#4172,.T.);
#2688=FACE_OUTER_BOUND('',#4173,.T.);
#2689=FACE_OUTER_BOUND('',#4174,.T.);
#2690=FACE_OUTER_BOUND('',#4175,.T.);
#2691=FACE_OUTER_BOUND('',#4176,.T.);
#2692=FACE_OUTER_BOUND('',#4177,.T.);
#2693=FACE_OUTER_BOUND('',#4178,.T.);
#2694=FACE_OUTER_BOUND('',#4179,.T.);
#2695=FACE_OUTER_BOUND('',#4180,.T.);
#2696=FACE_OUTER_BOUND('',#4181,.T.);
#2697=FACE_OUTER_BOUND('',#4182,.T.);
#2698=FACE_OUTER_BOUND('',#4183,.T.);
#2699=FACE_OUTER_BOUND('',#4184,.T.);
#2700=FACE_OUTER_BOUND('',#4185,.T.);
#2701=FACE_OUTER_BOUND('',#4186,.T.);
#2702=FACE_OUTER_BOUND('',#4187,.T.);
#2703=FACE_OUTER_BOUND('',#4188,.T.);
#2704=FACE_OUTER_BOUND('',#4189,.T.);
#2705=FACE_OUTER_BOUND('',#4190,.T.);
#2706=FACE_OUTER_BOUND('',#4191,.T.);
#2707=FACE_OUTER_BOUND('',#4192,.T.);
#2708=FACE_OUTER_BOUND('',#4193,.T.);
#2709=FACE_OUTER_BOUND('',#4194,.T.);
#2710=FACE_OUTER_BOUND('',#4195,.T.);
#2711=FACE_OUTER_BOUND('',#4196,.T.);
#2712=FACE_OUTER_BOUND('',#4197,.T.);
#2713=FACE_OUTER_BOUND('',#4198,.T.);
#2714=FACE_OUTER_BOUND('',#4199,.T.);
#2715=FACE_OUTER_BOUND('',#4200,.T.);
#2716=FACE_OUTER_BOUND('',#4201,.T.);
#2717=FACE_OUTER_BOUND('',#4202,.T.);
#2718=FACE_OUTER_BOUND('',#4203,.T.);
#2719=FACE_OUTER_BOUND('',#4204,.T.);
#2720=FACE_OUTER_BOUND('',#4205,.T.);
#2721=FACE_OUTER_BOUND('',#4206,.T.);
#2722=FACE_OUTER_BOUND('',#4207,.T.);
#2723=FACE_OUTER_BOUND('',#4208,.T.);
#2724=FACE_OUTER_BOUND('',#4209,.T.);
#2725=FACE_OUTER_BOUND('',#4210,.T.);
#2726=FACE_OUTER_BOUND('',#4211,.T.);
#2727=FACE_OUTER_BOUND('',#4212,.T.);
#2728=FACE_OUTER_BOUND('',#4213,.T.);
#2729=FACE_OUTER_BOUND('',#4214,.T.);
#2730=FACE_OUTER_BOUND('',#4215,.T.);
#2731=FACE_OUTER_BOUND('',#4216,.T.);
#2732=FACE_OUTER_BOUND('',#4217,.T.);
#2733=FACE_OUTER_BOUND('',#4218,.T.);
#2734=FACE_OUTER_BOUND('',#4219,.T.);
#2735=FACE_OUTER_BOUND('',#4220,.T.);
#2736=FACE_OUTER_BOUND('',#4221,.T.);
#2737=FACE_OUTER_BOUND('',#4222,.T.);
#2738=FACE_OUTER_BOUND('',#4223,.T.);
#2739=FACE_OUTER_BOUND('',#4224,.T.);
#2740=FACE_OUTER_BOUND('',#4225,.T.);
#2741=FACE_OUTER_BOUND('',#4226,.T.);
#2742=FACE_OUTER_BOUND('',#4227,.T.);
#2743=FACE_OUTER_BOUND('',#4228,.T.);
#2744=FACE_OUTER_BOUND('',#4229,.T.);
#2745=FACE_OUTER_BOUND('',#4230,.T.);
#2746=FACE_OUTER_BOUND('',#4231,.T.);
#2747=FACE_OUTER_BOUND('',#4232,.T.);
#2748=FACE_OUTER_BOUND('',#4233,.T.);
#2749=FACE_OUTER_BOUND('',#4234,.T.);
#2750=FACE_OUTER_BOUND('',#4235,.T.);
#2751=FACE_OUTER_BOUND('',#4236,.T.);
#2752=FACE_OUTER_BOUND('',#4237,.T.);
#2753=FACE_OUTER_BOUND('',#4238,.T.);
#2754=FACE_OUTER_BOUND('',#4239,.T.);
#2755=FACE_OUTER_BOUND('',#4240,.T.);
#2756=FACE_OUTER_BOUND('',#4241,.T.);
#2757=FACE_OUTER_BOUND('',#4242,.T.);
#2758=FACE_OUTER_BOUND('',#4243,.T.);
#2759=FACE_OUTER_BOUND('',#4244,.T.);
#2760=FACE_OUTER_BOUND('',#4245,.T.);
#2761=FACE_OUTER_BOUND('',#4246,.T.);
#2762=FACE_OUTER_BOUND('',#4247,.T.);
#2763=FACE_OUTER_BOUND('',#4248,.T.);
#2764=FACE_OUTER_BOUND('',#4249,.T.);
#2765=FACE_OUTER_BOUND('',#4250,.T.);
#2766=FACE_OUTER_BOUND('',#4251,.T.);
#2767=FACE_OUTER_BOUND('',#4252,.T.);
#2768=FACE_OUTER_BOUND('',#4253,.T.);
#2769=FACE_OUTER_BOUND('',#4254,.T.);
#2770=FACE_OUTER_BOUND('',#4255,.T.);
#2771=FACE_OUTER_BOUND('',#4256,.T.);
#2772=FACE_OUTER_BOUND('',#4257,.T.);
#2773=FACE_OUTER_BOUND('',#4258,.T.);
#2774=FACE_OUTER_BOUND('',#4259,.T.);
#2775=FACE_OUTER_BOUND('',#4260,.T.);
#2776=FACE_OUTER_BOUND('',#4261,.T.);
#2777=FACE_OUTER_BOUND('',#4262,.T.);
#2778=FACE_OUTER_BOUND('',#4263,.T.);
#2779=FACE_OUTER_BOUND('',#4264,.T.);
#2780=FACE_OUTER_BOUND('',#4265,.T.);
#2781=FACE_OUTER_BOUND('',#4266,.T.);
#2782=FACE_OUTER_BOUND('',#4267,.T.);
#2783=FACE_OUTER_BOUND('',#4268,.T.);
#2784=FACE_OUTER_BOUND('',#4269,.T.);
#2785=FACE_OUTER_BOUND('',#4270,.T.);
#2786=FACE_OUTER_BOUND('',#4271,.T.);
#2787=FACE_OUTER_BOUND('',#4272,.T.);
#2788=FACE_OUTER_BOUND('',#4273,.T.);
#2789=FACE_OUTER_BOUND('',#4274,.T.);
#2790=FACE_OUTER_BOUND('',#4275,.T.);
#2791=FACE_OUTER_BOUND('',#4276,.T.);
#2792=FACE_OUTER_BOUND('',#4277,.T.);
#2793=FACE_OUTER_BOUND('',#4278,.T.);
#2794=FACE_OUTER_BOUND('',#4279,.T.);
#2795=FACE_OUTER_BOUND('',#4280,.T.);
#2796=FACE_OUTER_BOUND('',#4281,.T.);
#2797=FACE_OUTER_BOUND('',#4282,.T.);
#2798=FACE_OUTER_BOUND('',#4283,.T.);
#2799=FACE_OUTER_BOUND('',#4284,.T.);
#2800=FACE_OUTER_BOUND('',#4285,.T.);
#2801=FACE_OUTER_BOUND('',#4286,.T.);
#2802=FACE_OUTER_BOUND('',#4287,.T.);
#2803=FACE_OUTER_BOUND('',#4288,.T.);
#2804=FACE_OUTER_BOUND('',#4289,.T.);
#2805=FACE_OUTER_BOUND('',#4290,.T.);
#2806=FACE_OUTER_BOUND('',#4291,.T.);
#2807=FACE_OUTER_BOUND('',#4292,.T.);
#2808=FACE_OUTER_BOUND('',#4293,.T.);
#2809=FACE_OUTER_BOUND('',#4294,.T.);
#2810=FACE_OUTER_BOUND('',#4295,.T.);
#2811=FACE_OUTER_BOUND('',#4296,.T.);
#2812=FACE_OUTER_BOUND('',#4297,.T.);
#2813=FACE_OUTER_BOUND('',#4298,.T.);
#2814=FACE_OUTER_BOUND('',#4299,.T.);
#2815=FACE_OUTER_BOUND('',#4300,.T.);
#2816=FACE_OUTER_BOUND('',#4301,.T.);
#2817=FACE_OUTER_BOUND('',#4302,.T.);
#2818=FACE_OUTER_BOUND('',#4303,.T.);
#2819=FACE_OUTER_BOUND('',#4304,.T.);
#2820=FACE_OUTER_BOUND('',#4305,.T.);
#2821=FACE_OUTER_BOUND('',#4306,.T.);
#2822=FACE_OUTER_BOUND('',#4307,.T.);
#2823=FACE_OUTER_BOUND('',#4308,.T.);
#2824=FACE_OUTER_BOUND('',#4309,.T.);
#2825=FACE_OUTER_BOUND('',#4310,.T.);
#2826=FACE_OUTER_BOUND('',#4311,.T.);
#2827=FACE_OUTER_BOUND('',#4312,.T.);
#2828=FACE_OUTER_BOUND('',#4313,.T.);
#2829=FACE_OUTER_BOUND('',#4315,.T.);
#2830=FACE_OUTER_BOUND('',#4316,.T.);
#2831=FACE_OUTER_BOUND('',#4317,.T.);
#2832=FACE_OUTER_BOUND('',#4318,.T.);
#2833=FACE_OUTER_BOUND('',#4319,.T.);
#2834=FACE_OUTER_BOUND('',#4321,.T.);
#2835=FACE_OUTER_BOUND('',#4322,.T.);
#2836=FACE_OUTER_BOUND('',#4324,.T.);
#2837=FACE_OUTER_BOUND('',#4325,.T.);
#2838=FACE_OUTER_BOUND('',#4326,.T.);
#2839=FACE_OUTER_BOUND('',#4328,.T.);
#2840=FACE_OUTER_BOUND('',#4329,.T.);
#2841=FACE_OUTER_BOUND('',#4330,.T.);
#2842=FACE_OUTER_BOUND('',#4331,.T.);
#2843=FACE_OUTER_BOUND('',#4332,.T.);
#2844=FACE_OUTER_BOUND('',#4333,.T.);
#2845=FACE_OUTER_BOUND('',#4335,.T.);
#2846=FACE_OUTER_BOUND('',#4336,.T.);
#2847=FACE_OUTER_BOUND('',#4337,.T.);
#2848=FACE_OUTER_BOUND('',#4338,.T.);
#2849=FACE_OUTER_BOUND('',#4339,.T.);
#2850=FACE_OUTER_BOUND('',#4340,.T.);
#2851=FACE_OUTER_BOUND('',#4341,.T.);
#2852=FACE_OUTER_BOUND('',#4342,.T.);
#2853=FACE_OUTER_BOUND('',#4343,.T.);
#2854=FACE_OUTER_BOUND('',#4347,.T.);
#2855=FACE_OUTER_BOUND('',#4348,.T.);
#2856=FACE_OUTER_BOUND('',#4349,.T.);
#2857=FACE_OUTER_BOUND('',#4350,.T.);
#2858=FACE_OUTER_BOUND('',#4351,.T.);
#2859=FACE_OUTER_BOUND('',#4352,.T.);
#2860=FACE_OUTER_BOUND('',#4353,.T.);
#2861=FACE_OUTER_BOUND('',#4354,.T.);
#2862=FACE_OUTER_BOUND('',#4355,.T.);
#2863=FACE_OUTER_BOUND('',#4356,.T.);
#2864=FACE_OUTER_BOUND('',#4358,.T.);
#2865=FACE_OUTER_BOUND('',#4359,.T.);
#2866=FACE_OUTER_BOUND('',#4360,.T.);
#2867=FACE_OUTER_BOUND('',#4361,.T.);
#2868=FACE_OUTER_BOUND('',#4362,.T.);
#2869=FACE_OUTER_BOUND('',#4363,.T.);
#2870=FACE_OUTER_BOUND('',#4364,.T.);
#2871=FACE_OUTER_BOUND('',#4365,.T.);
#2872=FACE_OUTER_BOUND('',#4366,.T.);
#2873=FACE_OUTER_BOUND('',#4368,.T.);
#2874=FACE_OUTER_BOUND('',#4369,.T.);
#2875=FACE_OUTER_BOUND('',#4370,.T.);
#2876=FACE_OUTER_BOUND('',#4371,.T.);
#2877=FACE_OUTER_BOUND('',#4373,.T.);
#2878=FACE_OUTER_BOUND('',#4374,.T.);
#2879=FACE_OUTER_BOUND('',#4376,.T.);
#2880=FACE_OUTER_BOUND('',#4377,.T.);
#2881=FACE_OUTER_BOUND('',#4378,.T.);
#2882=FACE_OUTER_BOUND('',#4379,.T.);
#2883=FACE_OUTER_BOUND('',#4380,.T.);
#2884=FACE_OUTER_BOUND('',#4381,.T.);
#2885=FACE_OUTER_BOUND('',#4382,.T.);
#2886=FACE_OUTER_BOUND('',#4383,.T.);
#2887=FACE_OUTER_BOUND('',#4384,.T.);
#2888=FACE_OUTER_BOUND('',#4385,.T.);
#2889=FACE_OUTER_BOUND('',#4386,.T.);
#2890=FACE_OUTER_BOUND('',#4387,.T.);
#2891=FACE_OUTER_BOUND('',#4388,.T.);
#2892=FACE_OUTER_BOUND('',#4399,.T.);
#2893=FACE_OUTER_BOUND('',#4400,.T.);
#2894=FACE_OUTER_BOUND('',#4411,.T.);
#2895=FACE_OUTER_BOUND('',#4412,.T.);
#2896=FACE_OUTER_BOUND('',#4413,.T.);
#2897=FACE_OUTER_BOUND('',#4414,.T.);
#2898=FACE_OUTER_BOUND('',#4415,.T.);
#2899=FACE_OUTER_BOUND('',#4416,.T.);
#2900=FACE_OUTER_BOUND('',#4417,.T.);
#2901=FACE_OUTER_BOUND('',#4418,.T.);
#2902=FACE_OUTER_BOUND('',#4419,.T.);
#2903=FACE_OUTER_BOUND('',#4420,.T.);
#2904=FACE_OUTER_BOUND('',#4422,.T.);
#2905=FACE_OUTER_BOUND('',#4423,.T.);
#2906=FACE_OUTER_BOUND('',#4424,.T.);
#2907=FACE_OUTER_BOUND('',#4425,.T.);
#2908=FACE_OUTER_BOUND('',#4427,.T.);
#2909=FACE_OUTER_BOUND('',#4429,.T.);
#2910=FACE_OUTER_BOUND('',#4430,.T.);
#2911=FACE_OUTER_BOUND('',#4432,.T.);
#2912=FACE_OUTER_BOUND('',#4433,.T.);
#2913=FACE_OUTER_BOUND('',#4434,.T.);
#2914=FACE_OUTER_BOUND('',#4435,.T.);
#2915=FACE_OUTER_BOUND('',#4439,.T.);
#2916=FACE_OUTER_BOUND('',#4440,.T.);
#2917=FACE_OUTER_BOUND('',#4442,.T.);
#2918=FACE_OUTER_BOUND('',#4443,.T.);
#2919=FACE_OUTER_BOUND('',#4444,.T.);
#2920=FACE_OUTER_BOUND('',#4445,.T.);
#2921=FACE_OUTER_BOUND('',#4446,.T.);
#2922=FACE_OUTER_BOUND('',#4448,.T.);
#2923=FACE_OUTER_BOUND('',#4449,.T.);
#2924=FACE_OUTER_BOUND('',#4450,.T.);
#2925=FACE_OUTER_BOUND('',#4451,.T.);
#2926=FACE_OUTER_BOUND('',#4452,.T.);
#2927=FACE_OUTER_BOUND('',#4453,.T.);
#2928=FACE_OUTER_BOUND('',#4455,.T.);
#2929=FACE_OUTER_BOUND('',#4456,.T.);
#2930=FACE_OUTER_BOUND('',#4457,.T.);
#2931=FACE_OUTER_BOUND('',#4458,.T.);
#2932=FACE_OUTER_BOUND('',#4459,.T.);
#2933=FACE_OUTER_BOUND('',#4460,.T.);
#2934=FACE_OUTER_BOUND('',#4461,.T.);
#2935=FACE_OUTER_BOUND('',#4462,.T.);
#2936=FACE_OUTER_BOUND('',#4467,.T.);
#2937=FACE_OUTER_BOUND('',#4468,.T.);
#2938=FACE_OUTER_BOUND('',#4473,.T.);
#2939=FACE_OUTER_BOUND('',#4474,.T.);
#2940=FACE_OUTER_BOUND('',#4475,.T.);
#2941=FACE_OUTER_BOUND('',#4476,.T.);
#2942=FACE_OUTER_BOUND('',#4477,.T.);
#2943=FACE_OUTER_BOUND('',#4478,.T.);
#2944=FACE_OUTER_BOUND('',#4479,.T.);
#2945=FACE_OUTER_BOUND('',#4480,.T.);
#2946=FACE_OUTER_BOUND('',#4481,.T.);
#2947=FACE_OUTER_BOUND('',#4482,.T.);
#2948=FACE_OUTER_BOUND('',#4483,.T.);
#2949=FACE_OUTER_BOUND('',#4484,.T.);
#2950=FACE_OUTER_BOUND('',#4485,.T.);
#2951=FACE_OUTER_BOUND('',#4486,.T.);
#2952=FACE_OUTER_BOUND('',#4488,.T.);
#2953=FACE_OUTER_BOUND('',#4489,.T.);
#2954=FACE_OUTER_BOUND('',#4494,.T.);
#2955=FACE_OUTER_BOUND('',#4495,.T.);
#2956=FACE_OUTER_BOUND('',#4496,.T.);
#2957=FACE_OUTER_BOUND('',#4497,.T.);
#2958=FACE_OUTER_BOUND('',#4498,.T.);
#2959=FACE_OUTER_BOUND('',#4499,.T.);
#2960=FACE_OUTER_BOUND('',#4500,.T.);
#2961=FACE_OUTER_BOUND('',#4501,.T.);
#2962=FACE_OUTER_BOUND('',#4502,.T.);
#2963=FACE_OUTER_BOUND('',#4503,.T.);
#2964=FACE_OUTER_BOUND('',#4504,.T.);
#2965=FACE_OUTER_BOUND('',#4505,.T.);
#2966=FACE_OUTER_BOUND('',#4506,.T.);
#2967=FACE_OUTER_BOUND('',#4507,.T.);
#2968=FACE_OUTER_BOUND('',#4508,.T.);
#2969=FACE_OUTER_BOUND('',#4509,.T.);
#2970=FACE_OUTER_BOUND('',#4520,.T.);
#2971=FACE_OUTER_BOUND('',#4521,.T.);
#2972=FACE_OUTER_BOUND('',#4522,.T.);
#2973=FACE_OUTER_BOUND('',#4523,.T.);
#2974=FACE_OUTER_BOUND('',#4524,.T.);
#2975=FACE_OUTER_BOUND('',#4525,.T.);
#2976=FACE_OUTER_BOUND('',#4526,.T.);
#2977=FACE_OUTER_BOUND('',#4527,.T.);
#2978=FACE_OUTER_BOUND('',#4528,.T.);
#2979=FACE_OUTER_BOUND('',#4529,.T.);
#2980=FACE_OUTER_BOUND('',#4530,.T.);
#2981=FACE_OUTER_BOUND('',#4531,.T.);
#2982=FACE_OUTER_BOUND('',#4532,.T.);
#2983=FACE_OUTER_BOUND('',#4533,.T.);
#2984=FACE_OUTER_BOUND('',#4534,.T.);
#2985=FACE_OUTER_BOUND('',#4535,.T.);
#2986=FACE_OUTER_BOUND('',#4536,.T.);
#2987=FACE_OUTER_BOUND('',#4537,.T.);
#2988=FACE_OUTER_BOUND('',#4538,.T.);
#2989=FACE_OUTER_BOUND('',#4539,.T.);
#2990=FACE_OUTER_BOUND('',#4540,.T.);
#2991=FACE_OUTER_BOUND('',#4541,.T.);
#2992=FACE_OUTER_BOUND('',#4542,.T.);
#2993=FACE_OUTER_BOUND('',#4543,.T.);
#2994=FACE_OUTER_BOUND('',#4544,.T.);
#2995=FACE_OUTER_BOUND('',#4545,.T.);
#2996=FACE_OUTER_BOUND('',#4546,.T.);
#2997=FACE_OUTER_BOUND('',#4547,.T.);
#2998=FACE_OUTER_BOUND('',#4548,.T.);
#2999=FACE_OUTER_BOUND('',#4549,.T.);
#3000=FACE_OUTER_BOUND('',#4560,.T.);
#3001=FACE_OUTER_BOUND('',#4561,.T.);
#3002=FACE_OUTER_BOUND('',#4562,.T.);
#3003=FACE_OUTER_BOUND('',#4563,.T.);
#3004=FACE_OUTER_BOUND('',#4564,.T.);
#3005=FACE_OUTER_BOUND('',#4565,.T.);
#3006=FACE_OUTER_BOUND('',#4566,.T.);
#3007=FACE_OUTER_BOUND('',#4567,.T.);
#3008=FACE_OUTER_BOUND('',#4569,.T.);
#3009=FACE_OUTER_BOUND('',#4570,.T.);
#3010=FACE_OUTER_BOUND('',#4571,.T.);
#3011=FACE_OUTER_BOUND('',#4572,.T.);
#3012=FACE_OUTER_BOUND('',#4574,.T.);
#3013=FACE_OUTER_BOUND('',#4575,.T.);
#3014=FACE_OUTER_BOUND('',#4576,.T.);
#3015=FACE_OUTER_BOUND('',#4580,.T.);
#3016=FACE_OUTER_BOUND('',#4581,.T.);
#3017=FACE_OUTER_BOUND('',#4582,.T.);
#3018=FACE_OUTER_BOUND('',#4583,.T.);
#3019=FACE_OUTER_BOUND('',#4584,.T.);
#3020=FACE_OUTER_BOUND('',#4585,.T.);
#3021=FACE_OUTER_BOUND('',#4588,.T.);
#3022=FACE_OUTER_BOUND('',#4589,.T.);
#3023=FACE_OUTER_BOUND('',#4590,.T.);
#3024=FACE_OUTER_BOUND('',#4591,.T.);
#3025=FACE_OUTER_BOUND('',#4592,.T.);
#3026=FACE_OUTER_BOUND('',#4593,.T.);
#3027=FACE_OUTER_BOUND('',#4594,.T.);
#3028=FACE_OUTER_BOUND('',#4595,.T.);
#3029=FACE_OUTER_BOUND('',#4596,.T.);
#3030=FACE_OUTER_BOUND('',#4597,.T.);
#3031=FACE_OUTER_BOUND('',#4598,.T.);
#3032=FACE_OUTER_BOUND('',#4599,.T.);
#3033=FACE_OUTER_BOUND('',#4600,.T.);
#3034=FACE_OUTER_BOUND('',#4601,.T.);
#3035=FACE_OUTER_BOUND('',#4602,.T.);
#3036=FACE_OUTER_BOUND('',#4603,.T.);
#3037=FACE_OUTER_BOUND('',#4604,.T.);
#3038=FACE_OUTER_BOUND('',#4605,.T.);
#3039=FACE_OUTER_BOUND('',#4606,.T.);
#3040=FACE_OUTER_BOUND('',#4607,.T.);
#3041=FACE_OUTER_BOUND('',#4608,.T.);
#3042=FACE_OUTER_BOUND('',#4609,.T.);
#3043=FACE_OUTER_BOUND('',#4610,.T.);
#3044=FACE_OUTER_BOUND('',#4611,.T.);
#3045=FACE_OUTER_BOUND('',#4612,.T.);
#3046=FACE_OUTER_BOUND('',#4613,.T.);
#3047=FACE_OUTER_BOUND('',#4614,.T.);
#3048=FACE_OUTER_BOUND('',#4615,.T.);
#3049=FACE_OUTER_BOUND('',#4616,.T.);
#3050=FACE_OUTER_BOUND('',#4617,.T.);
#3051=FACE_OUTER_BOUND('',#4620,.T.);
#3052=FACE_OUTER_BOUND('',#4621,.T.);
#3053=FACE_OUTER_BOUND('',#4624,.T.);
#3054=FACE_OUTER_BOUND('',#4625,.T.);
#3055=FACE_OUTER_BOUND('',#4627,.T.);
#3056=FACE_OUTER_BOUND('',#4628,.T.);
#3057=FACE_OUTER_BOUND('',#4629,.T.);
#3058=FACE_OUTER_BOUND('',#4630,.T.);
#3059=FACE_OUTER_BOUND('',#4631,.T.);
#3060=FACE_OUTER_BOUND('',#4632,.T.);
#3061=FACE_OUTER_BOUND('',#4633,.T.);
#3062=FACE_OUTER_BOUND('',#4634,.T.);
#3063=FACE_OUTER_BOUND('',#4635,.T.);
#3064=FACE_OUTER_BOUND('',#4636,.T.);
#3065=FACE_OUTER_BOUND('',#4637,.T.);
#3066=FACE_OUTER_BOUND('',#4638,.T.);
#3067=FACE_OUTER_BOUND('',#4639,.T.);
#3068=FACE_OUTER_BOUND('',#4640,.T.);
#3069=FACE_OUTER_BOUND('',#4641,.T.);
#3070=FACE_OUTER_BOUND('',#4642,.T.);
#3071=FACE_OUTER_BOUND('',#4643,.T.);
#3072=FACE_OUTER_BOUND('',#4644,.T.);
#3073=FACE_OUTER_BOUND('',#4645,.T.);
#3074=FACE_OUTER_BOUND('',#4646,.T.);
#3075=FACE_OUTER_BOUND('',#4647,.T.);
#3076=FACE_OUTER_BOUND('',#4648,.T.);
#3077=FACE_OUTER_BOUND('',#4649,.T.);
#3078=FACE_OUTER_BOUND('',#4650,.T.);
#3079=FACE_OUTER_BOUND('',#4651,.T.);
#3080=FACE_OUTER_BOUND('',#4652,.T.);
#3081=FACE_OUTER_BOUND('',#4653,.T.);
#3082=FACE_OUTER_BOUND('',#4654,.T.);
#3083=FACE_OUTER_BOUND('',#4655,.T.);
#3084=FACE_OUTER_BOUND('',#4656,.T.);
#3085=FACE_OUTER_BOUND('',#4657,.T.);
#3086=FACE_OUTER_BOUND('',#4658,.T.);
#3087=FACE_OUTER_BOUND('',#4659,.T.);
#3088=FACE_OUTER_BOUND('',#4660,.T.);
#3089=FACE_OUTER_BOUND('',#4661,.T.);
#3090=FACE_OUTER_BOUND('',#4662,.T.);
#3091=FACE_OUTER_BOUND('',#4663,.T.);
#3092=FACE_OUTER_BOUND('',#4668,.T.);
#3093=FACE_OUTER_BOUND('',#4669,.T.);
#3094=FACE_OUTER_BOUND('',#4681,.T.);
#3095=FACE_OUTER_BOUND('',#4682,.T.);
#3096=FACE_OUTER_BOUND('',#4683,.T.);
#3097=FACE_OUTER_BOUND('',#4684,.T.);
#3098=FACE_OUTER_BOUND('',#4685,.T.);
#3099=FACE_OUTER_BOUND('',#4686,.T.);
#3100=FACE_OUTER_BOUND('',#4687,.T.);
#3101=FACE_OUTER_BOUND('',#4688,.T.);
#3102=FACE_OUTER_BOUND('',#4689,.T.);
#3103=FACE_OUTER_BOUND('',#4690,.T.);
#3104=FACE_OUTER_BOUND('',#4691,.T.);
#3105=FACE_OUTER_BOUND('',#4692,.T.);
#3106=FACE_OUTER_BOUND('',#4693,.T.);
#3107=FACE_OUTER_BOUND('',#4694,.T.);
#3108=FACE_OUTER_BOUND('',#4695,.T.);
#3109=FACE_OUTER_BOUND('',#4696,.T.);
#3110=FACE_OUTER_BOUND('',#4697,.T.);
#3111=FACE_OUTER_BOUND('',#4698,.T.);
#3112=FACE_OUTER_BOUND('',#4699,.T.);
#3113=FACE_OUTER_BOUND('',#4700,.T.);
#3114=FACE_OUTER_BOUND('',#4701,.T.);
#3115=FACE_OUTER_BOUND('',#4703,.T.);
#3116=FACE_OUTER_BOUND('',#4704,.T.);
#3117=FACE_OUTER_BOUND('',#4705,.T.);
#3118=FACE_OUTER_BOUND('',#4706,.T.);
#3119=FACE_OUTER_BOUND('',#4708,.T.);
#3120=FACE_OUTER_BOUND('',#4709,.T.);
#3121=FACE_OUTER_BOUND('',#4710,.T.);
#3122=FACE_OUTER_BOUND('',#4711,.T.);
#3123=FACE_OUTER_BOUND('',#4712,.T.);
#3124=FACE_OUTER_BOUND('',#4713,.T.);
#3125=FACE_OUTER_BOUND('',#4714,.T.);
#3126=FACE_OUTER_BOUND('',#4715,.T.);
#3127=FACE_OUTER_BOUND('',#4716,.T.);
#3128=FACE_OUTER_BOUND('',#4717,.T.);
#3129=FACE_OUTER_BOUND('',#4718,.T.);
#3130=FACE_OUTER_BOUND('',#4719,.T.);
#3131=FACE_OUTER_BOUND('',#4720,.T.);
#3132=FACE_OUTER_BOUND('',#4721,.T.);
#3133=FACE_OUTER_BOUND('',#4722,.T.);
#3134=FACE_OUTER_BOUND('',#4723,.T.);
#3135=FACE_OUTER_BOUND('',#4724,.T.);
#3136=FACE_OUTER_BOUND('',#4725,.T.);
#3137=FACE_OUTER_BOUND('',#4726,.T.);
#3138=FACE_OUTER_BOUND('',#4727,.T.);
#3139=FACE_OUTER_BOUND('',#4728,.T.);
#3140=FACE_OUTER_BOUND('',#4729,.T.);
#3141=FACE_OUTER_BOUND('',#4730,.T.);
#3142=FACE_OUTER_BOUND('',#4731,.T.);
#3143=FACE_OUTER_BOUND('',#4732,.T.);
#3144=FACE_OUTER_BOUND('',#4733,.T.);
#3145=FACE_OUTER_BOUND('',#4734,.T.);
#3146=FACE_OUTER_BOUND('',#4735,.T.);
#3147=FACE_OUTER_BOUND('',#4736,.T.);
#3148=FACE_OUTER_BOUND('',#4737,.T.);
#3149=FACE_OUTER_BOUND('',#4738,.T.);
#3150=FACE_OUTER_BOUND('',#4739,.T.);
#3151=FACE_OUTER_BOUND('',#4740,.T.);
#3152=FACE_OUTER_BOUND('',#4741,.T.);
#3153=FACE_OUTER_BOUND('',#4743,.T.);
#3154=FACE_OUTER_BOUND('',#4744,.T.);
#3155=FACE_OUTER_BOUND('',#4745,.T.);
#3156=FACE_OUTER_BOUND('',#4746,.T.);
#3157=FACE_OUTER_BOUND('',#4747,.T.);
#3158=FACE_OUTER_BOUND('',#4748,.T.);
#3159=FACE_OUTER_BOUND('',#4749,.T.);
#3160=FACE_OUTER_BOUND('',#4750,.T.);
#3161=FACE_OUTER_BOUND('',#4751,.T.);
#3162=FACE_OUTER_BOUND('',#4752,.T.);
#3163=FACE_OUTER_BOUND('',#4753,.T.);
#3164=FACE_OUTER_BOUND('',#4754,.T.);
#3165=FACE_OUTER_BOUND('',#4756,.T.);
#3166=FACE_OUTER_BOUND('',#4757,.T.);
#3167=FACE_OUTER_BOUND('',#4758,.T.);
#3168=FACE_OUTER_BOUND('',#4759,.T.);
#3169=FACE_OUTER_BOUND('',#4760,.T.);
#3170=FACE_OUTER_BOUND('',#4761,.T.);
#3171=FACE_OUTER_BOUND('',#4762,.T.);
#3172=FACE_OUTER_BOUND('',#4763,.T.);
#3173=FACE_OUTER_BOUND('',#4764,.T.);
#3174=FACE_OUTER_BOUND('',#4765,.T.);
#3175=FACE_OUTER_BOUND('',#4766,.T.);
#3176=FACE_OUTER_BOUND('',#4767,.T.);
#3177=FACE_OUTER_BOUND('',#4768,.T.);
#3178=FACE_OUTER_BOUND('',#4769,.T.);
#3179=FACE_OUTER_BOUND('',#4770,.T.);
#3180=FACE_OUTER_BOUND('',#4771,.T.);
#3181=FACE_OUTER_BOUND('',#4772,.T.);
#3182=FACE_OUTER_BOUND('',#4773,.T.);
#3183=FACE_OUTER_BOUND('',#4774,.T.);
#3184=FACE_OUTER_BOUND('',#4775,.T.);
#3185=FACE_OUTER_BOUND('',#4776,.T.);
#3186=FACE_OUTER_BOUND('',#4777,.T.);
#3187=FACE_OUTER_BOUND('',#4778,.T.);
#3188=FACE_OUTER_BOUND('',#4779,.T.);
#3189=FACE_OUTER_BOUND('',#4780,.T.);
#3190=FACE_OUTER_BOUND('',#4781,.T.);
#3191=FACE_OUTER_BOUND('',#4782,.T.);
#3192=FACE_OUTER_BOUND('',#4783,.T.);
#3193=FACE_OUTER_BOUND('',#4784,.T.);
#3194=FACE_OUTER_BOUND('',#4785,.T.);
#3195=FACE_OUTER_BOUND('',#4786,.T.);
#3196=FACE_OUTER_BOUND('',#4787,.T.);
#3197=FACE_OUTER_BOUND('',#4788,.T.);
#3198=FACE_OUTER_BOUND('',#4789,.T.);
#3199=FACE_OUTER_BOUND('',#4790,.T.);
#3200=FACE_OUTER_BOUND('',#4791,.T.);
#3201=FACE_OUTER_BOUND('',#4792,.T.);
#3202=FACE_OUTER_BOUND('',#4793,.T.);
#3203=FACE_OUTER_BOUND('',#4794,.T.);
#3204=FACE_OUTER_BOUND('',#4795,.T.);
#3205=FACE_OUTER_BOUND('',#4796,.T.);
#3206=FACE_OUTER_BOUND('',#4797,.T.);
#3207=FACE_OUTER_BOUND('',#4798,.T.);
#3208=FACE_OUTER_BOUND('',#4799,.T.);
#3209=FACE_OUTER_BOUND('',#4800,.T.);
#3210=FACE_OUTER_BOUND('',#4801,.T.);
#3211=FACE_OUTER_BOUND('',#4802,.T.);
#3212=FACE_OUTER_BOUND('',#4803,.T.);
#3213=FACE_OUTER_BOUND('',#4804,.T.);
#3214=FACE_OUTER_BOUND('',#4805,.T.);
#3215=FACE_OUTER_BOUND('',#4806,.T.);
#3216=FACE_OUTER_BOUND('',#4807,.T.);
#3217=FACE_OUTER_BOUND('',#4808,.T.);
#3218=FACE_OUTER_BOUND('',#4809,.T.);
#3219=FACE_OUTER_BOUND('',#4810,.T.);
#3220=FACE_OUTER_BOUND('',#4811,.T.);
#3221=FACE_OUTER_BOUND('',#4812,.T.);
#3222=FACE_OUTER_BOUND('',#4813,.T.);
#3223=FACE_OUTER_BOUND('',#4814,.T.);
#3224=FACE_OUTER_BOUND('',#4815,.T.);
#3225=FACE_OUTER_BOUND('',#4816,.T.);
#3226=FACE_OUTER_BOUND('',#4817,.T.);
#3227=FACE_OUTER_BOUND('',#4818,.T.);
#3228=FACE_OUTER_BOUND('',#4819,.T.);
#3229=FACE_OUTER_BOUND('',#4820,.T.);
#3230=FACE_OUTER_BOUND('',#4821,.T.);
#3231=FACE_OUTER_BOUND('',#4822,.T.);
#3232=FACE_OUTER_BOUND('',#4823,.T.);
#3233=FACE_OUTER_BOUND('',#4824,.T.);
#3234=FACE_OUTER_BOUND('',#4825,.T.);
#3235=FACE_OUTER_BOUND('',#4826,.T.);
#3236=FACE_OUTER_BOUND('',#4827,.T.);
#3237=FACE_OUTER_BOUND('',#4828,.T.);
#3238=FACE_OUTER_BOUND('',#4829,.T.);
#3239=FACE_OUTER_BOUND('',#4830,.T.);
#3240=FACE_OUTER_BOUND('',#4831,.T.);
#3241=FACE_OUTER_BOUND('',#4832,.T.);
#3242=FACE_OUTER_BOUND('',#4833,.T.);
#3243=FACE_OUTER_BOUND('',#4834,.T.);
#3244=FACE_OUTER_BOUND('',#4835,.T.);
#3245=FACE_OUTER_BOUND('',#4836,.T.);
#3246=FACE_OUTER_BOUND('',#4837,.T.);
#3247=FACE_OUTER_BOUND('',#4838,.T.);
#3248=FACE_OUTER_BOUND('',#4839,.T.);
#3249=FACE_OUTER_BOUND('',#4840,.T.);
#3250=FACE_OUTER_BOUND('',#4841,.T.);
#3251=FACE_OUTER_BOUND('',#4842,.T.);
#3252=FACE_OUTER_BOUND('',#4843,.T.);
#3253=FACE_OUTER_BOUND('',#4844,.T.);
#3254=FACE_OUTER_BOUND('',#4845,.T.);
#3255=FACE_OUTER_BOUND('',#4846,.T.);
#3256=FACE_OUTER_BOUND('',#4847,.T.);
#3257=FACE_OUTER_BOUND('',#4848,.T.);
#3258=FACE_OUTER_BOUND('',#4849,.T.);
#3259=FACE_OUTER_BOUND('',#4850,.T.);
#3260=FACE_OUTER_BOUND('',#4851,.T.);
#3261=FACE_OUTER_BOUND('',#4852,.T.);
#3262=FACE_OUTER_BOUND('',#4853,.T.);
#3263=FACE_OUTER_BOUND('',#4854,.T.);
#3264=FACE_OUTER_BOUND('',#4855,.T.);
#3265=FACE_OUTER_BOUND('',#4856,.T.);
#3266=FACE_OUTER_BOUND('',#4857,.T.);
#3267=FACE_OUTER_BOUND('',#4858,.T.);
#3268=FACE_OUTER_BOUND('',#4859,.T.);
#3269=FACE_OUTER_BOUND('',#4860,.T.);
#3270=FACE_OUTER_BOUND('',#4861,.T.);
#3271=FACE_OUTER_BOUND('',#4862,.T.);
#3272=FACE_OUTER_BOUND('',#4863,.T.);
#3273=FACE_OUTER_BOUND('',#4864,.T.);
#3274=FACE_OUTER_BOUND('',#4865,.T.);
#3275=FACE_OUTER_BOUND('',#4866,.T.);
#3276=FACE_OUTER_BOUND('',#4867,.T.);
#3277=FACE_OUTER_BOUND('',#4868,.T.);
#3278=FACE_OUTER_BOUND('',#4869,.T.);
#3279=FACE_OUTER_BOUND('',#4870,.T.);
#3280=FACE_OUTER_BOUND('',#4871,.T.);
#3281=FACE_OUTER_BOUND('',#4872,.T.);
#3282=FACE_OUTER_BOUND('',#4873,.T.);
#3283=FACE_OUTER_BOUND('',#4874,.T.);
#3284=FACE_OUTER_BOUND('',#4875,.T.);
#3285=FACE_OUTER_BOUND('',#4876,.T.);
#3286=FACE_OUTER_BOUND('',#4877,.T.);
#3287=FACE_OUTER_BOUND('',#4878,.T.);
#3288=FACE_OUTER_BOUND('',#4879,.T.);
#3289=FACE_OUTER_BOUND('',#4880,.T.);
#3290=FACE_OUTER_BOUND('',#4881,.T.);
#3291=FACE_OUTER_BOUND('',#4882,.T.);
#3292=FACE_OUTER_BOUND('',#4883,.T.);
#3293=FACE_OUTER_BOUND('',#4884,.T.);
#3294=FACE_OUTER_BOUND('',#4885,.T.);
#3295=FACE_OUTER_BOUND('',#4886,.T.);
#3296=FACE_OUTER_BOUND('',#4887,.T.);
#3297=FACE_OUTER_BOUND('',#4888,.T.);
#3298=FACE_OUTER_BOUND('',#4889,.T.);
#3299=FACE_OUTER_BOUND('',#4890,.T.);
#3300=FACE_OUTER_BOUND('',#4891,.T.);
#3301=FACE_OUTER_BOUND('',#4892,.T.);
#3302=FACE_OUTER_BOUND('',#4893,.T.);
#3303=FACE_OUTER_BOUND('',#4894,.T.);
#3304=FACE_OUTER_BOUND('',#4895,.T.);
#3305=FACE_OUTER_BOUND('',#4896,.T.);
#3306=FACE_OUTER_BOUND('',#4897,.T.);
#3307=FACE_OUTER_BOUND('',#4898,.T.);
#3308=FACE_OUTER_BOUND('',#4899,.T.);
#3309=FACE_OUTER_BOUND('',#4900,.T.);
#3310=FACE_OUTER_BOUND('',#4901,.T.);
#3311=FACE_OUTER_BOUND('',#4902,.T.);
#3312=FACE_OUTER_BOUND('',#4903,.T.);
#3313=FACE_OUTER_BOUND('',#4904,.T.);
#3314=FACE_OUTER_BOUND('',#4905,.T.);
#3315=FACE_OUTER_BOUND('',#4906,.T.);
#3316=FACE_OUTER_BOUND('',#4907,.T.);
#3317=FACE_OUTER_BOUND('',#4908,.T.);
#3318=FACE_OUTER_BOUND('',#4909,.T.);
#3319=FACE_OUTER_BOUND('',#4910,.T.);
#3320=FACE_OUTER_BOUND('',#4911,.T.);
#3321=FACE_OUTER_BOUND('',#4912,.T.);
#3322=FACE_OUTER_BOUND('',#4913,.T.);
#3323=FACE_OUTER_BOUND('',#4914,.T.);
#3324=FACE_OUTER_BOUND('',#4915,.T.);
#3325=FACE_OUTER_BOUND('',#4916,.T.);
#3326=FACE_OUTER_BOUND('',#4917,.T.);
#3327=FACE_OUTER_BOUND('',#4918,.T.);
#3328=FACE_OUTER_BOUND('',#4919,.T.);
#3329=FACE_OUTER_BOUND('',#4920,.T.);
#3330=FACE_OUTER_BOUND('',#4921,.T.);
#3331=FACE_OUTER_BOUND('',#4922,.T.);
#3332=FACE_OUTER_BOUND('',#4923,.T.);
#3333=FACE_OUTER_BOUND('',#4924,.T.);
#3334=FACE_OUTER_BOUND('',#4925,.T.);
#3335=FACE_OUTER_BOUND('',#4926,.T.);
#3336=FACE_OUTER_BOUND('',#4927,.T.);
#3337=FACE_OUTER_BOUND('',#4928,.T.);
#3338=FACE_OUTER_BOUND('',#4929,.T.);
#3339=FACE_OUTER_BOUND('',#4930,.T.);
#3340=FACE_OUTER_BOUND('',#4931,.T.);
#3341=FACE_OUTER_BOUND('',#4932,.T.);
#3342=FACE_OUTER_BOUND('',#4933,.T.);
#3343=FACE_OUTER_BOUND('',#4934,.T.);
#3344=FACE_OUTER_BOUND('',#4935,.T.);
#3345=FACE_OUTER_BOUND('',#4937,.T.);
#3346=FACE_OUTER_BOUND('',#4938,.T.);
#3347=FACE_OUTER_BOUND('',#4939,.T.);
#3348=FACE_OUTER_BOUND('',#4940,.T.);
#3349=FACE_OUTER_BOUND('',#4941,.T.);
#3350=FACE_OUTER_BOUND('',#4943,.T.);
#3351=FACE_OUTER_BOUND('',#4945,.T.);
#3352=FACE_OUTER_BOUND('',#4946,.T.);
#3353=FACE_OUTER_BOUND('',#4947,.T.);
#3354=FACE_OUTER_BOUND('',#4948,.T.);
#3355=FACE_OUTER_BOUND('',#4949,.T.);
#3356=FACE_OUTER_BOUND('',#4950,.T.);
#3357=FACE_OUTER_BOUND('',#4951,.T.);
#3358=FACE_OUTER_BOUND('',#4952,.T.);
#3359=FACE_OUTER_BOUND('',#4953,.T.);
#3360=FACE_OUTER_BOUND('',#4954,.T.);
#3361=FACE_OUTER_BOUND('',#4955,.T.);
#3362=FACE_OUTER_BOUND('',#4956,.T.);
#3363=FACE_OUTER_BOUND('',#4957,.T.);
#3364=FACE_OUTER_BOUND('',#4958,.T.);
#3365=FACE_OUTER_BOUND('',#4959,.T.);
#3366=FACE_OUTER_BOUND('',#4960,.T.);
#3367=FACE_OUTER_BOUND('',#4961,.T.);
#3368=FACE_OUTER_BOUND('',#4962,.T.);
#3369=FACE_OUTER_BOUND('',#4963,.T.);
#3370=FACE_OUTER_BOUND('',#4964,.T.);
#3371=FACE_OUTER_BOUND('',#4965,.T.);
#3372=FACE_OUTER_BOUND('',#4966,.T.);
#3373=FACE_OUTER_BOUND('',#4967,.T.);
#3374=FACE_OUTER_BOUND('',#4968,.T.);
#3375=FACE_OUTER_BOUND('',#4969,.T.);
#3376=FACE_OUTER_BOUND('',#4970,.T.);
#3377=FACE_OUTER_BOUND('',#4971,.T.);
#3378=FACE_OUTER_BOUND('',#4972,.T.);
#3379=FACE_OUTER_BOUND('',#4973,.T.);
#3380=FACE_OUTER_BOUND('',#4974,.T.);
#3381=FACE_OUTER_BOUND('',#4975,.T.);
#3382=FACE_OUTER_BOUND('',#4976,.T.);
#3383=FACE_OUTER_BOUND('',#4977,.T.);
#3384=FACE_OUTER_BOUND('',#4978,.T.);
#3385=FACE_OUTER_BOUND('',#4979,.T.);
#3386=FACE_OUTER_BOUND('',#4980,.T.);
#3387=FACE_OUTER_BOUND('',#4981,.T.);
#3388=FACE_OUTER_BOUND('',#4982,.T.);
#3389=FACE_OUTER_BOUND('',#4983,.T.);
#3390=FACE_OUTER_BOUND('',#4984,.T.);
#3391=FACE_OUTER_BOUND('',#4985,.T.);
#3392=FACE_OUTER_BOUND('',#4986,.T.);
#3393=FACE_OUTER_BOUND('',#4987,.T.);
#3394=FACE_OUTER_BOUND('',#4988,.T.);
#3395=FACE_OUTER_BOUND('',#4989,.T.);
#3396=FACE_OUTER_BOUND('',#4990,.T.);
#3397=FACE_OUTER_BOUND('',#4991,.T.);
#3398=FACE_OUTER_BOUND('',#4992,.T.);
#3399=FACE_OUTER_BOUND('',#4993,.T.);
#3400=FACE_OUTER_BOUND('',#4994,.T.);
#3401=FACE_OUTER_BOUND('',#4995,.T.);
#3402=FACE_OUTER_BOUND('',#4996,.T.);
#3403=FACE_OUTER_BOUND('',#4997,.T.);
#3404=FACE_OUTER_BOUND('',#4998,.T.);
#3405=FACE_OUTER_BOUND('',#4999,.T.);
#3406=FACE_OUTER_BOUND('',#5000,.T.);
#3407=FACE_OUTER_BOUND('',#5001,.T.);
#3408=FACE_OUTER_BOUND('',#5002,.T.);
#3409=FACE_OUTER_BOUND('',#5003,.T.);
#3410=FACE_OUTER_BOUND('',#5004,.T.);
#3411=FACE_OUTER_BOUND('',#5005,.T.);
#3412=FACE_OUTER_BOUND('',#5006,.T.);
#3413=FACE_OUTER_BOUND('',#5007,.T.);
#3414=FACE_OUTER_BOUND('',#5008,.T.);
#3415=FACE_OUTER_BOUND('',#5009,.T.);
#3416=FACE_OUTER_BOUND('',#5010,.T.);
#3417=FACE_OUTER_BOUND('',#5011,.T.);
#3418=FACE_OUTER_BOUND('',#5012,.T.);
#3419=FACE_OUTER_BOUND('',#5013,.T.);
#3420=FACE_OUTER_BOUND('',#5014,.T.);
#3421=FACE_OUTER_BOUND('',#5015,.T.);
#3422=FACE_OUTER_BOUND('',#5016,.T.);
#3423=FACE_OUTER_BOUND('',#5017,.T.);
#3424=FACE_OUTER_BOUND('',#5018,.T.);
#3425=FACE_OUTER_BOUND('',#5019,.T.);
#3426=FACE_OUTER_BOUND('',#5020,.T.);
#3427=FACE_OUTER_BOUND('',#5021,.T.);
#3428=FACE_OUTER_BOUND('',#5022,.T.);
#3429=FACE_OUTER_BOUND('',#5023,.T.);
#3430=FACE_OUTER_BOUND('',#5024,.T.);
#3431=FACE_OUTER_BOUND('',#5025,.T.);
#3432=FACE_OUTER_BOUND('',#5026,.T.);
#3433=FACE_OUTER_BOUND('',#5027,.T.);
#3434=FACE_OUTER_BOUND('',#5028,.T.);
#3435=FACE_OUTER_BOUND('',#5029,.T.);
#3436=FACE_OUTER_BOUND('',#5030,.T.);
#3437=FACE_OUTER_BOUND('',#5031,.T.);
#3438=FACE_OUTER_BOUND('',#5032,.T.);
#3439=FACE_OUTER_BOUND('',#5033,.T.);
#3440=FACE_OUTER_BOUND('',#5034,.T.);
#3441=FACE_OUTER_BOUND('',#5035,.T.);
#3442=FACE_OUTER_BOUND('',#5036,.T.);
#3443=FACE_OUTER_BOUND('',#5037,.T.);
#3444=FACE_OUTER_BOUND('',#5038,.T.);
#3445=FACE_OUTER_BOUND('',#5039,.T.);
#3446=FACE_OUTER_BOUND('',#5040,.T.);
#3447=FACE_OUTER_BOUND('',#5041,.T.);
#3448=FACE_OUTER_BOUND('',#5042,.T.);
#3449=FACE_OUTER_BOUND('',#5043,.T.);
#3450=FACE_OUTER_BOUND('',#5044,.T.);
#3451=FACE_OUTER_BOUND('',#5045,.T.);
#3452=FACE_OUTER_BOUND('',#5046,.T.);
#3453=FACE_OUTER_BOUND('',#5047,.T.);
#3454=FACE_OUTER_BOUND('',#5048,.T.);
#3455=FACE_OUTER_BOUND('',#5049,.T.);
#3456=FACE_OUTER_BOUND('',#5050,.T.);
#3457=FACE_OUTER_BOUND('',#5051,.T.);
#3458=FACE_OUTER_BOUND('',#5052,.T.);
#3459=FACE_OUTER_BOUND('',#5053,.T.);
#3460=FACE_OUTER_BOUND('',#5054,.T.);
#3461=FACE_OUTER_BOUND('',#5055,.T.);
#3462=FACE_OUTER_BOUND('',#5056,.T.);
#3463=FACE_OUTER_BOUND('',#5057,.T.);
#3464=FACE_OUTER_BOUND('',#5058,.T.);
#3465=FACE_OUTER_BOUND('',#5059,.T.);
#3466=FACE_OUTER_BOUND('',#5060,.T.);
#3467=FACE_OUTER_BOUND('',#5061,.T.);
#3468=FACE_OUTER_BOUND('',#5062,.T.);
#3469=FACE_OUTER_BOUND('',#5063,.T.);
#3470=FACE_OUTER_BOUND('',#5064,.T.);
#3471=FACE_OUTER_BOUND('',#5065,.T.);
#3472=FACE_OUTER_BOUND('',#5066,.T.);
#3473=FACE_OUTER_BOUND('',#5067,.T.);
#3474=FACE_OUTER_BOUND('',#5068,.T.);
#3475=FACE_OUTER_BOUND('',#5069,.T.);
#3476=FACE_OUTER_BOUND('',#5070,.T.);
#3477=FACE_OUTER_BOUND('',#5071,.T.);
#3478=FACE_OUTER_BOUND('',#5072,.T.);
#3479=FACE_OUTER_BOUND('',#5073,.T.);
#3480=FACE_OUTER_BOUND('',#5074,.T.);
#3481=FACE_OUTER_BOUND('',#5075,.T.);
#3482=FACE_OUTER_BOUND('',#5076,.T.);
#3483=FACE_OUTER_BOUND('',#5077,.T.);
#3484=FACE_OUTER_BOUND('',#5078,.T.);
#3485=FACE_OUTER_BOUND('',#5079,.T.);
#3486=FACE_OUTER_BOUND('',#5080,.T.);
#3487=FACE_OUTER_BOUND('',#5081,.T.);
#3488=FACE_OUTER_BOUND('',#5082,.T.);
#3489=FACE_OUTER_BOUND('',#5083,.T.);
#3490=FACE_OUTER_BOUND('',#5084,.T.);
#3491=FACE_OUTER_BOUND('',#5085,.T.);
#3492=FACE_OUTER_BOUND('',#5086,.T.);
#3493=FACE_OUTER_BOUND('',#5087,.T.);
#3494=FACE_OUTER_BOUND('',#5088,.T.);
#3495=FACE_OUTER_BOUND('',#5089,.T.);
#3496=FACE_OUTER_BOUND('',#5090,.T.);
#3497=FACE_OUTER_BOUND('',#5091,.T.);
#3498=FACE_OUTER_BOUND('',#5092,.T.);
#3499=FACE_OUTER_BOUND('',#5093,.T.);
#3500=FACE_OUTER_BOUND('',#5094,.T.);
#3501=FACE_OUTER_BOUND('',#5095,.T.);
#3502=FACE_OUTER_BOUND('',#5096,.T.);
#3503=FACE_OUTER_BOUND('',#5097,.T.);
#3504=FACE_OUTER_BOUND('',#5098,.T.);
#3505=FACE_OUTER_BOUND('',#5099,.T.);
#3506=FACE_OUTER_BOUND('',#5100,.T.);
#3507=FACE_OUTER_BOUND('',#5101,.T.);
#3508=FACE_OUTER_BOUND('',#5102,.T.);
#3509=FACE_OUTER_BOUND('',#5103,.T.);
#3510=FACE_OUTER_BOUND('',#5104,.T.);
#3511=FACE_OUTER_BOUND('',#5105,.T.);
#3512=FACE_OUTER_BOUND('',#5106,.T.);
#3513=FACE_OUTER_BOUND('',#5107,.T.);
#3514=FACE_OUTER_BOUND('',#5108,.T.);
#3515=FACE_OUTER_BOUND('',#5109,.T.);
#3516=FACE_OUTER_BOUND('',#5110,.T.);
#3517=FACE_OUTER_BOUND('',#5111,.T.);
#3518=FACE_OUTER_BOUND('',#5112,.T.);
#3519=FACE_OUTER_BOUND('',#5113,.T.);
#3520=FACE_OUTER_BOUND('',#5114,.T.);
#3521=FACE_OUTER_BOUND('',#5116,.T.);
#3522=FACE_OUTER_BOUND('',#5117,.T.);
#3523=FACE_OUTER_BOUND('',#5118,.T.);
#3524=FACE_OUTER_BOUND('',#5119,.T.);
#3525=FACE_OUTER_BOUND('',#5120,.T.);
#3526=FACE_OUTER_BOUND('',#5122,.T.);
#3527=FACE_OUTER_BOUND('',#5124,.T.);
#3528=FACE_OUTER_BOUND('',#5125,.T.);
#3529=FACE_OUTER_BOUND('',#5126,.T.);
#3530=FACE_OUTER_BOUND('',#5127,.T.);
#3531=FACE_OUTER_BOUND('',#5128,.T.);
#3532=FACE_OUTER_BOUND('',#5129,.T.);
#3533=FACE_OUTER_BOUND('',#5130,.T.);
#3534=FACE_OUTER_BOUND('',#5131,.T.);
#3535=FACE_OUTER_BOUND('',#5132,.T.);
#3536=FACE_OUTER_BOUND('',#5133,.T.);
#3537=FACE_OUTER_BOUND('',#5134,.T.);
#3538=FACE_OUTER_BOUND('',#5135,.T.);
#3539=FACE_OUTER_BOUND('',#5136,.T.);
#3540=FACE_OUTER_BOUND('',#5137,.T.);
#3541=FACE_OUTER_BOUND('',#5138,.T.);
#3542=FACE_OUTER_BOUND('',#5139,.T.);
#3543=FACE_OUTER_BOUND('',#5140,.T.);
#3544=FACE_OUTER_BOUND('',#5141,.T.);
#3545=FACE_OUTER_BOUND('',#5142,.T.);
#3546=FACE_OUTER_BOUND('',#5143,.T.);
#3547=FACE_OUTER_BOUND('',#5144,.T.);
#3548=FACE_OUTER_BOUND('',#5145,.T.);
#3549=FACE_OUTER_BOUND('',#5146,.T.);
#3550=FACE_OUTER_BOUND('',#5147,.T.);
#3551=FACE_OUTER_BOUND('',#5148,.T.);
#3552=FACE_OUTER_BOUND('',#5149,.T.);
#3553=FACE_OUTER_BOUND('',#5150,.T.);
#3554=FACE_OUTER_BOUND('',#5151,.T.);
#3555=FACE_OUTER_BOUND('',#5152,.T.);
#3556=FACE_OUTER_BOUND('',#5153,.T.);
#3557=FACE_OUTER_BOUND('',#5154,.T.);
#3558=FACE_OUTER_BOUND('',#5155,.T.);
#3559=FACE_OUTER_BOUND('',#5156,.T.);
#3560=FACE_OUTER_BOUND('',#5157,.T.);
#3561=FACE_OUTER_BOUND('',#5158,.T.);
#3562=FACE_OUTER_BOUND('',#5159,.T.);
#3563=FACE_OUTER_BOUND('',#5160,.T.);
#3564=FACE_OUTER_BOUND('',#5161,.T.);
#3565=FACE_OUTER_BOUND('',#5162,.T.);
#3566=FACE_OUTER_BOUND('',#5163,.T.);
#3567=FACE_OUTER_BOUND('',#5164,.T.);
#3568=FACE_OUTER_BOUND('',#5165,.T.);
#3569=FACE_OUTER_BOUND('',#5166,.T.);
#3570=FACE_OUTER_BOUND('',#5167,.T.);
#3571=FACE_OUTER_BOUND('',#5168,.T.);
#3572=FACE_OUTER_BOUND('',#5169,.T.);
#3573=FACE_OUTER_BOUND('',#5170,.T.);
#3574=FACE_OUTER_BOUND('',#5171,.T.);
#3575=FACE_OUTER_BOUND('',#5172,.T.);
#3576=FACE_OUTER_BOUND('',#5173,.T.);
#3577=FACE_OUTER_BOUND('',#5174,.T.);
#3578=FACE_OUTER_BOUND('',#5175,.T.);
#3579=FACE_OUTER_BOUND('',#5176,.T.);
#3580=FACE_OUTER_BOUND('',#5177,.T.);
#3581=FACE_OUTER_BOUND('',#5178,.T.);
#3582=FACE_OUTER_BOUND('',#5179,.T.);
#3583=FACE_OUTER_BOUND('',#5180,.T.);
#3584=FACE_OUTER_BOUND('',#5181,.T.);
#3585=FACE_OUTER_BOUND('',#5182,.T.);
#3586=FACE_OUTER_BOUND('',#5183,.T.);
#3587=FACE_OUTER_BOUND('',#5184,.T.);
#3588=FACE_OUTER_BOUND('',#5185,.T.);
#3589=FACE_OUTER_BOUND('',#5186,.T.);
#3590=FACE_OUTER_BOUND('',#5187,.T.);
#3591=FACE_OUTER_BOUND('',#5188,.T.);
#3592=FACE_OUTER_BOUND('',#5189,.T.);
#3593=FACE_OUTER_BOUND('',#5190,.T.);
#3594=FACE_OUTER_BOUND('',#5191,.T.);
#3595=FACE_OUTER_BOUND('',#5192,.T.);
#3596=FACE_OUTER_BOUND('',#5193,.T.);
#3597=FACE_OUTER_BOUND('',#5194,.T.);
#3598=FACE_OUTER_BOUND('',#5195,.T.);
#3599=FACE_OUTER_BOUND('',#5196,.T.);
#3600=FACE_OUTER_BOUND('',#5197,.T.);
#3601=FACE_OUTER_BOUND('',#5198,.T.);
#3602=FACE_OUTER_BOUND('',#5199,.T.);
#3603=FACE_OUTER_BOUND('',#5200,.T.);
#3604=FACE_OUTER_BOUND('',#5201,.T.);
#3605=FACE_OUTER_BOUND('',#5202,.T.);
#3606=FACE_OUTER_BOUND('',#5203,.T.);
#3607=FACE_OUTER_BOUND('',#5204,.T.);
#3608=FACE_OUTER_BOUND('',#5205,.T.);
#3609=FACE_OUTER_BOUND('',#5206,.T.);
#3610=FACE_OUTER_BOUND('',#5207,.T.);
#3611=FACE_OUTER_BOUND('',#5208,.T.);
#3612=FACE_OUTER_BOUND('',#5209,.T.);
#3613=FACE_OUTER_BOUND('',#5210,.T.);
#3614=FACE_OUTER_BOUND('',#5211,.T.);
#3615=FACE_OUTER_BOUND('',#5212,.T.);
#3616=FACE_OUTER_BOUND('',#5213,.T.);
#3617=FACE_OUTER_BOUND('',#5214,.T.);
#3618=FACE_OUTER_BOUND('',#5215,.T.);
#3619=FACE_OUTER_BOUND('',#5216,.T.);
#3620=FACE_OUTER_BOUND('',#5217,.T.);
#3621=FACE_OUTER_BOUND('',#5218,.T.);
#3622=FACE_OUTER_BOUND('',#5219,.T.);
#3623=FACE_OUTER_BOUND('',#5220,.T.);
#3624=FACE_OUTER_BOUND('',#5221,.T.);
#3625=FACE_OUTER_BOUND('',#5222,.T.);
#3626=FACE_OUTER_BOUND('',#5223,.T.);
#3627=FACE_OUTER_BOUND('',#5224,.T.);
#3628=FACE_OUTER_BOUND('',#5225,.T.);
#3629=FACE_OUTER_BOUND('',#5226,.T.);
#3630=FACE_OUTER_BOUND('',#5227,.T.);
#3631=FACE_OUTER_BOUND('',#5228,.T.);
#3632=FACE_OUTER_BOUND('',#5229,.T.);
#3633=FACE_OUTER_BOUND('',#5230,.T.);
#3634=FACE_OUTER_BOUND('',#5231,.T.);
#3635=FACE_OUTER_BOUND('',#5232,.T.);
#3636=FACE_OUTER_BOUND('',#5233,.T.);
#3637=FACE_OUTER_BOUND('',#5234,.T.);
#3638=FACE_OUTER_BOUND('',#5235,.T.);
#3639=FACE_OUTER_BOUND('',#5236,.T.);
#3640=FACE_OUTER_BOUND('',#5237,.T.);
#3641=FACE_OUTER_BOUND('',#5238,.T.);
#3642=FACE_OUTER_BOUND('',#5239,.T.);
#3643=FACE_OUTER_BOUND('',#5240,.T.);
#3644=FACE_OUTER_BOUND('',#5241,.T.);
#3645=FACE_OUTER_BOUND('',#5242,.T.);
#3646=FACE_OUTER_BOUND('',#5243,.T.);
#3647=FACE_OUTER_BOUND('',#5244,.T.);
#3648=FACE_OUTER_BOUND('',#5245,.T.);
#3649=FACE_OUTER_BOUND('',#5246,.T.);
#3650=FACE_OUTER_BOUND('',#5247,.T.);
#3651=FACE_OUTER_BOUND('',#5248,.T.);
#3652=FACE_OUTER_BOUND('',#5249,.T.);
#3653=FACE_OUTER_BOUND('',#5250,.T.);
#3654=FACE_OUTER_BOUND('',#5251,.T.);
#3655=FACE_OUTER_BOUND('',#5252,.T.);
#3656=FACE_OUTER_BOUND('',#5253,.T.);
#3657=FACE_OUTER_BOUND('',#5254,.T.);
#3658=FACE_OUTER_BOUND('',#5255,.T.);
#3659=FACE_OUTER_BOUND('',#5256,.T.);
#3660=FACE_OUTER_BOUND('',#5257,.T.);
#3661=FACE_OUTER_BOUND('',#5258,.T.);
#3662=FACE_OUTER_BOUND('',#5259,.T.);
#3663=FACE_OUTER_BOUND('',#5260,.T.);
#3664=FACE_OUTER_BOUND('',#5261,.T.);
#3665=FACE_OUTER_BOUND('',#5262,.T.);
#3666=FACE_OUTER_BOUND('',#5263,.T.);
#3667=FACE_OUTER_BOUND('',#5264,.T.);
#3668=FACE_OUTER_BOUND('',#5265,.T.);
#3669=FACE_OUTER_BOUND('',#5266,.T.);
#3670=FACE_OUTER_BOUND('',#5267,.T.);
#3671=FACE_OUTER_BOUND('',#5268,.T.);
#3672=FACE_OUTER_BOUND('',#5269,.T.);
#3673=FACE_OUTER_BOUND('',#5270,.T.);
#3674=FACE_OUTER_BOUND('',#5271,.T.);
#3675=FACE_OUTER_BOUND('',#5273,.T.);
#3676=FACE_OUTER_BOUND('',#5274,.T.);
#3677=FACE_OUTER_BOUND('',#5275,.T.);
#3678=FACE_OUTER_BOUND('',#5276,.T.);
#3679=FACE_OUTER_BOUND('',#5278,.T.);
#3680=FACE_OUTER_BOUND('',#5280,.T.);
#3681=FACE_OUTER_BOUND('',#5281,.T.);
#3682=FACE_OUTER_BOUND('',#5282,.T.);
#3683=FACE_OUTER_BOUND('',#5283,.T.);
#3684=FACE_OUTER_BOUND('',#5284,.T.);
#3685=FACE_OUTER_BOUND('',#5285,.T.);
#3686=FACE_OUTER_BOUND('',#5286,.T.);
#3687=FACE_OUTER_BOUND('',#5287,.T.);
#3688=FACE_OUTER_BOUND('',#5288,.T.);
#3689=FACE_OUTER_BOUND('',#5289,.T.);
#3690=FACE_OUTER_BOUND('',#5290,.T.);
#3691=FACE_OUTER_BOUND('',#5291,.T.);
#3692=FACE_OUTER_BOUND('',#5292,.T.);
#3693=FACE_OUTER_BOUND('',#5293,.T.);
#3694=FACE_OUTER_BOUND('',#5294,.T.);
#3695=FACE_OUTER_BOUND('',#5295,.T.);
#3696=FACE_OUTER_BOUND('',#5296,.T.);
#3697=FACE_OUTER_BOUND('',#5297,.T.);
#3698=FACE_OUTER_BOUND('',#5298,.T.);
#3699=FACE_OUTER_BOUND('',#5299,.T.);
#3700=FACE_OUTER_BOUND('',#5300,.T.);
#3701=FACE_OUTER_BOUND('',#5301,.T.);
#3702=FACE_OUTER_BOUND('',#5302,.T.);
#3703=FACE_OUTER_BOUND('',#5303,.T.);
#3704=FACE_OUTER_BOUND('',#5304,.T.);
#3705=FACE_OUTER_BOUND('',#5305,.T.);
#3706=FACE_OUTER_BOUND('',#5307,.T.);
#3707=FACE_OUTER_BOUND('',#5308,.T.);
#3708=FACE_OUTER_BOUND('',#5309,.T.);
#3709=FACE_OUTER_BOUND('',#5310,.T.);
#3710=FACE_OUTER_BOUND('',#5311,.T.);
#3711=FACE_OUTER_BOUND('',#5312,.T.);
#3712=FACE_OUTER_BOUND('',#5313,.T.);
#3713=FACE_OUTER_BOUND('',#5314,.T.);
#3714=FACE_OUTER_BOUND('',#5315,.T.);
#3715=FACE_OUTER_BOUND('',#5316,.T.);
#3716=FACE_OUTER_BOUND('',#5317,.T.);
#3717=FACE_OUTER_BOUND('',#5319,.T.);
#3718=FACE_OUTER_BOUND('',#5320,.T.);
#3719=FACE_OUTER_BOUND('',#5321,.T.);
#3720=FACE_OUTER_BOUND('',#5322,.T.);
#3721=FACE_OUTER_BOUND('',#5323,.T.);
#3722=FACE_OUTER_BOUND('',#5324,.T.);
#3723=FACE_OUTER_BOUND('',#5325,.T.);
#3724=FACE_OUTER_BOUND('',#5326,.T.);
#3725=FACE_OUTER_BOUND('',#5327,.T.);
#3726=FACE_OUTER_BOUND('',#5328,.T.);
#3727=FACE_OUTER_BOUND('',#5329,.T.);
#3728=FACE_OUTER_BOUND('',#5330,.T.);
#3729=FACE_OUTER_BOUND('',#5331,.T.);
#3730=FACE_OUTER_BOUND('',#5332,.T.);
#3731=FACE_OUTER_BOUND('',#5333,.T.);
#3732=FACE_OUTER_BOUND('',#5334,.T.);
#3733=FACE_OUTER_BOUND('',#5335,.T.);
#3734=FACE_OUTER_BOUND('',#5336,.T.);
#3735=FACE_OUTER_BOUND('',#5337,.T.);
#3736=FACE_OUTER_BOUND('',#5338,.T.);
#3737=FACE_OUTER_BOUND('',#5339,.T.);
#3738=FACE_OUTER_BOUND('',#5340,.T.);
#3739=FACE_OUTER_BOUND('',#5341,.T.);
#3740=FACE_OUTER_BOUND('',#5342,.T.);
#3741=FACE_OUTER_BOUND('',#5343,.T.);
#3742=FACE_OUTER_BOUND('',#5344,.T.);
#3743=FACE_OUTER_BOUND('',#5345,.T.);
#3744=FACE_OUTER_BOUND('',#5346,.T.);
#3745=FACE_OUTER_BOUND('',#5347,.T.);
#3746=FACE_OUTER_BOUND('',#5348,.T.);
#3747=FACE_OUTER_BOUND('',#5349,.T.);
#3748=FACE_OUTER_BOUND('',#5350,.T.);
#3749=FACE_OUTER_BOUND('',#5351,.T.);
#3750=FACE_OUTER_BOUND('',#5352,.T.);
#3751=FACE_OUTER_BOUND('',#5353,.T.);
#3752=FACE_OUTER_BOUND('',#5354,.T.);
#3753=FACE_OUTER_BOUND('',#5355,.T.);
#3754=FACE_OUTER_BOUND('',#5356,.T.);
#3755=FACE_OUTER_BOUND('',#5357,.T.);
#3756=FACE_OUTER_BOUND('',#5358,.T.);
#3757=FACE_OUTER_BOUND('',#5359,.T.);
#3758=FACE_OUTER_BOUND('',#5360,.T.);
#3759=FACE_OUTER_BOUND('',#5361,.T.);
#3760=FACE_OUTER_BOUND('',#5362,.T.);
#3761=FACE_OUTER_BOUND('',#5363,.T.);
#3762=FACE_OUTER_BOUND('',#5364,.T.);
#3763=FACE_OUTER_BOUND('',#5365,.T.);
#3764=FACE_OUTER_BOUND('',#5367,.T.);
#3765=FACE_OUTER_BOUND('',#5368,.T.);
#3766=FACE_OUTER_BOUND('',#5369,.T.);
#3767=FACE_OUTER_BOUND('',#5370,.T.);
#3768=FACE_OUTER_BOUND('',#5371,.T.);
#3769=FACE_OUTER_BOUND('',#5372,.T.);
#3770=FACE_OUTER_BOUND('',#5373,.T.);
#3771=FACE_OUTER_BOUND('',#5374,.T.);
#3772=FACE_OUTER_BOUND('',#5375,.T.);
#3773=FACE_OUTER_BOUND('',#5376,.T.);
#3774=FACE_OUTER_BOUND('',#5378,.T.);
#3775=FACE_OUTER_BOUND('',#5379,.T.);
#3776=EDGE_LOOP('',(#15886,#15887,#15888,#15889,#15890));
#3777=EDGE_LOOP('',(#15891,#15892,#15893,#15894));
#3778=EDGE_LOOP('',(#15895,#15896,#15897,#15898,#15899));
#3779=EDGE_LOOP('',(#15900,#15901,#15902,#15903));
#3780=EDGE_LOOP('',(#15904,#15905,#15906,#15907));
#3781=EDGE_LOOP('',(#15908));
#3782=EDGE_LOOP('',(#15909));
#3783=EDGE_LOOP('',(#15910));
#3784=EDGE_LOOP('',(#15911));
#3785=EDGE_LOOP('',(#15912));
#3786=EDGE_LOOP('',(#15913));
#3787=EDGE_LOOP('',(#15914));
#3788=EDGE_LOOP('',(#15915));
#3789=EDGE_LOOP('',(#15916,#15917,#15918,#15919));
#3790=EDGE_LOOP('',(#15920));
#3791=EDGE_LOOP('',(#15921));
#3792=EDGE_LOOP('',(#15922));
#3793=EDGE_LOOP('',(#15923));
#3794=EDGE_LOOP('',(#15924));
#3795=EDGE_LOOP('',(#15925));
#3796=EDGE_LOOP('',(#15926));
#3797=EDGE_LOOP('',(#15927));
#3798=EDGE_LOOP('',(#15928,#15929,#15930,#15931));
#3799=EDGE_LOOP('',(#15932,#15933,#15934,#15935));
#3800=EDGE_LOOP('',(#15936,#15937,#15938,#15939,#15940));
#3801=EDGE_LOOP('',(#15941,#15942,#15943,#15944,#15945,#15946));
#3802=EDGE_LOOP('',(#15947,#15948,#15949,#15950,#15951));
#3803=EDGE_LOOP('',(#15952,#15953,#15954,#15955));
#3804=EDGE_LOOP('',(#15956,#15957,#15958,#15959));
#3805=EDGE_LOOP('',(#15960));
#3806=EDGE_LOOP('',(#15961));
#3807=EDGE_LOOP('',(#15962));
#3808=EDGE_LOOP('',(#15963));
#3809=EDGE_LOOP('',(#15964));
#3810=EDGE_LOOP('',(#15965,#15966,#15967,#15968,#15969));
#3811=EDGE_LOOP('',(#15970,#15971,#15972,#15973,#15974));
#3812=EDGE_LOOP('',(#15975,#15976,#15977,#15978,#15979));
#3813=EDGE_LOOP('',(#15980,#15981,#15982,#15983,#15984));
#3814=EDGE_LOOP('',(#15985,#15986,#15987,#15988,#15989));
#3815=EDGE_LOOP('',(#15990,#15991,#15992,#15993,#15994));
#3816=EDGE_LOOP('',(#15995,#15996,#15997,#15998,#15999));
#3817=EDGE_LOOP('',(#16000,#16001,#16002,#16003,#16004));
#3818=EDGE_LOOP('',(#16005,#16006,#16007,#16008,#16009));
#3819=EDGE_LOOP('',(#16010,#16011,#16012,#16013,#16014));
#3820=EDGE_LOOP('',(#16015,#16016,#16017,#16018,#16019));
#3821=EDGE_LOOP('',(#16020,#16021,#16022,#16023,#16024));
#3822=EDGE_LOOP('',(#16025,#16026,#16027,#16028,#16029));
#3823=EDGE_LOOP('',(#16030,#16031,#16032,#16033,#16034));
#3824=EDGE_LOOP('',(#16035,#16036,#16037,#16038));
#3825=EDGE_LOOP('',(#16039));
#3826=EDGE_LOOP('',(#16040));
#3827=EDGE_LOOP('',(#16041,#16042,#16043,#16044));
#3828=EDGE_LOOP('',(#16045));
#3829=EDGE_LOOP('',(#16046));
#3830=EDGE_LOOP('',(#16047,#16048,#16049,#16050));
#3831=EDGE_LOOP('',(#16051,#16052,#16053));
#3832=EDGE_LOOP('',(#16054,#16055,#16056,#16057));
#3833=EDGE_LOOP('',(#16058,#16059,#16060,#16061));
#3834=EDGE_LOOP('',(#16062,#16063,#16064));
#3835=EDGE_LOOP('',(#16065,#16066,#16067,#16068));
#3836=EDGE_LOOP('',(#16069,#16070,#16071,#16072));
#3837=EDGE_LOOP('',(#16073,#16074,#16075));
#3838=EDGE_LOOP('',(#16076,#16077,#16078,#16079));
#3839=EDGE_LOOP('',(#16080,#16081,#16082,#16083));
#3840=EDGE_LOOP('',(#16084,#16085,#16086,#16087));
#3841=EDGE_LOOP('',(#16088,#16089,#16090,#16091));
#3842=EDGE_LOOP('',(#16092,#16093,#16094,#16095));
#3843=EDGE_LOOP('',(#16096));
#3844=EDGE_LOOP('',(#16097));
#3845=EDGE_LOOP('',(#16098,#16099,#16100,#16101));
#3846=EDGE_LOOP('',(#16102,#16103,#16104,#16105));
#3847=EDGE_LOOP('',(#16106,#16107,#16108,#16109));
#3848=EDGE_LOOP('',(#16110));
#3849=EDGE_LOOP('',(#16111));
#3850=EDGE_LOOP('',(#16112,#16113,#16114,#16115));
#3851=EDGE_LOOP('',(#16116,#16117,#16118,#16119));
#3852=EDGE_LOOP('',(#16120,#16121,#16122,#16123));
#3853=EDGE_LOOP('',(#16124));
#3854=EDGE_LOOP('',(#16125));
#3855=EDGE_LOOP('',(#16126,#16127,#16128,#16129));
#3856=EDGE_LOOP('',(#16130,#16131,#16132,#16133));
#3857=EDGE_LOOP('',(#16134,#16135,#16136,#16137));
#3858=EDGE_LOOP('',(#16138));
#3859=EDGE_LOOP('',(#16139));
#3860=EDGE_LOOP('',(#16140,#16141,#16142,#16143));
#3861=EDGE_LOOP('',(#16144,#16145,#16146,#16147));
#3862=EDGE_LOOP('',(#16148,#16149,#16150,#16151));
#3863=EDGE_LOOP('',(#16152));
#3864=EDGE_LOOP('',(#16153));
#3865=EDGE_LOOP('',(#16154,#16155,#16156,#16157));
#3866=EDGE_LOOP('',(#16158,#16159,#16160,#16161));
#3867=EDGE_LOOP('',(#16162,#16163,#16164,#16165));
#3868=EDGE_LOOP('',(#16166));
#3869=EDGE_LOOP('',(#16167));
#3870=EDGE_LOOP('',(#16168,#16169,#16170,#16171,#16172));
#3871=EDGE_LOOP('',(#16173,#16174,#16175,#16176,#16177));
#3872=EDGE_LOOP('',(#16178,#16179,#16180));
#3873=EDGE_LOOP('',(#16181,#16182,#16183,#16184));
#3874=EDGE_LOOP('',(#16185,#16186,#16187,#16188));
#3875=EDGE_LOOP('',(#16189,#16190,#16191));
#3876=EDGE_LOOP('',(#16192,#16193,#16194,#16195));
#3877=EDGE_LOOP('',(#16196,#16197,#16198,#16199));
#3878=EDGE_LOOP('',(#16200,#16201,#16202));
#3879=EDGE_LOOP('',(#16203,#16204,#16205,#16206));
#3880=EDGE_LOOP('',(#16207,#16208,#16209,#16210));
#3881=EDGE_LOOP('',(#16211,#16212,#16213));
#3882=EDGE_LOOP('',(#16214,#16215,#16216,#16217));
#3883=EDGE_LOOP('',(#16218,#16219,#16220,#16221));
#3884=EDGE_LOOP('',(#16222,#16223,#16224));
#3885=EDGE_LOOP('',(#16225,#16226,#16227,#16228));
#3886=EDGE_LOOP('',(#16229,#16230,#16231,#16232));
#3887=EDGE_LOOP('',(#16233,#16234,#16235));
#3888=EDGE_LOOP('',(#16236,#16237,#16238,#16239));
#3889=EDGE_LOOP('',(#16240,#16241,#16242,#16243));
#3890=EDGE_LOOP('',(#16244,#16245,#16246));
#3891=EDGE_LOOP('',(#16247,#16248,#16249,#16250));
#3892=EDGE_LOOP('',(#16251,#16252,#16253,#16254));
#3893=EDGE_LOOP('',(#16255,#16256,#16257));
#3894=EDGE_LOOP('',(#16258,#16259,#16260,#16261));
#3895=EDGE_LOOP('',(#16262,#16263,#16264,#16265));
#3896=EDGE_LOOP('',(#16266,#16267,#16268));
#3897=EDGE_LOOP('',(#16269,#16270,#16271,#16272));
#3898=EDGE_LOOP('',(#16273,#16274,#16275,#16276));
#3899=EDGE_LOOP('',(#16277,#16278,#16279));
#3900=EDGE_LOOP('',(#16280,#16281,#16282,#16283));
#3901=EDGE_LOOP('',(#16284,#16285,#16286,#16287));
#3902=EDGE_LOOP('',(#16288,#16289,#16290));
#3903=EDGE_LOOP('',(#16291,#16292,#16293,#16294));
#3904=EDGE_LOOP('',(#16295,#16296,#16297,#16298));
#3905=EDGE_LOOP('',(#16299,#16300,#16301));
#3906=EDGE_LOOP('',(#16302,#16303,#16304,#16305));
#3907=EDGE_LOOP('',(#16306,#16307,#16308,#16309));
#3908=EDGE_LOOP('',(#16310,#16311,#16312));
#3909=EDGE_LOOP('',(#16313,#16314,#16315,#16316));
#3910=EDGE_LOOP('',(#16317,#16318,#16319,#16320));
#3911=EDGE_LOOP('',(#16321,#16322,#16323));
#3912=EDGE_LOOP('',(#16324,#16325,#16326,#16327));
#3913=EDGE_LOOP('',(#16328,#16329,#16330,#16331));
#3914=EDGE_LOOP('',(#16332,#16333,#16334));
#3915=EDGE_LOOP('',(#16335,#16336,#16337,#16338));
#3916=EDGE_LOOP('',(#16339,#16340,#16341,#16342));
#3917=EDGE_LOOP('',(#16343,#16344,#16345));
#3918=EDGE_LOOP('',(#16346,#16347,#16348,#16349));
#3919=EDGE_LOOP('',(#16350,#16351,#16352,#16353));
#3920=EDGE_LOOP('',(#16354,#16355,#16356));
#3921=EDGE_LOOP('',(#16357,#16358,#16359,#16360));
#3922=EDGE_LOOP('',(#16361,#16362,#16363,#16364));
#3923=EDGE_LOOP('',(#16365,#16366,#16367));
#3924=EDGE_LOOP('',(#16368,#16369,#16370,#16371));
#3925=EDGE_LOOP('',(#16372,#16373,#16374,#16375));
#3926=EDGE_LOOP('',(#16376,#16377,#16378,#16379,#16380));
#3927=EDGE_LOOP('',(#16381,#16382,#16383,#16384,#16385,#16386));
#3928=EDGE_LOOP('',(#16387));
#3929=EDGE_LOOP('',(#16388));
#3930=EDGE_LOOP('',(#16389));
#3931=EDGE_LOOP('',(#16390));
#3932=EDGE_LOOP('',(#16391));
#3933=EDGE_LOOP('',(#16392));
#3934=EDGE_LOOP('',(#16393));
#3935=EDGE_LOOP('',(#16394));
#3936=EDGE_LOOP('',(#16395,#16396,#16397,#16398,#16399));
#3937=EDGE_LOOP('',(#16400));
#3938=EDGE_LOOP('',(#16401));
#3939=EDGE_LOOP('',(#16402));
#3940=EDGE_LOOP('',(#16403));
#3941=EDGE_LOOP('',(#16404));
#3942=EDGE_LOOP('',(#16405));
#3943=EDGE_LOOP('',(#16406));
#3944=EDGE_LOOP('',(#16407));
#3945=EDGE_LOOP('',(#16408));
#3946=EDGE_LOOP('',(#16409));
#3947=EDGE_LOOP('',(#16410));
#3948=EDGE_LOOP('',(#16411));
#3949=EDGE_LOOP('',(#16412));
#3950=EDGE_LOOP('',(#16413));
#3951=EDGE_LOOP('',(#16414,#16415,#16416,#16417,#16418));
#3952=EDGE_LOOP('',(#16419,#16420,#16421,#16422,#16423,#16424));
#3953=EDGE_LOOP('',(#16425,#16426,#16427,#16428,#16429));
#3954=EDGE_LOOP('',(#16430,#16431,#16432));
#3955=EDGE_LOOP('',(#16433,#16434,#16435,#16436));
#3956=EDGE_LOOP('',(#16437,#16438,#16439,#16440));
#3957=EDGE_LOOP('',(#16441,#16442,#16443));
#3958=EDGE_LOOP('',(#16444,#16445,#16446,#16447));
#3959=EDGE_LOOP('',(#16448,#16449,#16450,#16451));
#3960=EDGE_LOOP('',(#16452,#16453,#16454));
#3961=EDGE_LOOP('',(#16455,#16456,#16457,#16458));
#3962=EDGE_LOOP('',(#16459,#16460,#16461,#16462));
#3963=EDGE_LOOP('',(#16463,#16464,#16465));
#3964=EDGE_LOOP('',(#16466,#16467,#16468,#16469));
#3965=EDGE_LOOP('',(#16470,#16471,#16472,#16473));
#3966=EDGE_LOOP('',(#16474,#16475,#16476));
#3967=EDGE_LOOP('',(#16477,#16478,#16479,#16480));
#3968=EDGE_LOOP('',(#16481,#16482,#16483,#16484));
#3969=EDGE_LOOP('',(#16485,#16486,#16487,#16488));
#3970=EDGE_LOOP('',(#16489,#16490,#16491,#16492));
#3971=EDGE_LOOP('',(#16493,#16494,#16495,#16496));
#3972=EDGE_LOOP('',(#16497));
#3973=EDGE_LOOP('',(#16498));
#3974=EDGE_LOOP('',(#16499,#16500,#16501,#16502));
#3975=EDGE_LOOP('',(#16503,#16504,#16505,#16506));
#3976=EDGE_LOOP('',(#16507,#16508,#16509,#16510));
#3977=EDGE_LOOP('',(#16511,#16512,#16513,#16514));
#3978=EDGE_LOOP('',(#16515));
#3979=EDGE_LOOP('',(#16516));
#3980=EDGE_LOOP('',(#16517,#16518,#16519,#16520));
#3981=EDGE_LOOP('',(#16521,#16522,#16523,#16524));
#3982=EDGE_LOOP('',(#16525,#16526,#16527,#16528));
#3983=EDGE_LOOP('',(#16529,#16530,#16531,#16532));
#3984=EDGE_LOOP('',(#16533));
#3985=EDGE_LOOP('',(#16534));
#3986=EDGE_LOOP('',(#16535,#16536,#16537,#16538));
#3987=EDGE_LOOP('',(#16539,#16540,#16541,#16542));
#3988=EDGE_LOOP('',(#16543,#16544,#16545,#16546));
#3989=EDGE_LOOP('',(#16547,#16548,#16549,#16550));
#3990=EDGE_LOOP('',(#16551));
#3991=EDGE_LOOP('',(#16552));
#3992=EDGE_LOOP('',(#16553,#16554,#16555,#16556));
#3993=EDGE_LOOP('',(#16557,#16558,#16559,#16560));
#3994=EDGE_LOOP('',(#16561,#16562,#16563,#16564));
#3995=EDGE_LOOP('',(#16565,#16566,#16567,#16568));
#3996=EDGE_LOOP('',(#16569));
#3997=EDGE_LOOP('',(#16570));
#3998=EDGE_LOOP('',(#16571,#16572,#16573,#16574));
#3999=EDGE_LOOP('',(#16575,#16576,#16577,#16578));
#4000=EDGE_LOOP('',(#16579,#16580,#16581,#16582));
#4001=EDGE_LOOP('',(#16583,#16584,#16585,#16586));
#4002=EDGE_LOOP('',(#16587));
#4003=EDGE_LOOP('',(#16588));
#4004=EDGE_LOOP('',(#16589,#16590,#16591,#16592));
#4005=EDGE_LOOP('',(#16593,#16594,#16595,#16596));
#4006=EDGE_LOOP('',(#16597,#16598,#16599,#16600));
#4007=EDGE_LOOP('',(#16601,#16602,#16603,#16604));
#4008=EDGE_LOOP('',(#16605));
#4009=EDGE_LOOP('',(#16606));
#4010=EDGE_LOOP('',(#16607,#16608,#16609,#16610));
#4011=EDGE_LOOP('',(#16611,#16612,#16613,#16614));
#4012=EDGE_LOOP('',(#16615,#16616,#16617,#16618));
#4013=EDGE_LOOP('',(#16619,#16620,#16621,#16622));
#4014=EDGE_LOOP('',(#16623));
#4015=EDGE_LOOP('',(#16624));
#4016=EDGE_LOOP('',(#16625,#16626,#16627,#16628));
#4017=EDGE_LOOP('',(#16629,#16630,#16631,#16632));
#4018=EDGE_LOOP('',(#16633,#16634,#16635,#16636));
#4019=EDGE_LOOP('',(#16637,#16638,#16639,#16640));
#4020=EDGE_LOOP('',(#16641));
#4021=EDGE_LOOP('',(#16642));
#4022=EDGE_LOOP('',(#16643,#16644,#16645,#16646));
#4023=EDGE_LOOP('',(#16647,#16648,#16649,#16650));
#4024=EDGE_LOOP('',(#16651,#16652,#16653,#16654));
#4025=EDGE_LOOP('',(#16655,#16656,#16657,#16658));
#4026=EDGE_LOOP('',(#16659));
#4027=EDGE_LOOP('',(#16660));
#4028=EDGE_LOOP('',(#16661,#16662,#16663,#16664));
#4029=EDGE_LOOP('',(#16665,#16666,#16667,#16668));
#4030=EDGE_LOOP('',(#16669,#16670,#16671,#16672));
#4031=EDGE_LOOP('',(#16673,#16674,#16675,#16676));
#4032=EDGE_LOOP('',(#16677));
#4033=EDGE_LOOP('',(#16678));
#4034=EDGE_LOOP('',(#16679,#16680,#16681,#16682));
#4035=EDGE_LOOP('',(#16683,#16684,#16685,#16686));
#4036=EDGE_LOOP('',(#16687,#16688,#16689,#16690));
#4037=EDGE_LOOP('',(#16691,#16692,#16693,#16694));
#4038=EDGE_LOOP('',(#16695));
#4039=EDGE_LOOP('',(#16696));
#4040=EDGE_LOOP('',(#16697,#16698,#16699,#16700));
#4041=EDGE_LOOP('',(#16701,#16702,#16703,#16704,#16705));
#4042=EDGE_LOOP('',(#16706,#16707,#16708,#16709,#16710,#16711));
#4043=EDGE_LOOP('',(#16712));
#4044=EDGE_LOOP('',(#16713));
#4045=EDGE_LOOP('',(#16714));
#4046=EDGE_LOOP('',(#16715));
#4047=EDGE_LOOP('',(#16716));
#4048=EDGE_LOOP('',(#16717,#16718,#16719,#16720,#16721));
#4049=EDGE_LOOP('',(#16722));
#4050=EDGE_LOOP('',(#16723));
#4051=EDGE_LOOP('',(#16724,#16725,#16726,#16727,#16728));
#4052=EDGE_LOOP('',(#16729,#16730,#16731,#16732,#16733,#16734));
#4053=EDGE_LOOP('',(#16735));
#4054=EDGE_LOOP('',(#16736));
#4055=EDGE_LOOP('',(#16737));
#4056=EDGE_LOOP('',(#16738));
#4057=EDGE_LOOP('',(#16739));
#4058=EDGE_LOOP('',(#16740));
#4059=EDGE_LOOP('',(#16741));
#4060=EDGE_LOOP('',(#16742));
#4061=EDGE_LOOP('',(#16743));
#4062=EDGE_LOOP('',(#16744));
#4063=EDGE_LOOP('',(#16745));
#4064=EDGE_LOOP('',(#16746));
#4065=EDGE_LOOP('',(#16747));
#4066=EDGE_LOOP('',(#16748));
#4067=EDGE_LOOP('',(#16749,#16750,#16751,#16752,#16753));
#4068=EDGE_LOOP('',(#16754));
#4069=EDGE_LOOP('',(#16755));
#4070=EDGE_LOOP('',(#16756));
#4071=EDGE_LOOP('',(#16757));
#4072=EDGE_LOOP('',(#16758));
#4073=EDGE_LOOP('',(#16759));
#4074=EDGE_LOOP('',(#16760));
#4075=EDGE_LOOP('',(#16761));
#4076=EDGE_LOOP('',(#16762,#16763,#16764,#16765,#16766));
#4077=EDGE_LOOP('',(#16767,#16768,#16769,#16770,#16771));
#4078=EDGE_LOOP('',(#16772,#16773,#16774,#16775,#16776));
#4079=EDGE_LOOP('',(#16777,#16778,#16779,#16780,#16781));
#4080=EDGE_LOOP('',(#16782,#16783,#16784,#16785,#16786));
#4081=EDGE_LOOP('',(#16787,#16788,#16789,#16790,#16791));
#4082=EDGE_LOOP('',(#16792,#16793,#16794,#16795,#16796));
#4083=EDGE_LOOP('',(#16797,#16798,#16799,#16800,#16801));
#4084=EDGE_LOOP('',(#16802,#16803,#16804,#16805,#16806));
#4085=EDGE_LOOP('',(#16807,#16808,#16809,#16810,#16811));
#4086=EDGE_LOOP('',(#16812,#16813,#16814,#16815,#16816));
#4087=EDGE_LOOP('',(#16817,#16818,#16819,#16820,#16821));
#4088=EDGE_LOOP('',(#16822,#16823,#16824,#16825,#16826,#16827));
#4089=EDGE_LOOP('',(#16828,#16829,#16830,#16831,#16832,#16833));
#4090=EDGE_LOOP('',(#16834,#16835,#16836,#16837,#16838,#16839));
#4091=EDGE_LOOP('',(#16840,#16841,#16842,#16843,#16844,#16845));
#4092=EDGE_LOOP('',(#16846,#16847,#16848,#16849,#16850,#16851));
#4093=EDGE_LOOP('',(#16852,#16853,#16854,#16855,#16856,#16857));
#4094=EDGE_LOOP('',(#16858,#16859,#16860,#16861,#16862,#16863));
#4095=EDGE_LOOP('',(#16864,#16865,#16866,#16867,#16868,#16869));
#4096=EDGE_LOOP('',(#16870,#16871,#16872,#16873,#16874,#16875));
#4097=EDGE_LOOP('',(#16876,#16877,#16878,#16879,#16880,#16881));
#4098=EDGE_LOOP('',(#16882,#16883,#16884,#16885,#16886,#16887));
#4099=EDGE_LOOP('',(#16888,#16889,#16890,#16891,#16892,#16893));
#4100=EDGE_LOOP('',(#16894,#16895,#16896,#16897,#16898,#16899));
#4101=EDGE_LOOP('',(#16900,#16901,#16902,#16903,#16904,#16905));
#4102=EDGE_LOOP('',(#16906,#16907,#16908,#16909,#16910,#16911));
#4103=EDGE_LOOP('',(#16912,#16913,#16914,#16915,#16916,#16917));
#4104=EDGE_LOOP('',(#16918,#16919,#16920,#16921,#16922,#16923));
#4105=EDGE_LOOP('',(#16924,#16925,#16926,#16927,#16928,#16929));
#4106=EDGE_LOOP('',(#16930));
#4107=EDGE_LOOP('',(#16931));
#4108=EDGE_LOOP('',(#16932));
#4109=EDGE_LOOP('',(#16933));
#4110=EDGE_LOOP('',(#16934));
#4111=EDGE_LOOP('',(#16935));
#4112=EDGE_LOOP('',(#16936));
#4113=EDGE_LOOP('',(#16937));
#4114=EDGE_LOOP('',(#16938,#16939,#16940,#16941));
#4115=EDGE_LOOP('',(#16942,#16943,#16944,#16945));
#4116=EDGE_LOOP('',(#16946,#16947,#16948,#16949));
#4117=EDGE_LOOP('',(#16950,#16951,#16952,#16953));
#4118=EDGE_LOOP('',(#16954,#16955,#16956,#16957,#16958));
#4119=EDGE_LOOP('',(#16959,#16960,#16961,#16962));
#4120=EDGE_LOOP('',(#16963,#16964,#16965,#16966));
#4121=EDGE_LOOP('',(#16967,#16968,#16969,#16970));
#4122=EDGE_LOOP('',(#16971,#16972,#16973,#16974,#16975,#16976));
#4123=EDGE_LOOP('',(#16977,#16978,#16979,#16980));
#4124=EDGE_LOOP('',(#16981,#16982,#16983,#16984));
#4125=EDGE_LOOP('',(#16985,#16986,#16987,#16988));
#4126=EDGE_LOOP('',(#16989,#16990,#16991,#16992));
#4127=EDGE_LOOP('',(#16993,#16994,#16995,#16996));
#4128=EDGE_LOOP('',(#16997,#16998,#16999,#17000,#17001,#17002));
#4129=EDGE_LOOP('',(#17003,#17004,#17005,#17006));
#4130=EDGE_LOOP('',(#17007,#17008,#17009,#17010));
#4131=EDGE_LOOP('',(#17011,#17012,#17013,#17014));
#4132=EDGE_LOOP('',(#17015,#17016,#17017,#17018));
#4133=EDGE_LOOP('',(#17019,#17020,#17021,#17022));
#4134=EDGE_LOOP('',(#17023,#17024,#17025,#17026));
#4135=EDGE_LOOP('',(#17027,#17028,#17029,#17030,#17031,#17032));
#4136=EDGE_LOOP('',(#17033,#17034,#17035,#17036));
#4137=EDGE_LOOP('',(#17037,#17038,#17039,#17040));
#4138=EDGE_LOOP('',(#17041,#17042,#17043,#17044));
#4139=EDGE_LOOP('',(#17045,#17046,#17047,#17048));
#4140=EDGE_LOOP('',(#17049,#17050,#17051,#17052));
#4141=EDGE_LOOP('',(#17053,#17054,#17055,#17056,#17057,#17058));
#4142=EDGE_LOOP('',(#17059,#17060,#17061,#17062));
#4143=EDGE_LOOP('',(#17063,#17064,#17065,#17066));
#4144=EDGE_LOOP('',(#17067,#17068,#17069,#17070));
#4145=EDGE_LOOP('',(#17071,#17072,#17073,#17074));
#4146=EDGE_LOOP('',(#17075,#17076,#17077,#17078));
#4147=EDGE_LOOP('',(#17079,#17080,#17081,#17082,#17083));
#4148=EDGE_LOOP('',(#17084,#17085,#17086,#17087));
#4149=EDGE_LOOP('',(#17088,#17089,#17090,#17091));
#4150=EDGE_LOOP('',(#17092,#17093,#17094,#17095));
#4151=EDGE_LOOP('',(#17096,#17097,#17098,#17099));
#4152=EDGE_LOOP('',(#17100,#17101,#17102,#17103));
#4153=EDGE_LOOP('',(#17104,#17105,#17106,#17107,#17108,#17109));
#4154=EDGE_LOOP('',(#17110,#17111,#17112,#17113));
#4155=EDGE_LOOP('',(#17114,#17115,#17116,#17117));
#4156=EDGE_LOOP('',(#17118,#17119,#17120,#17121));
#4157=EDGE_LOOP('',(#17122,#17123,#17124,#17125));
#4158=EDGE_LOOP('',(#17126,#17127,#17128,#17129));
#4159=EDGE_LOOP('',(#17130,#17131,#17132,#17133,#17134,#17135));
#4160=EDGE_LOOP('',(#17136,#17137,#17138,#17139));
#4161=EDGE_LOOP('',(#17140,#17141,#17142,#17143));
#4162=EDGE_LOOP('',(#17144,#17145,#17146,#17147));
#4163=EDGE_LOOP('',(#17148,#17149,#17150,#17151,#17152));
#4164=EDGE_LOOP('',(#17153,#17154,#17155,#17156));
#4165=EDGE_LOOP('',(#17157,#17158,#17159,#17160));
#4166=EDGE_LOOP('',(#17161,#17162,#17163,#17164));
#4167=EDGE_LOOP('',(#17165,#17166,#17167,#17168));
#4168=EDGE_LOOP('',(#17169,#17170,#17171,#17172));
#4169=EDGE_LOOP('',(#17173,#17174,#17175,#17176));
#4170=EDGE_LOOP('',(#17177,#17178,#17179,#17180,#17181,#17182));
#4171=EDGE_LOOP('',(#17183,#17184,#17185,#17186));
#4172=EDGE_LOOP('',(#17187,#17188,#17189,#17190));
#4173=EDGE_LOOP('',(#17191,#17192,#17193,#17194));
#4174=EDGE_LOOP('',(#17195,#17196,#17197,#17198));
#4175=EDGE_LOOP('',(#17199,#17200,#17201,#17202));
#4176=EDGE_LOOP('',(#17203,#17204,#17205,#17206,#17207,#17208));
#4177=EDGE_LOOP('',(#17209,#17210,#17211,#17212));
#4178=EDGE_LOOP('',(#17213,#17214,#17215,#17216));
#4179=EDGE_LOOP('',(#17217,#17218,#17219,#17220));
#4180=EDGE_LOOP('',(#17221,#17222,#17223,#17224));
#4181=EDGE_LOOP('',(#17225,#17226,#17227,#17228));
#4182=EDGE_LOOP('',(#17229,#17230,#17231,#17232,#17233));
#4183=EDGE_LOOP('',(#17234,#17235,#17236,#17237));
#4184=EDGE_LOOP('',(#17238,#17239,#17240,#17241));
#4185=EDGE_LOOP('',(#17242,#17243,#17244,#17245));
#4186=EDGE_LOOP('',(#17246,#17247,#17248,#17249));
#4187=EDGE_LOOP('',(#17250,#17251,#17252,#17253));
#4188=EDGE_LOOP('',(#17254,#17255,#17256,#17257,#17258,#17259));
#4189=EDGE_LOOP('',(#17260,#17261,#17262,#17263));
#4190=EDGE_LOOP('',(#17264,#17265,#17266,#17267));
#4191=EDGE_LOOP('',(#17268,#17269,#17270,#17271));
#4192=EDGE_LOOP('',(#17272,#17273,#17274,#17275));
#4193=EDGE_LOOP('',(#17276,#17277,#17278,#17279));
#4194=EDGE_LOOP('',(#17280,#17281,#17282,#17283,#17284,#17285));
#4195=EDGE_LOOP('',(#17286,#17287,#17288,#17289));
#4196=EDGE_LOOP('',(#17290,#17291,#17292,#17293));
#4197=EDGE_LOOP('',(#17294,#17295,#17296,#17297));
#4198=EDGE_LOOP('',(#17298,#17299,#17300,#17301));
#4199=EDGE_LOOP('',(#17302,#17303,#17304,#17305));
#4200=EDGE_LOOP('',(#17306,#17307,#17308,#17309,#17310,#17311));
#4201=EDGE_LOOP('',(#17312,#17313,#17314,#17315));
#4202=EDGE_LOOP('',(#17316,#17317,#17318,#17319));
#4203=EDGE_LOOP('',(#17320,#17321,#17322,#17323));
#4204=EDGE_LOOP('',(#17324,#17325,#17326,#17327));
#4205=EDGE_LOOP('',(#17328,#17329,#17330,#17331));
#4206=EDGE_LOOP('',(#17332,#17333,#17334,#17335));
#4207=EDGE_LOOP('',(#17336,#17337,#17338,#17339,#17340,#17341));
#4208=EDGE_LOOP('',(#17342,#17343,#17344,#17345));
#4209=EDGE_LOOP('',(#17346,#17347,#17348,#17349));
#4210=EDGE_LOOP('',(#17350,#17351,#17352,#17353));
#4211=EDGE_LOOP('',(#17354,#17355,#17356,#17357));
#4212=EDGE_LOOP('',(#17358,#17359,#17360,#17361));
#4213=EDGE_LOOP('',(#17362,#17363,#17364,#17365,#17366,#17367));
#4214=EDGE_LOOP('',(#17368,#17369,#17370,#17371));
#4215=EDGE_LOOP('',(#17372,#17373,#17374,#17375));
#4216=EDGE_LOOP('',(#17376,#17377,#17378,#17379));
#4217=EDGE_LOOP('',(#17380,#17381,#17382,#17383,#17384));
#4218=EDGE_LOOP('',(#17385,#17386,#17387,#17388));
#4219=EDGE_LOOP('',(#17389,#17390,#17391,#17392));
#4220=EDGE_LOOP('',(#17393,#17394,#17395,#17396));
#4221=EDGE_LOOP('',(#17397,#17398,#17399,#17400));
#4222=EDGE_LOOP('',(#17401,#17402,#17403,#17404));
#4223=EDGE_LOOP('',(#17405,#17406,#17407,#17408));
#4224=EDGE_LOOP('',(#17409,#17410,#17411,#17412,#17413,#17414));
#4225=EDGE_LOOP('',(#17415,#17416,#17417,#17418));
#4226=EDGE_LOOP('',(#17419,#17420,#17421,#17422));
#4227=EDGE_LOOP('',(#17423,#17424,#17425,#17426));
#4228=EDGE_LOOP('',(#17427,#17428,#17429,#17430));
#4229=EDGE_LOOP('',(#17431,#17432,#17433,#17434));
#4230=EDGE_LOOP('',(#17435,#17436,#17437,#17438,#17439,#17440));
#4231=EDGE_LOOP('',(#17441,#17442,#17443,#17444));
#4232=EDGE_LOOP('',(#17445,#17446,#17447,#17448));
#4233=EDGE_LOOP('',(#17449,#17450,#17451,#17452));
#4234=EDGE_LOOP('',(#17453,#17454,#17455,#17456));
#4235=EDGE_LOOP('',(#17457,#17458,#17459,#17460,#17461));
#4236=EDGE_LOOP('',(#17462,#17463,#17464,#17465));
#4237=EDGE_LOOP('',(#17466,#17467,#17468,#17469));
#4238=EDGE_LOOP('',(#17470,#17471,#17472,#17473));
#4239=EDGE_LOOP('',(#17474,#17475,#17476,#17477));
#4240=EDGE_LOOP('',(#17478,#17479,#17480,#17481,#17482,#17483));
#4241=EDGE_LOOP('',(#17484,#17485,#17486,#17487));
#4242=EDGE_LOOP('',(#17488,#17489,#17490,#17491));
#4243=EDGE_LOOP('',(#17492,#17493,#17494,#17495));
#4244=EDGE_LOOP('',(#17496,#17497,#17498,#17499));
#4245=EDGE_LOOP('',(#17500,#17501,#17502,#17503));
#4246=EDGE_LOOP('',(#17504,#17505,#17506,#17507,#17508,#17509));
#4247=EDGE_LOOP('',(#17510,#17511,#17512,#17513));
#4248=EDGE_LOOP('',(#17514,#17515,#17516,#17517));
#4249=EDGE_LOOP('',(#17518,#17519,#17520,#17521));
#4250=EDGE_LOOP('',(#17522,#17523,#17524,#17525));
#4251=EDGE_LOOP('',(#17526,#17527,#17528,#17529));
#4252=EDGE_LOOP('',(#17530,#17531,#17532,#17533,#17534,#17535));
#4253=EDGE_LOOP('',(#17536,#17537,#17538,#17539));
#4254=EDGE_LOOP('',(#17540,#17541,#17542,#17543));
#4255=EDGE_LOOP('',(#17544,#17545,#17546,#17547));
#4256=EDGE_LOOP('',(#17548,#17549,#17550,#17551,#17552));
#4257=EDGE_LOOP('',(#17553,#17554,#17555,#17556));
#4258=EDGE_LOOP('',(#17557,#17558,#17559,#17560));
#4259=EDGE_LOOP('',(#17561,#17562,#17563,#17564));
#4260=EDGE_LOOP('',(#17565,#17566,#17567,#17568));
#4261=EDGE_LOOP('',(#17569,#17570,#17571,#17572,#17573));
#4262=EDGE_LOOP('',(#17574,#17575,#17576,#17577));
#4263=EDGE_LOOP('',(#17578,#17579,#17580,#17581,#17582));
#4264=EDGE_LOOP('',(#17583,#17584,#17585,#17586));
#4265=EDGE_LOOP('',(#17587,#17588,#17589,#17590));
#4266=EDGE_LOOP('',(#17591,#17592,#17593,#17594,#17595));
#4267=EDGE_LOOP('',(#17596,#17597,#17598,#17599));
#4268=EDGE_LOOP('',(#17600,#17601,#17602,#17603,#17604));
#4269=EDGE_LOOP('',(#17605,#17606,#17607,#17608));
#4270=EDGE_LOOP('',(#17609,#17610,#17611,#17612));
#4271=EDGE_LOOP('',(#17613,#17614,#17615,#17616,#17617));
#4272=EDGE_LOOP('',(#17618,#17619,#17620,#17621));
#4273=EDGE_LOOP('',(#17622,#17623,#17624,#17625));
#4274=EDGE_LOOP('',(#17626,#17627,#17628,#17629));
#4275=EDGE_LOOP('',(#17630,#17631,#17632,#17633));
#4276=EDGE_LOOP('',(#17634,#17635,#17636,#17637));
#4277=EDGE_LOOP('',(#17638,#17639,#17640,#17641));
#4278=EDGE_LOOP('',(#17642,#17643,#17644,#17645));
#4279=EDGE_LOOP('',(#17646,#17647,#17648,#17649));
#4280=EDGE_LOOP('',(#17650,#17651,#17652,#17653));
#4281=EDGE_LOOP('',(#17654,#17655,#17656,#17657));
#4282=EDGE_LOOP('',(#17658,#17659,#17660,#17661));
#4283=EDGE_LOOP('',(#17662,#17663,#17664,#17665));
#4284=EDGE_LOOP('',(#17666,#17667,#17668,#17669));
#4285=EDGE_LOOP('',(#17670,#17671,#17672,#17673));
#4286=EDGE_LOOP('',(#17674,#17675,#17676,#17677));
#4287=EDGE_LOOP('',(#17678,#17679,#17680,#17681));
#4288=EDGE_LOOP('',(#17682,#17683,#17684,#17685));
#4289=EDGE_LOOP('',(#17686,#17687,#17688,#17689));
#4290=EDGE_LOOP('',(#17690,#17691,#17692,#17693));
#4291=EDGE_LOOP('',(#17694,#17695,#17696,#17697));
#4292=EDGE_LOOP('',(#17698,#17699,#17700,#17701));
#4293=EDGE_LOOP('',(#17702,#17703,#17704,#17705));
#4294=EDGE_LOOP('',(#17706,#17707,#17708,#17709));
#4295=EDGE_LOOP('',(#17710,#17711,#17712,#17713));
#4296=EDGE_LOOP('',(#17714,#17715,#17716,#17717));
#4297=EDGE_LOOP('',(#17718,#17719,#17720,#17721));
#4298=EDGE_LOOP('',(#17722,#17723,#17724,#17725));
#4299=EDGE_LOOP('',(#17726,#17727,#17728,#17729));
#4300=EDGE_LOOP('',(#17730,#17731,#17732,#17733));
#4301=EDGE_LOOP('',(#17734,#17735,#17736,#17737));
#4302=EDGE_LOOP('',(#17738,#17739,#17740,#17741));
#4303=EDGE_LOOP('',(#17742,#17743,#17744,#17745));
#4304=EDGE_LOOP('',(#17746,#17747,#17748,#17749));
#4305=EDGE_LOOP('',(#17750,#17751,#17752,#17753));
#4306=EDGE_LOOP('',(#17754,#17755,#17756,#17757));
#4307=EDGE_LOOP('',(#17758,#17759,#17760,#17761));
#4308=EDGE_LOOP('',(#17762,#17763,#17764,#17765));
#4309=EDGE_LOOP('',(#17766,#17767,#17768,#17769));
#4310=EDGE_LOOP('',(#17770,#17771,#17772,#17773));
#4311=EDGE_LOOP('',(#17774,#17775,#17776,#17777));
#4312=EDGE_LOOP('',(#17778,#17779,#17780,#17781));
#4313=EDGE_LOOP('',(#17782));
#4314=EDGE_LOOP('',(#17783));
#4315=EDGE_LOOP('',(#17784,#17785,#17786,#17787));
#4316=EDGE_LOOP('',(#17788,#17789,#17790,#17791));
#4317=EDGE_LOOP('',(#17792,#17793,#17794,#17795,#17796));
#4318=EDGE_LOOP('',(#17797,#17798,#17799,#17800,#17801,#17802));
#4319=EDGE_LOOP('',(#17803));
#4320=EDGE_LOOP('',(#17804));
#4321=EDGE_LOOP('',(#17805,#17806,#17807,#17808,#17809));
#4322=EDGE_LOOP('',(#17810));
#4323=EDGE_LOOP('',(#17811));
#4324=EDGE_LOOP('',(#17812,#17813,#17814,#17815));
#4325=EDGE_LOOP('',(#17816,#17817,#17818,#17819));
#4326=EDGE_LOOP('',(#17820));
#4327=EDGE_LOOP('',(#17821));
#4328=EDGE_LOOP('',(#17822,#17823,#17824,#17825,#17826));
#4329=EDGE_LOOP('',(#17827,#17828,#17829,#17830,#17831,#17832));
#4330=EDGE_LOOP('',(#17833,#17834,#17835,#17836,#17837));
#4331=EDGE_LOOP('',(#17838,#17839,#17840,#17841));
#4332=EDGE_LOOP('',(#17842,#17843,#17844,#17845));
#4333=EDGE_LOOP('',(#17846));
#4334=EDGE_LOOP('',(#17847));
#4335=EDGE_LOOP('',(#17848,#17849,#17850,#17851,#17852));
#4336=EDGE_LOOP('',(#17853,#17854,#17855,#17856,#17857));
#4337=EDGE_LOOP('',(#17858,#17859,#17860,#17861));
#4338=EDGE_LOOP('',(#17862,#17863,#17864,#17865));
#4339=EDGE_LOOP('',(#17866,#17867,#17868,#17869));
#4340=EDGE_LOOP('',(#17870,#17871,#17872,#17873));
#4341=EDGE_LOOP('',(#17874,#17875,#17876,#17877));
#4342=EDGE_LOOP('',(#17878,#17879,#17880,#17881,#17882));
#4343=EDGE_LOOP('',(#17883));
#4344=EDGE_LOOP('',(#17884));
#4345=EDGE_LOOP('',(#17885));
#4346=EDGE_LOOP('',(#17886));
#4347=EDGE_LOOP('',(#17887,#17888,#17889,#17890,#17891));
#4348=EDGE_LOOP('',(#17892,#17893,#17894,#17895));
#4349=EDGE_LOOP('',(#17896,#17897,#17898,#17899));
#4350=EDGE_LOOP('',(#17900,#17901,#17902,#17903,#17904));
#4351=EDGE_LOOP('',(#17905,#17906,#17907,#17908,#17909,#17910));
#4352=EDGE_LOOP('',(#17911,#17912,#17913,#17914,#17915));
#4353=EDGE_LOOP('',(#17916,#17917,#17918,#17919));
#4354=EDGE_LOOP('',(#17920,#17921,#17922,#17923,#17924));
#4355=EDGE_LOOP('',(#17925,#17926,#17927,#17928,#17929,#17930));
#4356=EDGE_LOOP('',(#17931));
#4357=EDGE_LOOP('',(#17932));
#4358=EDGE_LOOP('',(#17933,#17934,#17935,#17936,#17937,#17938,#17939,#17940));
#4359=EDGE_LOOP('',(#17941,#17942,#17943,#17944,#17945,#17946,#17947));
#4360=EDGE_LOOP('',(#17948,#17949,#17950,#17951,#17952));
#4361=EDGE_LOOP('',(#17953,#17954,#17955,#17956,#17957,#17958,#17959));
#4362=EDGE_LOOP('',(#17960,#17961,#17962,#17963,#17964));
#4363=EDGE_LOOP('',(#17965,#17966,#17967,#17968));
#4364=EDGE_LOOP('',(#17969,#17970,#17971,#17972));
#4365=EDGE_LOOP('',(#17973,#17974,#17975,#17976));
#4366=EDGE_LOOP('',(#17977));
#4367=EDGE_LOOP('',(#17978));
#4368=EDGE_LOOP('',(#17979,#17980,#17981,#17982));
#4369=EDGE_LOOP('',(#17983,#17984,#17985,#17986));
#4370=EDGE_LOOP('',(#17987,#17988,#17989,#17990));
#4371=EDGE_LOOP('',(#17991));
#4372=EDGE_LOOP('',(#17992));
#4373=EDGE_LOOP('',(#17993,#17994,#17995,#17996,#17997));
#4374=EDGE_LOOP('',(#17998,#17999,#18000,#18001,#18002,#18003,#18004));
#4375=EDGE_LOOP('',(#18005));
#4376=EDGE_LOOP('',(#18006,#18007,#18008,#18009));
#4377=EDGE_LOOP('',(#18010,#18011,#18012,#18013));
#4378=EDGE_LOOP('',(#18014,#18015,#18016,#18017));
#4379=EDGE_LOOP('',(#18018,#18019,#18020,#18021));
#4380=EDGE_LOOP('',(#18022,#18023,#18024,#18025));
#4381=EDGE_LOOP('',(#18026,#18027,#18028,#18029));
#4382=EDGE_LOOP('',(#18030,#18031,#18032,#18033));
#4383=EDGE_LOOP('',(#18034,#18035,#18036,#18037));
#4384=EDGE_LOOP('',(#18038,#18039,#18040,#18041));
#4385=EDGE_LOOP('',(#18042,#18043,#18044,#18045));
#4386=EDGE_LOOP('',(#18046,#18047,#18048,#18049,#18050));
#4387=EDGE_LOOP('',(#18051,#18052,#18053,#18054,#18055,#18056));
#4388=EDGE_LOOP('',(#18057));
#4389=EDGE_LOOP('',(#18058));
#4390=EDGE_LOOP('',(#18059));
#4391=EDGE_LOOP('',(#18060));
#4392=EDGE_LOOP('',(#18061));
#4393=EDGE_LOOP('',(#18062));
#4394=EDGE_LOOP('',(#18063));
#4395=EDGE_LOOP('',(#18064));
#4396=EDGE_LOOP('',(#18065));
#4397=EDGE_LOOP('',(#18066));
#4398=EDGE_LOOP('',(#18067));
#4399=EDGE_LOOP('',(#18068,#18069,#18070,#18071,#18072));
#4400=EDGE_LOOP('',(#18073));
#4401=EDGE_LOOP('',(#18074));
#4402=EDGE_LOOP('',(#18075));
#4403=EDGE_LOOP('',(#18076));
#4404=EDGE_LOOP('',(#18077));
#4405=EDGE_LOOP('',(#18078));
#4406=EDGE_LOOP('',(#18079));
#4407=EDGE_LOOP('',(#18080));
#4408=EDGE_LOOP('',(#18081));
#4409=EDGE_LOOP('',(#18082));
#4410=EDGE_LOOP('',(#18083));
#4411=EDGE_LOOP('',(#18084,#18085,#18086,#18087,#18088));
#4412=EDGE_LOOP('',(#18089,#18090,#18091,#18092,#18093,#18094));
#4413=EDGE_LOOP('',(#18095,#18096,#18097,#18098,#18099));
#4414=EDGE_LOOP('',(#18100,#18101,#18102));
#4415=EDGE_LOOP('',(#18103,#18104,#18105,#18106));
#4416=EDGE_LOOP('',(#18107,#18108,#18109));
#4417=EDGE_LOOP('',(#18110,#18111,#18112,#18113));
#4418=EDGE_LOOP('',(#18114,#18115,#18116,#18117));
#4419=EDGE_LOOP('',(#18118));
#4420=EDGE_LOOP('',(#18119));
#4421=EDGE_LOOP('',(#18120));
#4422=EDGE_LOOP('',(#18121,#18122,#18123,#18124));
#4423=EDGE_LOOP('',(#18125,#18126,#18127,#18128));
#4424=EDGE_LOOP('',(#18129,#18130,#18131,#18132));
#4425=EDGE_LOOP('',(#18133));
#4426=EDGE_LOOP('',(#18134));
#4427=EDGE_LOOP('',(#18135));
#4428=EDGE_LOOP('',(#18136));
#4429=EDGE_LOOP('',(#18137,#18138,#18139,#18140));
#4430=EDGE_LOOP('',(#18141));
#4431=EDGE_LOOP('',(#18142));
#4432=EDGE_LOOP('',(#18143,#18144,#18145,#18146));
#4433=EDGE_LOOP('',(#18147,#18148,#18149,#18150));
#4434=EDGE_LOOP('',(#18151,#18152,#18153,#18154));
#4435=EDGE_LOOP('',(#18155));
#4436=EDGE_LOOP('',(#18156));
#4437=EDGE_LOOP('',(#18157));
#4438=EDGE_LOOP('',(#18158));
#4439=EDGE_LOOP('',(#18159,#18160,#18161,#18162));
#4440=EDGE_LOOP('',(#18163));
#4441=EDGE_LOOP('',(#18164));
#4442=EDGE_LOOP('',(#18165,#18166,#18167,#18168));
#4443=EDGE_LOOP('',(#18169,#18170,#18171,#18172));
#4444=EDGE_LOOP('',(#18173));
#4445=EDGE_LOOP('',(#18174,#18175,#18176,#18177,#18178));
#4446=EDGE_LOOP('',(#18179));
#4447=EDGE_LOOP('',(#18180));
#4448=EDGE_LOOP('',(#18181,#18182,#18183,#18184,#18185));
#4449=EDGE_LOOP('',(#18186,#18187,#18188,#18189,#18190));
#4450=EDGE_LOOP('',(#18191,#18192,#18193,#18194,#18195,#18196,#18197,#18198,
#18199,#18200,#18201));
#4451=EDGE_LOOP('',(#18202,#18203,#18204,#18205,#18206,#18207,#18208));
#4452=EDGE_LOOP('',(#18209,#18210,#18211,#18212,#18213,#18214,#18215));
#4453=EDGE_LOOP('',(#18216));
#4454=EDGE_LOOP('',(#18217));
#4455=EDGE_LOOP('',(#18218,#18219,#18220,#18221,#18222,#18223,#18224,#18225,
#18226,#18227));
#4456=EDGE_LOOP('',(#18228,#18229,#18230,#18231,#18232));
#4457=EDGE_LOOP('',(#18233,#18234,#18235,#18236,#18237,#18238));
#4458=EDGE_LOOP('',(#18239,#18240,#18241,#18242,#18243,#18244,#18245,#18246,
#18247));
#4459=EDGE_LOOP('',(#18248,#18249,#18250,#18251));
#4460=EDGE_LOOP('',(#18252,#18253,#18254,#18255));
#4461=EDGE_LOOP('',(#18256,#18257,#18258,#18259));
#4462=EDGE_LOOP('',(#18260));
#4463=EDGE_LOOP('',(#18261));
#4464=EDGE_LOOP('',(#18262,#18263));
#4465=EDGE_LOOP('',(#18264));
#4466=EDGE_LOOP('',(#18265));
#4467=EDGE_LOOP('',(#18266,#18267,#18268,#18269));
#4468=EDGE_LOOP('',(#18270));
#4469=EDGE_LOOP('',(#18271));
#4470=EDGE_LOOP('',(#18272));
#4471=EDGE_LOOP('',(#18273));
#4472=EDGE_LOOP('',(#18274));
#4473=EDGE_LOOP('',(#18275,#18276,#18277,#18278));
#4474=EDGE_LOOP('',(#18279,#18280,#18281,#18282));
#4475=EDGE_LOOP('',(#18283,#18284,#18285,#18286));
#4476=EDGE_LOOP('',(#18287,#18288,#18289,#18290));
#4477=EDGE_LOOP('',(#18291,#18292,#18293,#18294));
#4478=EDGE_LOOP('',(#18295,#18296,#18297,#18298));
#4479=EDGE_LOOP('',(#18299,#18300,#18301,#18302,#18303));
#4480=EDGE_LOOP('',(#18304,#18305,#18306,#18307));
#4481=EDGE_LOOP('',(#18308,#18309,#18310,#18311,#18312));
#4482=EDGE_LOOP('',(#18313,#18314,#18315,#18316,#18317,#18318));
#4483=EDGE_LOOP('',(#18319,#18320,#18321,#18322,#18323));
#4484=EDGE_LOOP('',(#18324,#18325,#18326,#18327,#18328));
#4485=EDGE_LOOP('',(#18329,#18330,#18331,#18332,#18333,#18334));
#4486=EDGE_LOOP('',(#18335,#18336,#18337,#18338,#18339,#18340,#18341,#18342,
#18343));
#4487=EDGE_LOOP('',(#18344));
#4488=EDGE_LOOP('',(#18345,#18346,#18347,#18348,#18349));
#4489=EDGE_LOOP('',(#18350));
#4490=EDGE_LOOP('',(#18351));
#4491=EDGE_LOOP('',(#18352));
#4492=EDGE_LOOP('',(#18353));
#4493=EDGE_LOOP('',(#18354));
#4494=EDGE_LOOP('',(#18355,#18356,#18357,#18358,#18359,#18360,#18361));
#4495=EDGE_LOOP('',(#18362,#18363,#18364,#18365,#18366,#18367));
#4496=EDGE_LOOP('',(#18368,#18369,#18370,#18371,#18372));
#4497=EDGE_LOOP('',(#18373,#18374,#18375,#18376));
#4498=EDGE_LOOP('',(#18377,#18378,#18379,#18380));
#4499=EDGE_LOOP('',(#18381,#18382,#18383,#18384,#18385));
#4500=EDGE_LOOP('',(#18386,#18387,#18388,#18389));
#4501=EDGE_LOOP('',(#18390,#18391,#18392,#18393));
#4502=EDGE_LOOP('',(#18394,#18395,#18396,#18397,#18398));
#4503=EDGE_LOOP('',(#18399,#18400,#18401,#18402));
#4504=EDGE_LOOP('',(#18403,#18404,#18405,#18406));
#4505=EDGE_LOOP('',(#18407,#18408,#18409,#18410,#18411));
#4506=EDGE_LOOP('',(#18412,#18413,#18414,#18415));
#4507=EDGE_LOOP('',(#18416,#18417,#18418,#18419));
#4508=EDGE_LOOP('',(#18420,#18421,#18422,#18423));
#4509=EDGE_LOOP('',(#18424,#18425,#18426,#18427));
#4510=EDGE_LOOP('',(#18428));
#4511=EDGE_LOOP('',(#18429));
#4512=EDGE_LOOP('',(#18430));
#4513=EDGE_LOOP('',(#18431,#18432,#18433,#18434));
#4514=EDGE_LOOP('',(#18435,#18436,#18437,#18438));
#4515=EDGE_LOOP('',(#18439,#18440,#18441,#18442));
#4516=EDGE_LOOP('',(#18443,#18444,#18445,#18446));
#4517=EDGE_LOOP('',(#18447,#18448,#18449,#18450));
#4518=EDGE_LOOP('',(#18451,#18452,#18453,#18454));
#4519=EDGE_LOOP('',(#18455));
#4520=EDGE_LOOP('',(#18456,#18457,#18458,#18459));
#4521=EDGE_LOOP('',(#18460,#18461,#18462,#18463));
#4522=EDGE_LOOP('',(#18464,#18465,#18466,#18467));
#4523=EDGE_LOOP('',(#18468,#18469,#18470,#18471));
#4524=EDGE_LOOP('',(#18472,#18473,#18474,#18475));
#4525=EDGE_LOOP('',(#18476,#18477,#18478,#18479));
#4526=EDGE_LOOP('',(#18480,#18481,#18482,#18483));
#4527=EDGE_LOOP('',(#18484,#18485,#18486,#18487));
#4528=EDGE_LOOP('',(#18488,#18489,#18490,#18491));
#4529=EDGE_LOOP('',(#18492,#18493,#18494,#18495));
#4530=EDGE_LOOP('',(#18496,#18497,#18498,#18499));
#4531=EDGE_LOOP('',(#18500,#18501,#18502,#18503));
#4532=EDGE_LOOP('',(#18504,#18505,#18506,#18507));
#4533=EDGE_LOOP('',(#18508,#18509,#18510,#18511));
#4534=EDGE_LOOP('',(#18512,#18513,#18514,#18515));
#4535=EDGE_LOOP('',(#18516,#18517,#18518,#18519));
#4536=EDGE_LOOP('',(#18520,#18521,#18522,#18523));
#4537=EDGE_LOOP('',(#18524,#18525,#18526,#18527));
#4538=EDGE_LOOP('',(#18528,#18529,#18530,#18531));
#4539=EDGE_LOOP('',(#18532,#18533,#18534,#18535));
#4540=EDGE_LOOP('',(#18536,#18537,#18538,#18539));
#4541=EDGE_LOOP('',(#18540,#18541,#18542,#18543));
#4542=EDGE_LOOP('',(#18544,#18545,#18546,#18547));
#4543=EDGE_LOOP('',(#18548,#18549,#18550,#18551));
#4544=EDGE_LOOP('',(#18552,#18553,#18554,#18555));
#4545=EDGE_LOOP('',(#18556,#18557,#18558,#18559));
#4546=EDGE_LOOP('',(#18560,#18561,#18562,#18563));
#4547=EDGE_LOOP('',(#18564,#18565,#18566,#18567));
#4548=EDGE_LOOP('',(#18568,#18569,#18570,#18571));
#4549=EDGE_LOOP('',(#18572,#18573,#18574,#18575));
#4550=EDGE_LOOP('',(#18576));
#4551=EDGE_LOOP('',(#18577));
#4552=EDGE_LOOP('',(#18578));
#4553=EDGE_LOOP('',(#18579,#18580,#18581,#18582));
#4554=EDGE_LOOP('',(#18583,#18584,#18585,#18586));
#4555=EDGE_LOOP('',(#18587,#18588,#18589,#18590));
#4556=EDGE_LOOP('',(#18591,#18592,#18593,#18594));
#4557=EDGE_LOOP('',(#18595,#18596,#18597,#18598));
#4558=EDGE_LOOP('',(#18599,#18600,#18601,#18602));
#4559=EDGE_LOOP('',(#18603));
#4560=EDGE_LOOP('',(#18604,#18605,#18606,#18607));
#4561=EDGE_LOOP('',(#18608,#18609,#18610,#18611));
#4562=EDGE_LOOP('',(#18612,#18613,#18614,#18615,#18616,#18617,#18618,#18619,
#18620,#18621,#18622,#18623,#18624,#18625,#18626,#18627));
#4563=EDGE_LOOP('',(#18628,#18629,#18630,#18631));
#4564=EDGE_LOOP('',(#18632,#18633,#18634,#18635));
#4565=EDGE_LOOP('',(#18636,#18637,#18638,#18639,#18640,#18641,#18642,#18643,
#18644,#18645,#18646,#18647,#18648,#18649,#18650,#18651));
#4566=EDGE_LOOP('',(#18652,#18653,#18654,#18655));
#4567=EDGE_LOOP('',(#18656,#18657,#18658,#18659));
#4568=EDGE_LOOP('',(#18660,#18661,#18662,#18663));
#4569=EDGE_LOOP('',(#18664,#18665,#18666,#18667));
#4570=EDGE_LOOP('',(#18668,#18669,#18670,#18671));
#4571=EDGE_LOOP('',(#18672,#18673,#18674,#18675));
#4572=EDGE_LOOP('',(#18676,#18677,#18678,#18679));
#4573=EDGE_LOOP('',(#18680,#18681,#18682,#18683));
#4574=EDGE_LOOP('',(#18684,#18685,#18686,#18687));
#4575=EDGE_LOOP('',(#18688,#18689,#18690,#18691));
#4576=EDGE_LOOP('',(#18692,#18693,#18694,#18695));
#4577=EDGE_LOOP('',(#18696));
#4578=EDGE_LOOP('',(#18697));
#4579=EDGE_LOOP('',(#18698,#18699,#18700,#18701));
#4580=EDGE_LOOP('',(#18702,#18703,#18704,#18705));
#4581=EDGE_LOOP('',(#18706,#18707,#18708,#18709));
#4582=EDGE_LOOP('',(#18710,#18711,#18712,#18713));
#4583=EDGE_LOOP('',(#18714,#18715,#18716,#18717));
#4584=EDGE_LOOP('',(#18718,#18719,#18720,#18721));
#4585=EDGE_LOOP('',(#18722,#18723,#18724,#18725));
#4586=EDGE_LOOP('',(#18726));
#4587=EDGE_LOOP('',(#18727));
#4588=EDGE_LOOP('',(#18728,#18729,#18730,#18731));
#4589=EDGE_LOOP('',(#18732,#18733,#18734,#18735));
#4590=EDGE_LOOP('',(#18736,#18737,#18738,#18739));
#4591=EDGE_LOOP('',(#18740,#18741,#18742,#18743));
#4592=EDGE_LOOP('',(#18744,#18745,#18746,#18747));
#4593=EDGE_LOOP('',(#18748,#18749,#18750,#18751));
#4594=EDGE_LOOP('',(#18752,#18753,#18754,#18755));
#4595=EDGE_LOOP('',(#18756,#18757,#18758,#18759));
#4596=EDGE_LOOP('',(#18760,#18761,#18762,#18763));
#4597=EDGE_LOOP('',(#18764,#18765,#18766,#18767));
#4598=EDGE_LOOP('',(#18768,#18769,#18770,#18771));
#4599=EDGE_LOOP('',(#18772,#18773,#18774,#18775));
#4600=EDGE_LOOP('',(#18776,#18777,#18778,#18779));
#4601=EDGE_LOOP('',(#18780,#18781,#18782,#18783));
#4602=EDGE_LOOP('',(#18784,#18785,#18786,#18787));
#4603=EDGE_LOOP('',(#18788,#18789,#18790,#18791,#18792,#18793,#18794,#18795,
#18796,#18797,#18798,#18799));
#4604=EDGE_LOOP('',(#18800,#18801,#18802,#18803));
#4605=EDGE_LOOP('',(#18804,#18805,#18806,#18807));
#4606=EDGE_LOOP('',(#18808,#18809,#18810,#18811));
#4607=EDGE_LOOP('',(#18812,#18813,#18814,#18815));
#4608=EDGE_LOOP('',(#18816,#18817,#18818,#18819));
#4609=EDGE_LOOP('',(#18820,#18821,#18822,#18823));
#4610=EDGE_LOOP('',(#18824,#18825,#18826,#18827));
#4611=EDGE_LOOP('',(#18828,#18829,#18830,#18831,#18832,#18833));
#4612=EDGE_LOOP('',(#18834,#18835));
#4613=EDGE_LOOP('',(#18836,#18837,#18838,#18839,#18840,#18841));
#4614=EDGE_LOOP('',(#18842,#18843,#18844,#18845,#18846));
#4615=EDGE_LOOP('',(#18847,#18848,#18849,#18850,#18851));
#4616=EDGE_LOOP('',(#18852,#18853,#18854,#18855));
#4617=EDGE_LOOP('',(#18856,#18857,#18858,#18859,#18860,#18861,#18862,#18863));
#4618=EDGE_LOOP('',(#18864));
#4619=EDGE_LOOP('',(#18865));
#4620=EDGE_LOOP('',(#18866,#18867,#18868,#18869));
#4621=EDGE_LOOP('',(#18870,#18871,#18872,#18873));
#4622=EDGE_LOOP('',(#18874));
#4623=EDGE_LOOP('',(#18875));
#4624=EDGE_LOOP('',(#18876,#18877,#18878,#18879));
#4625=EDGE_LOOP('',(#18880,#18881,#18882,#18883,#18884,#18885,#18886,#18887,
#18888,#18889));
#4626=EDGE_LOOP('',(#18890,#18891,#18892,#18893));
#4627=EDGE_LOOP('',(#18894,#18895,#18896,#18897));
#4628=EDGE_LOOP('',(#18898,#18899,#18900,#18901));
#4629=EDGE_LOOP('',(#18902,#18903,#18904,#18905));
#4630=EDGE_LOOP('',(#18906,#18907,#18908,#18909));
#4631=EDGE_LOOP('',(#18910,#18911,#18912,#18913));
#4632=EDGE_LOOP('',(#18914,#18915,#18916,#18917));
#4633=EDGE_LOOP('',(#18918,#18919,#18920,#18921));
#4634=EDGE_LOOP('',(#18922,#18923,#18924,#18925));
#4635=EDGE_LOOP('',(#18926,#18927,#18928,#18929));
#4636=EDGE_LOOP('',(#18930,#18931,#18932,#18933));
#4637=EDGE_LOOP('',(#18934,#18935,#18936,#18937));
#4638=EDGE_LOOP('',(#18938));
#4639=EDGE_LOOP('',(#18939,#18940,#18941,#18942));
#4640=EDGE_LOOP('',(#18943,#18944,#18945,#18946));
#4641=EDGE_LOOP('',(#18947,#18948,#18949,#18950));
#4642=EDGE_LOOP('',(#18951,#18952,#18953,#18954));
#4643=EDGE_LOOP('',(#18955,#18956,#18957,#18958));
#4644=EDGE_LOOP('',(#18959,#18960,#18961,#18962));
#4645=EDGE_LOOP('',(#18963,#18964,#18965,#18966));
#4646=EDGE_LOOP('',(#18967,#18968,#18969,#18970));
#4647=EDGE_LOOP('',(#18971,#18972,#18973,#18974));
#4648=EDGE_LOOP('',(#18975,#18976,#18977,#18978));
#4649=EDGE_LOOP('',(#18979,#18980,#18981,#18982));
#4650=EDGE_LOOP('',(#18983,#18984,#18985,#18986));
#4651=EDGE_LOOP('',(#18987,#18988,#18989,#18990));
#4652=EDGE_LOOP('',(#18991,#18992,#18993,#18994));
#4653=EDGE_LOOP('',(#18995,#18996,#18997,#18998));
#4654=EDGE_LOOP('',(#18999,#19000,#19001,#19002));
#4655=EDGE_LOOP('',(#19003,#19004,#19005,#19006));
#4656=EDGE_LOOP('',(#19007,#19008,#19009,#19010));
#4657=EDGE_LOOP('',(#19011,#19012,#19013,#19014));
#4658=EDGE_LOOP('',(#19015,#19016,#19017,#19018));
#4659=EDGE_LOOP('',(#19019,#19020,#19021,#19022));
#4660=EDGE_LOOP('',(#19023,#19024,#19025,#19026));
#4661=EDGE_LOOP('',(#19027,#19028,#19029,#19030));
#4662=EDGE_LOOP('',(#19031,#19032,#19033,#19034));
#4663=EDGE_LOOP('',(#19035));
#4664=EDGE_LOOP('',(#19036));
#4665=EDGE_LOOP('',(#19037));
#4666=EDGE_LOOP('',(#19038));
#4667=EDGE_LOOP('',(#19039));
#4668=EDGE_LOOP('',(#19040,#19041,#19042,#19043));
#4669=EDGE_LOOP('',(#19044));
#4670=EDGE_LOOP('',(#19045,#19046,#19047,#19048));
#4671=EDGE_LOOP('',(#19049,#19050,#19051,#19052));
#4672=EDGE_LOOP('',(#19053,#19054,#19055,#19056));
#4673=EDGE_LOOP('',(#19057,#19058,#19059,#19060));
#4674=EDGE_LOOP('',(#19061,#19062,#19063,#19064));
#4675=EDGE_LOOP('',(#19065));
#4676=EDGE_LOOP('',(#19066));
#4677=EDGE_LOOP('',(#19067));
#4678=EDGE_LOOP('',(#19068));
#4679=EDGE_LOOP('',(#19069));
#4680=EDGE_LOOP('',(#19070,#19071,#19072,#19073));
#4681=EDGE_LOOP('',(#19074,#19075,#19076,#19077,#19078,#19079,#19080,#19081));
#4682=EDGE_LOOP('',(#19082,#19083,#19084,#19085));
#4683=EDGE_LOOP('',(#19086,#19087,#19088,#19089));
#4684=EDGE_LOOP('',(#19090,#19091,#19092,#19093));
#4685=EDGE_LOOP('',(#19094,#19095,#19096,#19097));
#4686=EDGE_LOOP('',(#19098,#19099,#19100,#19101));
#4687=EDGE_LOOP('',(#19102,#19103,#19104,#19105));
#4688=EDGE_LOOP('',(#19106,#19107,#19108,#19109,#19110));
#4689=EDGE_LOOP('',(#19111,#19112,#19113,#19114,#19115,#19116,#19117,#19118,
#19119,#19120,#19121));
#4690=EDGE_LOOP('',(#19122,#19123,#19124,#19125));
#4691=EDGE_LOOP('',(#19126,#19127,#19128,#19129));
#4692=EDGE_LOOP('',(#19130,#19131,#19132,#19133,#19134,#19135,#19136,#19137,
#19138,#19139,#19140,#19141));
#4693=EDGE_LOOP('',(#19142,#19143,#19144,#19145));
#4694=EDGE_LOOP('',(#19146,#19147,#19148));
#4695=EDGE_LOOP('',(#19149,#19150,#19151,#19152));
#4696=EDGE_LOOP('',(#19153,#19154,#19155,#19156));
#4697=EDGE_LOOP('',(#19157,#19158,#19159,#19160));
#4698=EDGE_LOOP('',(#19161,#19162,#19163,#19164));
#4699=EDGE_LOOP('',(#19165,#19166,#19167,#19168));
#4700=EDGE_LOOP('',(#19169,#19170,#19171,#19172));
#4701=EDGE_LOOP('',(#19173,#19174,#19175,#19176,#19177,#19178));
#4702=EDGE_LOOP('',(#19179));
#4703=EDGE_LOOP('',(#19180));
#4704=EDGE_LOOP('',(#19181,#19182,#19183,#19184));
#4705=EDGE_LOOP('',(#19185,#19186,#19187,#19188,#19189,#19190));
#4706=EDGE_LOOP('',(#19191));
#4707=EDGE_LOOP('',(#19192,#19193,#19194,#19195,#19196,#19197));
#4708=EDGE_LOOP('',(#19198,#19199,#19200,#19201,#19202,#19203,#19204,#19205));
#4709=EDGE_LOOP('',(#19206,#19207,#19208,#19209));
#4710=EDGE_LOOP('',(#19210,#19211,#19212,#19213));
#4711=EDGE_LOOP('',(#19214,#19215,#19216,#19217));
#4712=EDGE_LOOP('',(#19218,#19219,#19220,#19221));
#4713=EDGE_LOOP('',(#19222,#19223,#19224,#19225));
#4714=EDGE_LOOP('',(#19226,#19227,#19228,#19229));
#4715=EDGE_LOOP('',(#19230,#19231,#19232,#19233));
#4716=EDGE_LOOP('',(#19234,#19235,#19236,#19237));
#4717=EDGE_LOOP('',(#19238,#19239,#19240,#19241));
#4718=EDGE_LOOP('',(#19242,#19243,#19244,#19245));
#4719=EDGE_LOOP('',(#19246,#19247,#19248,#19249));
#4720=EDGE_LOOP('',(#19250,#19251,#19252,#19253));
#4721=EDGE_LOOP('',(#19254,#19255,#19256,#19257));
#4722=EDGE_LOOP('',(#19258,#19259,#19260,#19261));
#4723=EDGE_LOOP('',(#19262,#19263,#19264,#19265));
#4724=EDGE_LOOP('',(#19266,#19267,#19268,#19269,#19270,#19271,#19272,#19273,
#19274,#19275,#19276,#19277,#19278,#19279,#19280,#19281,#19282,#19283,#19284,
#19285));
#4725=EDGE_LOOP('',(#19286,#19287,#19288,#19289,#19290));
#4726=EDGE_LOOP('',(#19291,#19292,#19293,#19294));
#4727=EDGE_LOOP('',(#19295,#19296,#19297,#19298,#19299,#19300,#19301,#19302,
#19303,#19304,#19305,#19306,#19307,#19308,#19309,#19310,#19311,#19312,#19313,
#19314));
#4728=EDGE_LOOP('',(#19315,#19316,#19317,#19318));
#4729=EDGE_LOOP('',(#19319,#19320,#19321));
#4730=EDGE_LOOP('',(#19322,#19323,#19324,#19325));
#4731=EDGE_LOOP('',(#19326,#19327,#19328,#19329));
#4732=EDGE_LOOP('',(#19330,#19331,#19332));
#4733=EDGE_LOOP('',(#19333,#19334,#19335));
#4734=EDGE_LOOP('',(#19336,#19337,#19338));
#4735=EDGE_LOOP('',(#19339,#19340,#19341));
#4736=EDGE_LOOP('',(#19342,#19343,#19344));
#4737=EDGE_LOOP('',(#19345,#19346,#19347));
#4738=EDGE_LOOP('',(#19348,#19349,#19350,#19351,#19352,#19353,#19354,#19355));
#4739=EDGE_LOOP('',(#19356,#19357,#19358,#19359,#19360,#19361,#19362,#19363));
#4740=EDGE_LOOP('',(#19364,#19365,#19366,#19367,#19368,#19369,#19370,#19371));
#4741=EDGE_LOOP('',(#19372,#19373,#19374,#19375,#19376,#19377,#19378,#19379,
#19380,#19381,#19382,#19383));
#4742=EDGE_LOOP('',(#19384,#19385,#19386,#19387));
#4743=EDGE_LOOP('',(#19388,#19389,#19390,#19391,#19392,#19393,#19394,#19395));
#4744=EDGE_LOOP('',(#19396,#19397,#19398));
#4745=EDGE_LOOP('',(#19399,#19400,#19401));
#4746=EDGE_LOOP('',(#19402,#19403,#19404));
#4747=EDGE_LOOP('',(#19405,#19406,#19407));
#4748=EDGE_LOOP('',(#19408,#19409,#19410));
#4749=EDGE_LOOP('',(#19411,#19412,#19413));
#4750=EDGE_LOOP('',(#19414,#19415,#19416,#19417,#19418,#19419,#19420,#19421));
#4751=EDGE_LOOP('',(#19422));
#4752=EDGE_LOOP('',(#19423,#19424,#19425,#19426));
#4753=EDGE_LOOP('',(#19427,#19428,#19429,#19430,#19431,#19432,#19433,#19434));
#4754=EDGE_LOOP('',(#19435,#19436,#19437,#19438,#19439,#19440,#19441,#19442,
#19443,#19444,#19445,#19446));
#4755=EDGE_LOOP('',(#19447));
#4756=EDGE_LOOP('',(#19448,#19449,#19450,#19451,#19452,#19453,#19454,#19455));
#4757=EDGE_LOOP('',(#19456,#19457,#19458,#19459));
#4758=EDGE_LOOP('',(#19460,#19461,#19462,#19463));
#4759=EDGE_LOOP('',(#19464,#19465,#19466,#19467));
#4760=EDGE_LOOP('',(#19468,#19469,#19470,#19471));
#4761=EDGE_LOOP('',(#19472,#19473,#19474,#19475));
#4762=EDGE_LOOP('',(#19476,#19477,#19478,#19479));
#4763=EDGE_LOOP('',(#19480,#19481,#19482,#19483));
#4764=EDGE_LOOP('',(#19484,#19485,#19486,#19487));
#4765=EDGE_LOOP('',(#19488,#19489,#19490,#19491));
#4766=EDGE_LOOP('',(#19492,#19493,#19494,#19495));
#4767=EDGE_LOOP('',(#19496,#19497,#19498,#19499));
#4768=EDGE_LOOP('',(#19500,#19501,#19502,#19503));
#4769=EDGE_LOOP('',(#19504,#19505,#19506,#19507));
#4770=EDGE_LOOP('',(#19508,#19509,#19510,#19511));
#4771=EDGE_LOOP('',(#19512,#19513,#19514,#19515));
#4772=EDGE_LOOP('',(#19516,#19517,#19518,#19519));
#4773=EDGE_LOOP('',(#19520,#19521,#19522,#19523));
#4774=EDGE_LOOP('',(#19524,#19525,#19526,#19527));
#4775=EDGE_LOOP('',(#19528,#19529,#19530,#19531));
#4776=EDGE_LOOP('',(#19532,#19533,#19534,#19535));
#4777=EDGE_LOOP('',(#19536,#19537,#19538,#19539));
#4778=EDGE_LOOP('',(#19540,#19541,#19542,#19543));
#4779=EDGE_LOOP('',(#19544,#19545,#19546,#19547));
#4780=EDGE_LOOP('',(#19548,#19549,#19550,#19551));
#4781=EDGE_LOOP('',(#19552,#19553,#19554,#19555));
#4782=EDGE_LOOP('',(#19556,#19557,#19558,#19559));
#4783=EDGE_LOOP('',(#19560,#19561,#19562,#19563));
#4784=EDGE_LOOP('',(#19564,#19565,#19566,#19567));
#4785=EDGE_LOOP('',(#19568,#19569,#19570,#19571));
#4786=EDGE_LOOP('',(#19572,#19573,#19574,#19575));
#4787=EDGE_LOOP('',(#19576,#19577,#19578,#19579));
#4788=EDGE_LOOP('',(#19580,#19581,#19582,#19583));
#4789=EDGE_LOOP('',(#19584,#19585,#19586,#19587));
#4790=EDGE_LOOP('',(#19588,#19589,#19590,#19591));
#4791=EDGE_LOOP('',(#19592,#19593,#19594,#19595));
#4792=EDGE_LOOP('',(#19596,#19597,#19598,#19599));
#4793=EDGE_LOOP('',(#19600,#19601,#19602,#19603));
#4794=EDGE_LOOP('',(#19604,#19605,#19606,#19607));
#4795=EDGE_LOOP('',(#19608,#19609,#19610,#19611));
#4796=EDGE_LOOP('',(#19612,#19613,#19614,#19615));
#4797=EDGE_LOOP('',(#19616,#19617,#19618,#19619));
#4798=EDGE_LOOP('',(#19620,#19621,#19622,#19623));
#4799=EDGE_LOOP('',(#19624,#19625,#19626,#19627));
#4800=EDGE_LOOP('',(#19628,#19629,#19630,#19631));
#4801=EDGE_LOOP('',(#19632,#19633,#19634,#19635));
#4802=EDGE_LOOP('',(#19636,#19637,#19638,#19639));
#4803=EDGE_LOOP('',(#19640,#19641,#19642,#19643));
#4804=EDGE_LOOP('',(#19644,#19645,#19646,#19647));
#4805=EDGE_LOOP('',(#19648,#19649,#19650,#19651));
#4806=EDGE_LOOP('',(#19652,#19653,#19654,#19655));
#4807=EDGE_LOOP('',(#19656,#19657,#19658,#19659));
#4808=EDGE_LOOP('',(#19660,#19661,#19662,#19663));
#4809=EDGE_LOOP('',(#19664,#19665,#19666,#19667));
#4810=EDGE_LOOP('',(#19668,#19669,#19670,#19671));
#4811=EDGE_LOOP('',(#19672,#19673,#19674,#19675));
#4812=EDGE_LOOP('',(#19676,#19677,#19678,#19679,#19680));
#4813=EDGE_LOOP('',(#19681,#19682,#19683,#19684,#19685));
#4814=EDGE_LOOP('',(#19686,#19687,#19688,#19689,#19690,#19691,#19692,#19693,
#19694,#19695,#19696,#19697,#19698,#19699,#19700,#19701,#19702,#19703,#19704,
#19705,#19706,#19707,#19708,#19709,#19710,#19711,#19712,#19713,#19714,#19715,
#19716,#19717,#19718,#19719,#19720,#19721,#19722,#19723,#19724,#19725,#19726,
#19727,#19728,#19729,#19730,#19731,#19732,#19733,#19734,#19735,#19736,#19737,
#19738,#19739,#19740,#19741,#19742,#19743,#19744,#19745,#19746));
#4815=EDGE_LOOP('',(#19747,#19748,#19749,#19750,#19751,#19752));
#4816=EDGE_LOOP('',(#19753,#19754,#19755));
#4817=EDGE_LOOP('',(#19756,#19757,#19758,#19759,#19760,#19761,#19762,#19763,
#19764,#19765,#19766,#19767,#19768,#19769,#19770,#19771,#19772,#19773,#19774,
#19775,#19776,#19777,#19778,#19779,#19780,#19781,#19782,#19783,#19784,#19785,
#19786,#19787,#19788,#19789,#19790,#19791,#19792,#19793,#19794,#19795,#19796,
#19797,#19798,#19799,#19800,#19801,#19802,#19803,#19804,#19805,#19806,#19807,
#19808,#19809,#19810,#19811,#19812,#19813,#19814,#19815));
#4818=EDGE_LOOP('',(#19816,#19817,#19818));
#4819=EDGE_LOOP('',(#19819,#19820,#19821,#19822));
#4820=EDGE_LOOP('',(#19823,#19824,#19825,#19826));
#4821=EDGE_LOOP('',(#19827,#19828,#19829));
#4822=EDGE_LOOP('',(#19830,#19831,#19832,#19833));
#4823=EDGE_LOOP('',(#19834,#19835,#19836,#19837));
#4824=EDGE_LOOP('',(#19838,#19839,#19840));
#4825=EDGE_LOOP('',(#19841,#19842,#19843,#19844));
#4826=EDGE_LOOP('',(#19845,#19846,#19847,#19848));
#4827=EDGE_LOOP('',(#19849,#19850,#19851));
#4828=EDGE_LOOP('',(#19852,#19853,#19854,#19855));
#4829=EDGE_LOOP('',(#19856,#19857,#19858,#19859));
#4830=EDGE_LOOP('',(#19860,#19861,#19862));
#4831=EDGE_LOOP('',(#19863,#19864,#19865,#19866));
#4832=EDGE_LOOP('',(#19867,#19868,#19869,#19870));
#4833=EDGE_LOOP('',(#19871,#19872,#19873));
#4834=EDGE_LOOP('',(#19874,#19875,#19876,#19877));
#4835=EDGE_LOOP('',(#19878,#19879,#19880,#19881));
#4836=EDGE_LOOP('',(#19882,#19883,#19884));
#4837=EDGE_LOOP('',(#19885,#19886,#19887,#19888));
#4838=EDGE_LOOP('',(#19889,#19890,#19891,#19892));
#4839=EDGE_LOOP('',(#19893,#19894,#19895));
#4840=EDGE_LOOP('',(#19896,#19897,#19898,#19899));
#4841=EDGE_LOOP('',(#19900,#19901,#19902,#19903));
#4842=EDGE_LOOP('',(#19904,#19905,#19906));
#4843=EDGE_LOOP('',(#19907,#19908,#19909,#19910));
#4844=EDGE_LOOP('',(#19911,#19912,#19913,#19914));
#4845=EDGE_LOOP('',(#19915,#19916,#19917));
#4846=EDGE_LOOP('',(#19918,#19919,#19920,#19921));
#4847=EDGE_LOOP('',(#19922,#19923,#19924,#19925));
#4848=EDGE_LOOP('',(#19926,#19927,#19928));
#4849=EDGE_LOOP('',(#19929,#19930,#19931,#19932));
#4850=EDGE_LOOP('',(#19933,#19934,#19935,#19936));
#4851=EDGE_LOOP('',(#19937,#19938,#19939));
#4852=EDGE_LOOP('',(#19940,#19941,#19942,#19943));
#4853=EDGE_LOOP('',(#19944,#19945,#19946,#19947));
#4854=EDGE_LOOP('',(#19948,#19949,#19950));
#4855=EDGE_LOOP('',(#19951,#19952,#19953,#19954));
#4856=EDGE_LOOP('',(#19955,#19956,#19957,#19958));
#4857=EDGE_LOOP('',(#19959,#19960,#19961));
#4858=EDGE_LOOP('',(#19962,#19963,#19964,#19965));
#4859=EDGE_LOOP('',(#19966,#19967,#19968,#19969));
#4860=EDGE_LOOP('',(#19970,#19971,#19972));
#4861=EDGE_LOOP('',(#19973,#19974,#19975,#19976));
#4862=EDGE_LOOP('',(#19977,#19978,#19979,#19980));
#4863=EDGE_LOOP('',(#19981,#19982,#19983));
#4864=EDGE_LOOP('',(#19984,#19985,#19986,#19987));
#4865=EDGE_LOOP('',(#19988,#19989,#19990,#19991));
#4866=EDGE_LOOP('',(#19992,#19993,#19994));
#4867=EDGE_LOOP('',(#19995,#19996,#19997,#19998));
#4868=EDGE_LOOP('',(#19999,#20000,#20001,#20002));
#4869=EDGE_LOOP('',(#20003,#20004,#20005,#20006));
#4870=EDGE_LOOP('',(#20007,#20008,#20009,#20010));
#4871=EDGE_LOOP('',(#20011,#20012,#20013,#20014));
#4872=EDGE_LOOP('',(#20015,#20016,#20017));
#4873=EDGE_LOOP('',(#20018,#20019,#20020,#20021));
#4874=EDGE_LOOP('',(#20022,#20023,#20024,#20025));
#4875=EDGE_LOOP('',(#20026,#20027,#20028));
#4876=EDGE_LOOP('',(#20029,#20030,#20031,#20032));
#4877=EDGE_LOOP('',(#20033,#20034,#20035,#20036));
#4878=EDGE_LOOP('',(#20037,#20038,#20039));
#4879=EDGE_LOOP('',(#20040,#20041,#20042,#20043));
#4880=EDGE_LOOP('',(#20044,#20045,#20046,#20047));
#4881=EDGE_LOOP('',(#20048,#20049,#20050));
#4882=EDGE_LOOP('',(#20051,#20052,#20053,#20054));
#4883=EDGE_LOOP('',(#20055,#20056,#20057,#20058));
#4884=EDGE_LOOP('',(#20059,#20060,#20061));
#4885=EDGE_LOOP('',(#20062,#20063,#20064,#20065));
#4886=EDGE_LOOP('',(#20066,#20067,#20068,#20069));
#4887=EDGE_LOOP('',(#20070,#20071,#20072));
#4888=EDGE_LOOP('',(#20073,#20074,#20075,#20076));
#4889=EDGE_LOOP('',(#20077,#20078,#20079,#20080));
#4890=EDGE_LOOP('',(#20081,#20082,#20083));
#4891=EDGE_LOOP('',(#20084,#20085,#20086,#20087));
#4892=EDGE_LOOP('',(#20088,#20089,#20090,#20091));
#4893=EDGE_LOOP('',(#20092,#20093,#20094));
#4894=EDGE_LOOP('',(#20095,#20096,#20097,#20098));
#4895=EDGE_LOOP('',(#20099,#20100,#20101,#20102));
#4896=EDGE_LOOP('',(#20103,#20104,#20105));
#4897=EDGE_LOOP('',(#20106,#20107,#20108,#20109));
#4898=EDGE_LOOP('',(#20110,#20111,#20112,#20113));
#4899=EDGE_LOOP('',(#20114,#20115,#20116));
#4900=EDGE_LOOP('',(#20117,#20118,#20119,#20120));
#4901=EDGE_LOOP('',(#20121,#20122,#20123,#20124));
#4902=EDGE_LOOP('',(#20125,#20126,#20127));
#4903=EDGE_LOOP('',(#20128,#20129,#20130,#20131));
#4904=EDGE_LOOP('',(#20132,#20133,#20134,#20135));
#4905=EDGE_LOOP('',(#20136,#20137,#20138));
#4906=EDGE_LOOP('',(#20139,#20140,#20141,#20142));
#4907=EDGE_LOOP('',(#20143,#20144,#20145,#20146));
#4908=EDGE_LOOP('',(#20147,#20148,#20149));
#4909=EDGE_LOOP('',(#20150,#20151,#20152,#20153));
#4910=EDGE_LOOP('',(#20154,#20155,#20156,#20157));
#4911=EDGE_LOOP('',(#20158,#20159,#20160));
#4912=EDGE_LOOP('',(#20161,#20162,#20163,#20164));
#4913=EDGE_LOOP('',(#20165,#20166,#20167,#20168));
#4914=EDGE_LOOP('',(#20169,#20170,#20171));
#4915=EDGE_LOOP('',(#20172,#20173,#20174,#20175));
#4916=EDGE_LOOP('',(#20176,#20177,#20178,#20179));
#4917=EDGE_LOOP('',(#20180,#20181,#20182));
#4918=EDGE_LOOP('',(#20183,#20184,#20185,#20186));
#4919=EDGE_LOOP('',(#20187,#20188,#20189,#20190));
#4920=EDGE_LOOP('',(#20191,#20192,#20193));
#4921=EDGE_LOOP('',(#20194,#20195,#20196,#20197));
#4922=EDGE_LOOP('',(#20198,#20199,#20200,#20201));
#4923=EDGE_LOOP('',(#20202,#20203,#20204,#20205,#20206,#20207,#20208,#20209,
#20210,#20211,#20212,#20213,#20214,#20215,#20216,#20217,#20218,#20219,#20220,
#20221,#20222,#20223,#20224,#20225,#20226,#20227,#20228,#20229,#20230,#20231,
#20232,#20233,#20234,#20235,#20236,#20237,#20238,#20239,#20240,#20241,#20242,
#20243,#20244,#20245,#20246,#20247,#20248,#20249,#20250,#20251,#20252,#20253,
#20254,#20255,#20256,#20257,#20258,#20259,#20260,#20261,#20262,#20263,#20264,
#20265,#20266,#20267,#20268,#20269,#20270,#20271,#20272,#20273,#20274,#20275,
#20276,#20277,#20278,#20279,#20280,#20281,#20282,#20283,#20284,#20285,#20286,
#20287,#20288,#20289,#20290,#20291,#20292,#20293,#20294,#20295,#20296,#20297,
#20298,#20299,#20300,#20301,#20302,#20303,#20304,#20305,#20306,#20307,#20308,
#20309,#20310,#20311,#20312,#20313,#20314,#20315,#20316,#20317,#20318,#20319,
#20320,#20321,#20322,#20323,#20324,#20325,#20326,#20327,#20328,#20329,#20330,
#20331,#20332,#20333,#20334,#20335,#20336,#20337,#20338,#20339,#20340,#20341,
#20342,#20343,#20344,#20345,#20346,#20347,#20348,#20349));
#4924=EDGE_LOOP('',(#20350,#20351,#20352,#20353));
#4925=EDGE_LOOP('',(#20354,#20355,#20356,#20357));
#4926=EDGE_LOOP('',(#20358,#20359,#20360));
#4927=EDGE_LOOP('',(#20361,#20362,#20363,#20364,#20365,#20366,#20367,#20368,
#20369,#20370,#20371,#20372,#20373,#20374,#20375,#20376,#20377,#20378,#20379,
#20380,#20381,#20382,#20383,#20384,#20385,#20386,#20387,#20388,#20389,#20390,
#20391,#20392,#20393,#20394,#20395,#20396,#20397,#20398,#20399,#20400,#20401,
#20402,#20403,#20404,#20405,#20406,#20407,#20408,#20409,#20410,#20411,#20412,
#20413,#20414,#20415,#20416,#20417,#20418,#20419,#20420,#20421,#20422,#20423,
#20424,#20425,#20426,#20427,#20428,#20429,#20430,#20431,#20432,#20433,#20434,
#20435,#20436,#20437,#20438,#20439,#20440,#20441,#20442,#20443,#20444,#20445,
#20446,#20447,#20448,#20449,#20450,#20451,#20452,#20453,#20454,#20455,#20456,
#20457,#20458,#20459,#20460,#20461,#20462,#20463,#20464,#20465,#20466,#20467,
#20468,#20469,#20470,#20471));
#4928=EDGE_LOOP('',(#20472,#20473,#20474));
#4929=EDGE_LOOP('',(#20475,#20476,#20477,#20478));
#4930=EDGE_LOOP('',(#20479,#20480,#20481,#20482));
#4931=EDGE_LOOP('',(#20483,#20484,#20485,#20486));
#4932=EDGE_LOOP('',(#20487,#20488,#20489,#20490));
#4933=EDGE_LOOP('',(#20491,#20492,#20493,#20494));
#4934=EDGE_LOOP('',(#20495,#20496,#20497,#20498));
#4935=EDGE_LOOP('',(#20499,#20500,#20501,#20502,#20503,#20504));
#4936=EDGE_LOOP('',(#20505));
#4937=EDGE_LOOP('',(#20506));
#4938=EDGE_LOOP('',(#20507,#20508,#20509,#20510));
#4939=EDGE_LOOP('',(#20511,#20512,#20513,#20514));
#4940=EDGE_LOOP('',(#20515,#20516,#20517,#20518,#20519,#20520));
#4941=EDGE_LOOP('',(#20521));
#4942=EDGE_LOOP('',(#20522));
#4943=EDGE_LOOP('',(#20523));
#4944=EDGE_LOOP('',(#20524,#20525,#20526,#20527,#20528,#20529));
#4945=EDGE_LOOP('',(#20530,#20531,#20532,#20533,#20534,#20535,#20536,#20537));
#4946=EDGE_LOOP('',(#20538,#20539,#20540,#20541));
#4947=EDGE_LOOP('',(#20542,#20543,#20544,#20545));
#4948=EDGE_LOOP('',(#20546,#20547,#20548,#20549));
#4949=EDGE_LOOP('',(#20550,#20551,#20552,#20553));
#4950=EDGE_LOOP('',(#20554,#20555,#20556,#20557));
#4951=EDGE_LOOP('',(#20558,#20559,#20560,#20561));
#4952=EDGE_LOOP('',(#20562,#20563,#20564,#20565));
#4953=EDGE_LOOP('',(#20566,#20567,#20568,#20569));
#4954=EDGE_LOOP('',(#20570,#20571,#20572,#20573));
#4955=EDGE_LOOP('',(#20574,#20575,#20576,#20577));
#4956=EDGE_LOOP('',(#20578,#20579,#20580,#20581));
#4957=EDGE_LOOP('',(#20582,#20583,#20584,#20585));
#4958=EDGE_LOOP('',(#20586,#20587,#20588,#20589));
#4959=EDGE_LOOP('',(#20590,#20591,#20592,#20593));
#4960=EDGE_LOOP('',(#20594,#20595,#20596,#20597));
#4961=EDGE_LOOP('',(#20598,#20599,#20600,#20601));
#4962=EDGE_LOOP('',(#20602,#20603,#20604,#20605));
#4963=EDGE_LOOP('',(#20606,#20607,#20608,#20609));
#4964=EDGE_LOOP('',(#20610,#20611,#20612,#20613));
#4965=EDGE_LOOP('',(#20614,#20615,#20616,#20617));
#4966=EDGE_LOOP('',(#20618,#20619,#20620,#20621));
#4967=EDGE_LOOP('',(#20622,#20623,#20624,#20625));
#4968=EDGE_LOOP('',(#20626,#20627,#20628,#20629));
#4969=EDGE_LOOP('',(#20630,#20631,#20632,#20633));
#4970=EDGE_LOOP('',(#20634,#20635,#20636,#20637));
#4971=EDGE_LOOP('',(#20638,#20639,#20640,#20641));
#4972=EDGE_LOOP('',(#20642,#20643,#20644,#20645));
#4973=EDGE_LOOP('',(#20646,#20647,#20648,#20649));
#4974=EDGE_LOOP('',(#20650,#20651,#20652,#20653));
#4975=EDGE_LOOP('',(#20654,#20655,#20656,#20657));
#4976=EDGE_LOOP('',(#20658,#20659,#20660,#20661));
#4977=EDGE_LOOP('',(#20662,#20663,#20664,#20665));
#4978=EDGE_LOOP('',(#20666,#20667,#20668,#20669));
#4979=EDGE_LOOP('',(#20670,#20671,#20672,#20673));
#4980=EDGE_LOOP('',(#20674,#20675,#20676,#20677));
#4981=EDGE_LOOP('',(#20678,#20679,#20680,#20681));
#4982=EDGE_LOOP('',(#20682,#20683,#20684,#20685));
#4983=EDGE_LOOP('',(#20686,#20687,#20688,#20689));
#4984=EDGE_LOOP('',(#20690,#20691,#20692,#20693));
#4985=EDGE_LOOP('',(#20694,#20695,#20696,#20697));
#4986=EDGE_LOOP('',(#20698,#20699,#20700,#20701));
#4987=EDGE_LOOP('',(#20702,#20703,#20704,#20705));
#4988=EDGE_LOOP('',(#20706,#20707,#20708,#20709));
#4989=EDGE_LOOP('',(#20710,#20711,#20712,#20713));
#4990=EDGE_LOOP('',(#20714,#20715,#20716,#20717));
#4991=EDGE_LOOP('',(#20718,#20719,#20720,#20721,#20722));
#4992=EDGE_LOOP('',(#20723,#20724,#20725,#20726,#20727));
#4993=EDGE_LOOP('',(#20728,#20729,#20730,#20731,#20732,#20733,#20734,#20735,
#20736,#20737,#20738,#20739,#20740,#20741,#20742,#20743,#20744,#20745,#20746,
#20747,#20748,#20749,#20750,#20751,#20752,#20753,#20754,#20755,#20756,#20757,
#20758,#20759,#20760,#20761,#20762,#20763,#20764,#20765,#20766,#20767,#20768,
#20769,#20770,#20771,#20772,#20773,#20774,#20775,#20776,#20777,#20778));
#4994=EDGE_LOOP('',(#20779,#20780,#20781,#20782,#20783,#20784));
#4995=EDGE_LOOP('',(#20785,#20786,#20787));
#4996=EDGE_LOOP('',(#20788,#20789,#20790,#20791,#20792,#20793,#20794,#20795,
#20796,#20797,#20798,#20799,#20800,#20801,#20802,#20803,#20804,#20805,#20806,
#20807,#20808,#20809,#20810,#20811,#20812,#20813,#20814,#20815,#20816,#20817,
#20818,#20819,#20820,#20821,#20822,#20823,#20824,#20825,#20826,#20827,#20828,
#20829,#20830,#20831,#20832,#20833,#20834,#20835,#20836,#20837));
#4997=EDGE_LOOP('',(#20838,#20839,#20840));
#4998=EDGE_LOOP('',(#20841,#20842,#20843,#20844));
#4999=EDGE_LOOP('',(#20845,#20846,#20847,#20848));
#5000=EDGE_LOOP('',(#20849,#20850,#20851));
#5001=EDGE_LOOP('',(#20852,#20853,#20854,#20855));
#5002=EDGE_LOOP('',(#20856,#20857,#20858,#20859));
#5003=EDGE_LOOP('',(#20860,#20861,#20862));
#5004=EDGE_LOOP('',(#20863,#20864,#20865,#20866));
#5005=EDGE_LOOP('',(#20867,#20868,#20869,#20870));
#5006=EDGE_LOOP('',(#20871,#20872,#20873));
#5007=EDGE_LOOP('',(#20874,#20875,#20876,#20877));
#5008=EDGE_LOOP('',(#20878,#20879,#20880,#20881));
#5009=EDGE_LOOP('',(#20882,#20883,#20884));
#5010=EDGE_LOOP('',(#20885,#20886,#20887,#20888));
#5011=EDGE_LOOP('',(#20889,#20890,#20891,#20892));
#5012=EDGE_LOOP('',(#20893,#20894,#20895));
#5013=EDGE_LOOP('',(#20896,#20897,#20898,#20899));
#5014=EDGE_LOOP('',(#20900,#20901,#20902,#20903));
#5015=EDGE_LOOP('',(#20904,#20905,#20906));
#5016=EDGE_LOOP('',(#20907,#20908,#20909,#20910));
#5017=EDGE_LOOP('',(#20911,#20912,#20913,#20914));
#5018=EDGE_LOOP('',(#20915,#20916,#20917));
#5019=EDGE_LOOP('',(#20918,#20919,#20920,#20921));
#5020=EDGE_LOOP('',(#20922,#20923,#20924,#20925));
#5021=EDGE_LOOP('',(#20926,#20927,#20928));
#5022=EDGE_LOOP('',(#20929,#20930,#20931,#20932));
#5023=EDGE_LOOP('',(#20933,#20934,#20935,#20936));
#5024=EDGE_LOOP('',(#20937,#20938,#20939));
#5025=EDGE_LOOP('',(#20940,#20941,#20942,#20943));
#5026=EDGE_LOOP('',(#20944,#20945,#20946,#20947));
#5027=EDGE_LOOP('',(#20948,#20949,#20950));
#5028=EDGE_LOOP('',(#20951,#20952,#20953,#20954));
#5029=EDGE_LOOP('',(#20955,#20956,#20957,#20958));
#5030=EDGE_LOOP('',(#20959,#20960,#20961));
#5031=EDGE_LOOP('',(#20962,#20963,#20964,#20965));
#5032=EDGE_LOOP('',(#20966,#20967,#20968,#20969));
#5033=EDGE_LOOP('',(#20970,#20971,#20972));
#5034=EDGE_LOOP('',(#20973,#20974,#20975,#20976));
#5035=EDGE_LOOP('',(#20977,#20978,#20979,#20980));
#5036=EDGE_LOOP('',(#20981,#20982,#20983));
#5037=EDGE_LOOP('',(#20984,#20985,#20986,#20987));
#5038=EDGE_LOOP('',(#20988,#20989,#20990,#20991));
#5039=EDGE_LOOP('',(#20992,#20993,#20994));
#5040=EDGE_LOOP('',(#20995,#20996,#20997,#20998));
#5041=EDGE_LOOP('',(#20999,#21000,#21001,#21002));
#5042=EDGE_LOOP('',(#21003,#21004,#21005));
#5043=EDGE_LOOP('',(#21006,#21007,#21008,#21009));
#5044=EDGE_LOOP('',(#21010,#21011,#21012,#21013));
#5045=EDGE_LOOP('',(#21014,#21015,#21016));
#5046=EDGE_LOOP('',(#21017,#21018,#21019,#21020));
#5047=EDGE_LOOP('',(#21021,#21022,#21023,#21024));
#5048=EDGE_LOOP('',(#21025,#21026,#21027,#21028));
#5049=EDGE_LOOP('',(#21029,#21030,#21031,#21032));
#5050=EDGE_LOOP('',(#21033,#21034,#21035,#21036));
#5051=EDGE_LOOP('',(#21037,#21038,#21039));
#5052=EDGE_LOOP('',(#21040,#21041,#21042,#21043));
#5053=EDGE_LOOP('',(#21044,#21045,#21046,#21047));
#5054=EDGE_LOOP('',(#21048,#21049,#21050));
#5055=EDGE_LOOP('',(#21051,#21052,#21053,#21054));
#5056=EDGE_LOOP('',(#21055,#21056,#21057,#21058));
#5057=EDGE_LOOP('',(#21059,#21060,#21061));
#5058=EDGE_LOOP('',(#21062,#21063,#21064,#21065));
#5059=EDGE_LOOP('',(#21066,#21067,#21068,#21069));
#5060=EDGE_LOOP('',(#21070,#21071,#21072));
#5061=EDGE_LOOP('',(#21073,#21074,#21075,#21076));
#5062=EDGE_LOOP('',(#21077,#21078,#21079,#21080));
#5063=EDGE_LOOP('',(#21081,#21082,#21083));
#5064=EDGE_LOOP('',(#21084,#21085,#21086,#21087));
#5065=EDGE_LOOP('',(#21088,#21089,#21090,#21091));
#5066=EDGE_LOOP('',(#21092,#21093,#21094));
#5067=EDGE_LOOP('',(#21095,#21096,#21097,#21098));
#5068=EDGE_LOOP('',(#21099,#21100,#21101,#21102));
#5069=EDGE_LOOP('',(#21103,#21104,#21105));
#5070=EDGE_LOOP('',(#21106,#21107,#21108,#21109));
#5071=EDGE_LOOP('',(#21110,#21111,#21112,#21113));
#5072=EDGE_LOOP('',(#21114,#21115,#21116));
#5073=EDGE_LOOP('',(#21117,#21118,#21119,#21120));
#5074=EDGE_LOOP('',(#21121,#21122,#21123,#21124));
#5075=EDGE_LOOP('',(#21125,#21126,#21127));
#5076=EDGE_LOOP('',(#21128,#21129,#21130,#21131));
#5077=EDGE_LOOP('',(#21132,#21133,#21134,#21135));
#5078=EDGE_LOOP('',(#21136,#21137,#21138));
#5079=EDGE_LOOP('',(#21139,#21140,#21141,#21142));
#5080=EDGE_LOOP('',(#21143,#21144,#21145,#21146));
#5081=EDGE_LOOP('',(#21147,#21148,#21149));
#5082=EDGE_LOOP('',(#21150,#21151,#21152,#21153));
#5083=EDGE_LOOP('',(#21154,#21155,#21156,#21157));
#5084=EDGE_LOOP('',(#21158,#21159,#21160));
#5085=EDGE_LOOP('',(#21161,#21162,#21163,#21164));
#5086=EDGE_LOOP('',(#21165,#21166,#21167,#21168));
#5087=EDGE_LOOP('',(#21169,#21170,#21171));
#5088=EDGE_LOOP('',(#21172,#21173,#21174,#21175));
#5089=EDGE_LOOP('',(#21176,#21177,#21178,#21179));
#5090=EDGE_LOOP('',(#21180,#21181,#21182));
#5091=EDGE_LOOP('',(#21183,#21184,#21185,#21186));
#5092=EDGE_LOOP('',(#21187,#21188,#21189,#21190));
#5093=EDGE_LOOP('',(#21191,#21192,#21193));
#5094=EDGE_LOOP('',(#21194,#21195,#21196,#21197));
#5095=EDGE_LOOP('',(#21198,#21199,#21200,#21201));
#5096=EDGE_LOOP('',(#21202,#21203,#21204));
#5097=EDGE_LOOP('',(#21205,#21206,#21207,#21208));
#5098=EDGE_LOOP('',(#21209,#21210,#21211,#21212));
#5099=EDGE_LOOP('',(#21213,#21214,#21215));
#5100=EDGE_LOOP('',(#21216,#21217,#21218,#21219));
#5101=EDGE_LOOP('',(#21220,#21221,#21222,#21223));
#5102=EDGE_LOOP('',(#21224,#21225,#21226,#21227,#21228,#21229,#21230,#21231,
#21232,#21233,#21234,#21235,#21236,#21237,#21238,#21239,#21240,#21241,#21242,
#21243,#21244,#21245,#21246,#21247,#21248,#21249,#21250,#21251,#21252,#21253,
#21254,#21255,#21256,#21257,#21258,#21259,#21260,#21261,#21262,#21263,#21264,
#21265,#21266,#21267,#21268,#21269,#21270,#21271,#21272,#21273,#21274,#21275,
#21276,#21277,#21278,#21279,#21280,#21281,#21282,#21283,#21284,#21285,#21286,
#21287,#21288,#21289,#21290,#21291,#21292,#21293,#21294,#21295,#21296,#21297,
#21298,#21299,#21300,#21301,#21302,#21303,#21304,#21305,#21306,#21307,#21308,
#21309,#21310,#21311,#21312,#21313,#21314,#21315,#21316,#21317,#21318,#21319,
#21320,#21321,#21322,#21323,#21324,#21325,#21326,#21327,#21328,#21329,#21330,
#21331,#21332,#21333,#21334,#21335,#21336,#21337,#21338,#21339,#21340,#21341,
#21342,#21343,#21344,#21345,#21346,#21347,#21348,#21349,#21350,#21351,#21352,
#21353,#21354,#21355,#21356,#21357,#21358,#21359,#21360,#21361,#21362,#21363,
#21364,#21365,#21366,#21367,#21368,#21369,#21370,#21371));
#5103=EDGE_LOOP('',(#21372,#21373,#21374,#21375));
#5104=EDGE_LOOP('',(#21376,#21377,#21378,#21379));
#5105=EDGE_LOOP('',(#21380,#21381,#21382));
#5106=EDGE_LOOP('',(#21383,#21384,#21385,#21386,#21387,#21388,#21389,#21390,
#21391,#21392,#21393,#21394,#21395,#21396,#21397,#21398,#21399,#21400,#21401,
#21402,#21403,#21404,#21405,#21406,#21407,#21408,#21409,#21410,#21411,#21412,
#21413,#21414,#21415,#21416,#21417,#21418,#21419,#21420,#21421,#21422,#21423,
#21424,#21425,#21426,#21427,#21428,#21429,#21430,#21431,#21432,#21433,#21434,
#21435,#21436,#21437,#21438,#21439,#21440,#21441,#21442,#21443,#21444,#21445,
#21446,#21447,#21448,#21449,#21450,#21451,#21452,#21453,#21454,#21455,#21456,
#21457,#21458,#21459,#21460,#21461,#21462,#21463,#21464,#21465,#21466,#21467,
#21468,#21469,#21470,#21471,#21472,#21473,#21474,#21475,#21476,#21477,#21478,
#21479,#21480,#21481,#21482,#21483,#21484,#21485,#21486,#21487,#21488,#21489,
#21490,#21491,#21492,#21493));
#5107=EDGE_LOOP('',(#21494,#21495,#21496));
#5108=EDGE_LOOP('',(#21497,#21498,#21499,#21500));
#5109=EDGE_LOOP('',(#21501,#21502,#21503,#21504));
#5110=EDGE_LOOP('',(#21505,#21506,#21507,#21508));
#5111=EDGE_LOOP('',(#21509,#21510,#21511,#21512));
#5112=EDGE_LOOP('',(#21513,#21514,#21515,#21516));
#5113=EDGE_LOOP('',(#21517,#21518,#21519,#21520));
#5114=EDGE_LOOP('',(#21521,#21522,#21523,#21524,#21525,#21526));
#5115=EDGE_LOOP('',(#21527));
#5116=EDGE_LOOP('',(#21528));
#5117=EDGE_LOOP('',(#21529,#21530,#21531,#21532));
#5118=EDGE_LOOP('',(#21533,#21534,#21535,#21536));
#5119=EDGE_LOOP('',(#21537,#21538,#21539,#21540,#21541,#21542));
#5120=EDGE_LOOP('',(#21543));
#5121=EDGE_LOOP('',(#21544));
#5122=EDGE_LOOP('',(#21545));
#5123=EDGE_LOOP('',(#21546,#21547,#21548,#21549,#21550,#21551));
#5124=EDGE_LOOP('',(#21552,#21553,#21554,#21555,#21556,#21557,#21558,#21559));
#5125=EDGE_LOOP('',(#21560,#21561,#21562,#21563));
#5126=EDGE_LOOP('',(#21564,#21565,#21566,#21567));
#5127=EDGE_LOOP('',(#21568,#21569,#21570,#21571));
#5128=EDGE_LOOP('',(#21572,#21573,#21574,#21575));
#5129=EDGE_LOOP('',(#21576,#21577,#21578,#21579));
#5130=EDGE_LOOP('',(#21580,#21581,#21582,#21583));
#5131=EDGE_LOOP('',(#21584,#21585,#21586,#21587));
#5132=EDGE_LOOP('',(#21588,#21589,#21590,#21591));
#5133=EDGE_LOOP('',(#21592,#21593,#21594,#21595));
#5134=EDGE_LOOP('',(#21596,#21597,#21598,#21599));
#5135=EDGE_LOOP('',(#21600,#21601,#21602,#21603));
#5136=EDGE_LOOP('',(#21604,#21605,#21606,#21607));
#5137=EDGE_LOOP('',(#21608,#21609,#21610,#21611));
#5138=EDGE_LOOP('',(#21612,#21613,#21614,#21615));
#5139=EDGE_LOOP('',(#21616,#21617,#21618,#21619));
#5140=EDGE_LOOP('',(#21620,#21621,#21622,#21623));
#5141=EDGE_LOOP('',(#21624,#21625,#21626,#21627));
#5142=EDGE_LOOP('',(#21628,#21629,#21630,#21631));
#5143=EDGE_LOOP('',(#21632,#21633,#21634,#21635));
#5144=EDGE_LOOP('',(#21636,#21637,#21638,#21639));
#5145=EDGE_LOOP('',(#21640,#21641,#21642,#21643));
#5146=EDGE_LOOP('',(#21644,#21645,#21646,#21647));
#5147=EDGE_LOOP('',(#21648,#21649,#21650,#21651,#21652));
#5148=EDGE_LOOP('',(#21653,#21654,#21655,#21656,#21657));
#5149=EDGE_LOOP('',(#21658,#21659,#21660,#21661,#21662,#21663,#21664,#21665,
#21666,#21667,#21668,#21669,#21670,#21671,#21672,#21673,#21674,#21675,#21676,
#21677,#21678,#21679,#21680,#21681,#21682,#21683,#21684,#21685));
#5150=EDGE_LOOP('',(#21686,#21687,#21688,#21689,#21690,#21691));
#5151=EDGE_LOOP('',(#21692,#21693,#21694));
#5152=EDGE_LOOP('',(#21695,#21696,#21697,#21698,#21699,#21700,#21701,#21702,
#21703,#21704,#21705,#21706,#21707,#21708,#21709,#21710,#21711,#21712,#21713,
#21714,#21715,#21716,#21717,#21718,#21719,#21720,#21721));
#5153=EDGE_LOOP('',(#21722,#21723,#21724,#21725));
#5154=EDGE_LOOP('',(#21726,#21727,#21728));
#5155=EDGE_LOOP('',(#21729,#21730,#21731,#21732));
#5156=EDGE_LOOP('',(#21733,#21734,#21735,#21736));
#5157=EDGE_LOOP('',(#21737,#21738,#21739));
#5158=EDGE_LOOP('',(#21740,#21741,#21742,#21743));
#5159=EDGE_LOOP('',(#21744,#21745,#21746,#21747));
#5160=EDGE_LOOP('',(#21748,#21749,#21750));
#5161=EDGE_LOOP('',(#21751,#21752,#21753,#21754));
#5162=EDGE_LOOP('',(#21755,#21756,#21757,#21758));
#5163=EDGE_LOOP('',(#21759,#21760,#21761));
#5164=EDGE_LOOP('',(#21762,#21763,#21764,#21765));
#5165=EDGE_LOOP('',(#21766,#21767,#21768,#21769));
#5166=EDGE_LOOP('',(#21770,#21771,#21772));
#5167=EDGE_LOOP('',(#21773,#21774,#21775,#21776));
#5168=EDGE_LOOP('',(#21777,#21778,#21779,#21780));
#5169=EDGE_LOOP('',(#21781,#21782,#21783));
#5170=EDGE_LOOP('',(#21784,#21785,#21786,#21787));
#5171=EDGE_LOOP('',(#21788,#21789,#21790,#21791));
#5172=EDGE_LOOP('',(#21792,#21793,#21794));
#5173=EDGE_LOOP('',(#21795,#21796,#21797,#21798));
#5174=EDGE_LOOP('',(#21799,#21800,#21801,#21802));
#5175=EDGE_LOOP('',(#21803,#21804,#21805));
#5176=EDGE_LOOP('',(#21806,#21807,#21808,#21809));
#5177=EDGE_LOOP('',(#21810,#21811,#21812,#21813));
#5178=EDGE_LOOP('',(#21814,#21815,#21816));
#5179=EDGE_LOOP('',(#21817,#21818,#21819,#21820));
#5180=EDGE_LOOP('',(#21821,#21822,#21823,#21824));
#5181=EDGE_LOOP('',(#21825,#21826,#21827));
#5182=EDGE_LOOP('',(#21828,#21829,#21830,#21831));
#5183=EDGE_LOOP('',(#21832,#21833,#21834,#21835));
#5184=EDGE_LOOP('',(#21836,#21837,#21838));
#5185=EDGE_LOOP('',(#21839,#21840,#21841,#21842));
#5186=EDGE_LOOP('',(#21843,#21844,#21845,#21846));
#5187=EDGE_LOOP('',(#21847,#21848,#21849));
#5188=EDGE_LOOP('',(#21850,#21851,#21852,#21853));
#5189=EDGE_LOOP('',(#21854,#21855,#21856,#21857));
#5190=EDGE_LOOP('',(#21858,#21859,#21860));
#5191=EDGE_LOOP('',(#21861,#21862,#21863,#21864));
#5192=EDGE_LOOP('',(#21865,#21866,#21867,#21868));
#5193=EDGE_LOOP('',(#21869,#21870,#21871));
#5194=EDGE_LOOP('',(#21872,#21873,#21874,#21875));
#5195=EDGE_LOOP('',(#21876,#21877,#21878,#21879));
#5196=EDGE_LOOP('',(#21880,#21881,#21882));
#5197=EDGE_LOOP('',(#21883,#21884,#21885,#21886));
#5198=EDGE_LOOP('',(#21887,#21888,#21889,#21890));
#5199=EDGE_LOOP('',(#21891,#21892,#21893));
#5200=EDGE_LOOP('',(#21894,#21895,#21896,#21897));
#5201=EDGE_LOOP('',(#21898,#21899,#21900,#21901));
#5202=EDGE_LOOP('',(#21902,#21903,#21904));
#5203=EDGE_LOOP('',(#21905,#21906,#21907,#21908));
#5204=EDGE_LOOP('',(#21909,#21910,#21911,#21912));
#5205=EDGE_LOOP('',(#21913,#21914,#21915,#21916));
#5206=EDGE_LOOP('',(#21917,#21918,#21919,#21920));
#5207=EDGE_LOOP('',(#21921,#21922,#21923,#21924));
#5208=EDGE_LOOP('',(#21925,#21926,#21927));
#5209=EDGE_LOOP('',(#21928,#21929,#21930,#21931));
#5210=EDGE_LOOP('',(#21932,#21933,#21934,#21935));
#5211=EDGE_LOOP('',(#21936,#21937,#21938));
#5212=EDGE_LOOP('',(#21939,#21940,#21941,#21942));
#5213=EDGE_LOOP('',(#21943,#21944,#21945,#21946));
#5214=EDGE_LOOP('',(#21947,#21948,#21949));
#5215=EDGE_LOOP('',(#21950,#21951,#21952,#21953));
#5216=EDGE_LOOP('',(#21954,#21955,#21956,#21957));
#5217=EDGE_LOOP('',(#21958,#21959,#21960));
#5218=EDGE_LOOP('',(#21961,#21962,#21963,#21964));
#5219=EDGE_LOOP('',(#21965,#21966,#21967,#21968));
#5220=EDGE_LOOP('',(#21969,#21970,#21971));
#5221=EDGE_LOOP('',(#21972,#21973,#21974,#21975));
#5222=EDGE_LOOP('',(#21976,#21977,#21978,#21979));
#5223=EDGE_LOOP('',(#21980,#21981,#21982));
#5224=EDGE_LOOP('',(#21983,#21984,#21985,#21986));
#5225=EDGE_LOOP('',(#21987,#21988,#21989,#21990));
#5226=EDGE_LOOP('',(#21991,#21992,#21993));
#5227=EDGE_LOOP('',(#21994,#21995,#21996,#21997));
#5228=EDGE_LOOP('',(#21998,#21999,#22000,#22001));
#5229=EDGE_LOOP('',(#22002,#22003,#22004));
#5230=EDGE_LOOP('',(#22005,#22006,#22007,#22008));
#5231=EDGE_LOOP('',(#22009,#22010,#22011,#22012));
#5232=EDGE_LOOP('',(#22013,#22014,#22015));
#5233=EDGE_LOOP('',(#22016,#22017,#22018,#22019));
#5234=EDGE_LOOP('',(#22020,#22021,#22022,#22023));
#5235=EDGE_LOOP('',(#22024,#22025,#22026));
#5236=EDGE_LOOP('',(#22027,#22028,#22029,#22030));
#5237=EDGE_LOOP('',(#22031,#22032,#22033,#22034));
#5238=EDGE_LOOP('',(#22035,#22036,#22037));
#5239=EDGE_LOOP('',(#22038,#22039,#22040,#22041));
#5240=EDGE_LOOP('',(#22042,#22043,#22044,#22045));
#5241=EDGE_LOOP('',(#22046,#22047,#22048));
#5242=EDGE_LOOP('',(#22049,#22050,#22051,#22052));
#5243=EDGE_LOOP('',(#22053,#22054,#22055,#22056));
#5244=EDGE_LOOP('',(#22057,#22058,#22059));
#5245=EDGE_LOOP('',(#22060,#22061,#22062,#22063));
#5246=EDGE_LOOP('',(#22064,#22065,#22066,#22067));
#5247=EDGE_LOOP('',(#22068,#22069,#22070));
#5248=EDGE_LOOP('',(#22071,#22072,#22073,#22074));
#5249=EDGE_LOOP('',(#22075,#22076,#22077,#22078));
#5250=EDGE_LOOP('',(#22079,#22080,#22081));
#5251=EDGE_LOOP('',(#22082,#22083,#22084,#22085));
#5252=EDGE_LOOP('',(#22086,#22087,#22088,#22089));
#5253=EDGE_LOOP('',(#22090,#22091,#22092));
#5254=EDGE_LOOP('',(#22093,#22094,#22095,#22096));
#5255=EDGE_LOOP('',(#22097,#22098,#22099,#22100));
#5256=EDGE_LOOP('',(#22101,#22102,#22103));
#5257=EDGE_LOOP('',(#22104,#22105,#22106,#22107));
#5258=EDGE_LOOP('',(#22108,#22109,#22110,#22111));
#5259=EDGE_LOOP('',(#22112,#22113,#22114,#22115,#22116,#22117,#22118,#22119,
#22120,#22121,#22122,#22123,#22124,#22125,#22126,#22127,#22128,#22129,#22130,
#22131,#22132,#22133,#22134,#22135,#22136,#22137,#22138,#22139,#22140,#22141,
#22142,#22143,#22144,#22145,#22146,#22147,#22148,#22149,#22150,#22151,#22152,
#22153,#22154,#22155,#22156,#22157,#22158,#22159,#22160,#22161,#22162,#22163,
#22164,#22165,#22166,#22167,#22168,#22169,#22170,#22171,#22172,#22173,#22174,
#22175,#22176,#22177,#22178,#22179,#22180,#22181,#22182,#22183,#22184,#22185,
#22186,#22187,#22188,#22189,#22190,#22191,#22192,#22193,#22194,#22195,#22196,
#22197,#22198,#22199,#22200,#22201,#22202,#22203,#22204,#22205,#22206,#22207,
#22208,#22209,#22210,#22211,#22212,#22213,#22214,#22215,#22216,#22217,#22218,
#22219,#22220,#22221,#22222,#22223,#22224,#22225,#22226,#22227,#22228,#22229,
#22230,#22231,#22232,#22233,#22234,#22235,#22236,#22237,#22238,#22239,#22240,
#22241,#22242,#22243,#22244,#22245,#22246,#22247,#22248,#22249,#22250,#22251,
#22252,#22253,#22254,#22255,#22256,#22257,#22258,#22259));
#5260=EDGE_LOOP('',(#22260,#22261,#22262,#22263));
#5261=EDGE_LOOP('',(#22264,#22265,#22266,#22267));
#5262=EDGE_LOOP('',(#22268,#22269,#22270));
#5263=EDGE_LOOP('',(#22271,#22272,#22273,#22274,#22275,#22276,#22277,#22278,
#22279,#22280,#22281,#22282,#22283,#22284,#22285,#22286,#22287,#22288,#22289,
#22290,#22291,#22292,#22293,#22294,#22295,#22296,#22297,#22298,#22299,#22300,
#22301,#22302,#22303,#22304,#22305,#22306,#22307,#22308,#22309,#22310,#22311,
#22312,#22313,#22314,#22315,#22316,#22317,#22318,#22319,#22320,#22321,#22322,
#22323,#22324,#22325,#22326,#22327,#22328,#22329,#22330,#22331,#22332,#22333,
#22334,#22335,#22336,#22337,#22338,#22339,#22340,#22341,#22342,#22343,#22344,
#22345,#22346,#22347,#22348,#22349,#22350,#22351,#22352,#22353,#22354,#22355,
#22356,#22357,#22358,#22359,#22360,#22361,#22362,#22363,#22364,#22365,#22366,
#22367,#22368,#22369,#22370,#22371,#22372,#22373,#22374,#22375,#22376,#22377,
#22378,#22379,#22380,#22381));
#5264=EDGE_LOOP('',(#22382,#22383,#22384));
#5265=EDGE_LOOP('',(#22385,#22386,#22387,#22388));
#5266=EDGE_LOOP('',(#22389,#22390,#22391,#22392));
#5267=EDGE_LOOP('',(#22393,#22394,#22395,#22396));
#5268=EDGE_LOOP('',(#22397,#22398,#22399,#22400));
#5269=EDGE_LOOP('',(#22401,#22402,#22403,#22404));
#5270=EDGE_LOOP('',(#22405,#22406,#22407,#22408));
#5271=EDGE_LOOP('',(#22409,#22410,#22411,#22412,#22413,#22414));
#5272=EDGE_LOOP('',(#22415));
#5273=EDGE_LOOP('',(#22416));
#5274=EDGE_LOOP('',(#22417,#22418,#22419,#22420));
#5275=EDGE_LOOP('',(#22421,#22422,#22423,#22424,#22425,#22426));
#5276=EDGE_LOOP('',(#22427));
#5277=EDGE_LOOP('',(#22428));
#5278=EDGE_LOOP('',(#22429));
#5279=EDGE_LOOP('',(#22430,#22431,#22432,#22433,#22434,#22435));
#5280=EDGE_LOOP('',(#22436,#22437,#22438,#22439,#22440,#22441,#22442,#22443));
#5281=EDGE_LOOP('',(#22444,#22445,#22446,#22447));
#5282=EDGE_LOOP('',(#22448,#22449,#22450,#22451));
#5283=EDGE_LOOP('',(#22452,#22453,#22454,#22455));
#5284=EDGE_LOOP('',(#22456,#22457,#22458,#22459));
#5285=EDGE_LOOP('',(#22460,#22461,#22462,#22463));
#5286=EDGE_LOOP('',(#22464,#22465,#22466,#22467));
#5287=EDGE_LOOP('',(#22468,#22469,#22470,#22471));
#5288=EDGE_LOOP('',(#22472,#22473,#22474,#22475));
#5289=EDGE_LOOP('',(#22476,#22477,#22478,#22479));
#5290=EDGE_LOOP('',(#22480,#22481,#22482,#22483));
#5291=EDGE_LOOP('',(#22484,#22485,#22486,#22487));
#5292=EDGE_LOOP('',(#22488,#22489,#22490,#22491));
#5293=EDGE_LOOP('',(#22492,#22493,#22494,#22495));
#5294=EDGE_LOOP('',(#22496,#22497,#22498,#22499,#22500));
#5295=EDGE_LOOP('',(#22501,#22502,#22503,#22504,#22505,#22506,#22507,#22508,
#22509,#22510,#22511,#22512,#22513,#22514,#22515,#22516,#22517,#22518,#22519));
#5296=EDGE_LOOP('',(#22520,#22521,#22522,#22523,#22524,#22525));
#5297=EDGE_LOOP('',(#22526,#22527,#22528));
#5298=EDGE_LOOP('',(#22529,#22530,#22531,#22532,#22533,#22534,#22535,#22536,
#22537,#22538,#22539,#22540,#22541,#22542,#22543,#22544,#22545,#22546));
#5299=EDGE_LOOP('',(#22547,#22548,#22549,#22550));
#5300=EDGE_LOOP('',(#22551,#22552,#22553,#22554));
#5301=EDGE_LOOP('',(#22555,#22556,#22557,#22558));
#5302=EDGE_LOOP('',(#22559,#22560,#22561,#22562));
#5303=EDGE_LOOP('',(#22563,#22564,#22565,#22566));
#5304=EDGE_LOOP('',(#22567,#22568,#22569,#22570));
#5305=EDGE_LOOP('',(#22571));
#5306=EDGE_LOOP('',(#22572,#22573,#22574,#22575,#22576,#22577,#22578,#22579,
#22580,#22581,#22582,#22583));
#5307=EDGE_LOOP('',(#22584,#22585,#22586,#22587));
#5308=EDGE_LOOP('',(#22588,#22589,#22590,#22591));
#5309=EDGE_LOOP('',(#22592,#22593,#22594,#22595));
#5310=EDGE_LOOP('',(#22596,#22597,#22598,#22599));
#5311=EDGE_LOOP('',(#22600,#22601,#22602,#22603));
#5312=EDGE_LOOP('',(#22604,#22605,#22606,#22607));
#5313=EDGE_LOOP('',(#22608,#22609,#22610,#22611,#22612,#22613,#22614,#22615,
#22616,#22617,#22618,#22619));
#5314=EDGE_LOOP('',(#22620));
#5315=EDGE_LOOP('',(#22621,#22622,#22623,#22624));
#5316=EDGE_LOOP('',(#22625,#22626,#22627,#22628));
#5317=EDGE_LOOP('',(#22629));
#5318=EDGE_LOOP('',(#22630,#22631,#22632,#22633));
#5319=EDGE_LOOP('',(#22634,#22635,#22636,#22637));
#5320=EDGE_LOOP('',(#22638,#22639,#22640,#22641));
#5321=EDGE_LOOP('',(#22642,#22643,#22644,#22645,#22646,#22647,#22648,#22649));
#5322=EDGE_LOOP('',(#22650,#22651,#22652,#22653));
#5323=EDGE_LOOP('',(#22654,#22655,#22656,#22657));
#5324=EDGE_LOOP('',(#22658,#22659,#22660,#22661));
#5325=EDGE_LOOP('',(#22662,#22663,#22664,#22665));
#5326=EDGE_LOOP('',(#22666,#22667,#22668,#22669));
#5327=EDGE_LOOP('',(#22670,#22671,#22672,#22673));
#5328=EDGE_LOOP('',(#22674,#22675,#22676,#22677));
#5329=EDGE_LOOP('',(#22678,#22679,#22680,#22681));
#5330=EDGE_LOOP('',(#22682,#22683,#22684,#22685));
#5331=EDGE_LOOP('',(#22686,#22687,#22688,#22689));
#5332=EDGE_LOOP('',(#22690,#22691,#22692,#22693));
#5333=EDGE_LOOP('',(#22694,#22695,#22696,#22697));
#5334=EDGE_LOOP('',(#22698,#22699,#22700,#22701));
#5335=EDGE_LOOP('',(#22702,#22703,#22704,#22705));
#5336=EDGE_LOOP('',(#22706,#22707,#22708,#22709));
#5337=EDGE_LOOP('',(#22710,#22711,#22712));
#5338=EDGE_LOOP('',(#22713,#22714,#22715,#22716,#22717));
#5339=EDGE_LOOP('',(#22718,#22719,#22720,#22721));
#5340=EDGE_LOOP('',(#22722,#22723,#22724,#22725));
#5341=EDGE_LOOP('',(#22726,#22727,#22728,#22729));
#5342=EDGE_LOOP('',(#22730,#22731,#22732,#22733));
#5343=EDGE_LOOP('',(#22734,#22735,#22736,#22737));
#5344=EDGE_LOOP('',(#22738,#22739,#22740,#22741));
#5345=EDGE_LOOP('',(#22742,#22743,#22744,#22745));
#5346=EDGE_LOOP('',(#22746,#22747,#22748,#22749));
#5347=EDGE_LOOP('',(#22750,#22751,#22752,#22753));
#5348=EDGE_LOOP('',(#22754,#22755,#22756,#22757));
#5349=EDGE_LOOP('',(#22758,#22759,#22760,#22761));
#5350=EDGE_LOOP('',(#22762,#22763,#22764,#22765));
#5351=EDGE_LOOP('',(#22766,#22767,#22768,#22769));
#5352=EDGE_LOOP('',(#22770,#22771,#22772,#22773));
#5353=EDGE_LOOP('',(#22774,#22775,#22776,#22777,#22778));
#5354=EDGE_LOOP('',(#22779,#22780,#22781,#22782,#22783,#22784,#22785,#22786,
#22787,#22788,#22789,#22790,#22791,#22792,#22793,#22794,#22795,#22796,#22797,
#22798,#22799,#22800,#22801,#22802,#22803,#22804,#22805,#22806,#22807,#22808,
#22809,#22810,#22811,#22812,#22813,#22814));
#5355=EDGE_LOOP('',(#22815,#22816,#22817,#22818,#22819,#22820));
#5356=EDGE_LOOP('',(#22821,#22822,#22823));
#5357=EDGE_LOOP('',(#22824,#22825,#22826,#22827,#22828,#22829,#22830,#22831,
#22832,#22833,#22834,#22835,#22836,#22837,#22838,#22839,#22840,#22841,#22842,
#22843,#22844,#22845,#22846,#22847,#22848,#22849,#22850,#22851,#22852,#22853,
#22854,#22855,#22856,#22857,#22858,#22859));
#5358=EDGE_LOOP('',(#22860,#22861,#22862,#22863));
#5359=EDGE_LOOP('',(#22864,#22865,#22866,#22867));
#5360=EDGE_LOOP('',(#22868,#22869,#22870,#22871));
#5361=EDGE_LOOP('',(#22872,#22873,#22874,#22875));
#5362=EDGE_LOOP('',(#22876,#22877,#22878,#22879));
#5363=EDGE_LOOP('',(#22880,#22881,#22882,#22883));
#5364=EDGE_LOOP('',(#22884,#22885,#22886,#22887));
#5365=EDGE_LOOP('',(#22888));
#5366=EDGE_LOOP('',(#22889,#22890,#22891,#22892,#22893,#22894,#22895,#22896,
#22897,#22898,#22899,#22900));
#5367=EDGE_LOOP('',(#22901,#22902,#22903,#22904));
#5368=EDGE_LOOP('',(#22905,#22906,#22907,#22908));
#5369=EDGE_LOOP('',(#22909,#22910,#22911,#22912));
#5370=EDGE_LOOP('',(#22913,#22914,#22915,#22916));
#5371=EDGE_LOOP('',(#22917,#22918,#22919,#22920));
#5372=EDGE_LOOP('',(#22921,#22922,#22923,#22924));
#5373=EDGE_LOOP('',(#22925,#22926,#22927,#22928,#22929,#22930,#22931,#22932,
#22933,#22934,#22935,#22936));
#5374=EDGE_LOOP('',(#22937));
#5375=EDGE_LOOP('',(#22938,#22939,#22940,#22941));
#5376=EDGE_LOOP('',(#22942));
#5377=EDGE_LOOP('',(#22943,#22944,#22945,#22946,#22947));
#5378=EDGE_LOOP('',(#22948,#22949,#22950,#22951));
#5379=EDGE_LOOP('',(#22952,#22953,#22954,#22955));
#5380=LINE('',#33875,#7201);
#5381=LINE('',#33881,#7202);
#5382=LINE('',#33886,#7203);
#5383=LINE('',#33891,#7204);
#5384=LINE('',#33895,#7205);
#5385=LINE('',#33914,#7206);
#5386=LINE('',#33934,#7207);
#5387=LINE('',#33937,#7208);
#5388=LINE('',#33941,#7209);
#5389=LINE('',#33950,#7210);
#5390=LINE('',#33954,#7211);
#5391=LINE('',#33957,#7212);
#5392=LINE('',#33961,#7213);
#5393=LINE('',#33974,#7214);
#5394=LINE('',#33981,#7215);
#5395=LINE('',#33984,#7216);
#5396=LINE('',#33991,#7217);
#5397=LINE('',#33994,#7218);
#5398=LINE('',#34001,#7219);
#5399=LINE('',#34004,#7220);
#5400=LINE('',#34011,#7221);
#5401=LINE('',#34014,#7222);
#5402=LINE('',#34021,#7223);
#5403=LINE('',#34024,#7224);
#5404=LINE('',#34031,#7225);
#5405=LINE('',#34034,#7226);
#5406=LINE('',#34040,#7227);
#5407=LINE('',#34044,#7228);
#5408=LINE('',#34051,#7229);
#5409=LINE('',#34057,#7230);
#5410=LINE('',#34061,#7231);
#5411=LINE('',#34065,#7232);
#5412=LINE('',#34068,#7233);
#5413=LINE('',#34072,#7234);
#5414=LINE('',#34076,#7235);
#5415=LINE('',#34079,#7236);
#5416=LINE('',#34083,#7237);
#5417=LINE('',#34087,#7238);
#5418=LINE('',#34090,#7239);
#5419=LINE('',#34093,#7240);
#5420=LINE('',#34097,#7241);
#5421=LINE('',#34101,#7242);
#5422=LINE('',#34106,#7243);
#5423=LINE('',#34110,#7244);
#5424=LINE('',#34114,#7245);
#5425=LINE('',#34119,#7246);
#5426=LINE('',#34123,#7247);
#5427=LINE('',#34127,#7248);
#5428=LINE('',#34132,#7249);
#5429=LINE('',#34136,#7250);
#5430=LINE('',#34140,#7251);
#5431=LINE('',#34145,#7252);
#5432=LINE('',#34149,#7253);
#5433=LINE('',#34153,#7254);
#5434=LINE('',#34158,#7255);
#5435=LINE('',#34162,#7256);
#5436=LINE('',#34166,#7257);
#5437=LINE('',#34171,#7258);
#5438=LINE('',#34176,#7259);
#5439=LINE('',#34181,#7260);
#5440=LINE('',#34185,#7261);
#5441=LINE('',#34189,#7262);
#5442=LINE('',#34194,#7263);
#5443=LINE('',#34198,#7264);
#5444=LINE('',#34202,#7265);
#5445=LINE('',#34207,#7266);
#5446=LINE('',#34211,#7267);
#5447=LINE('',#34215,#7268);
#5448=LINE('',#34220,#7269);
#5449=LINE('',#34224,#7270);
#5450=LINE('',#34228,#7271);
#5451=LINE('',#34233,#7272);
#5452=LINE('',#34237,#7273);
#5453=LINE('',#34241,#7274);
#5454=LINE('',#34246,#7275);
#5455=LINE('',#34250,#7276);
#5456=LINE('',#34254,#7277);
#5457=LINE('',#34259,#7278);
#5458=LINE('',#34263,#7279);
#5459=LINE('',#34267,#7280);
#5460=LINE('',#34272,#7281);
#5461=LINE('',#34276,#7282);
#5462=LINE('',#34280,#7283);
#5463=LINE('',#34285,#7284);
#5464=LINE('',#34289,#7285);
#5465=LINE('',#34293,#7286);
#5466=LINE('',#34298,#7287);
#5467=LINE('',#34302,#7288);
#5468=LINE('',#34306,#7289);
#5469=LINE('',#34311,#7290);
#5470=LINE('',#34315,#7291);
#5471=LINE('',#34319,#7292);
#5472=LINE('',#34324,#7293);
#5473=LINE('',#34328,#7294);
#5474=LINE('',#34332,#7295);
#5475=LINE('',#34337,#7296);
#5476=LINE('',#34341,#7297);
#5477=LINE('',#34345,#7298);
#5478=LINE('',#34350,#7299);
#5479=LINE('',#34354,#7300);
#5480=LINE('',#34358,#7301);
#5481=LINE('',#34363,#7302);
#5482=LINE('',#34367,#7303);
#5483=LINE('',#34371,#7304);
#5484=LINE('',#34376,#7305);
#5485=LINE('',#34380,#7306);
#5486=LINE('',#34384,#7307);
#5487=LINE('',#34389,#7308);
#5488=LINE('',#34393,#7309);
#5489=LINE('',#34397,#7310);
#5490=LINE('',#34402,#7311);
#5491=LINE('',#34406,#7312);
#5492=LINE('',#34410,#7313);
#5493=LINE('',#34416,#7314);
#5494=LINE('',#34425,#7315);
#5495=LINE('',#34431,#7316);
#5496=LINE('',#34438,#7317);
#5497=LINE('',#34444,#7318);
#5498=LINE('',#34449,#7319);
#5499=LINE('',#34454,#7320);
#5500=LINE('',#34458,#7321);
#5501=LINE('',#34462,#7322);
#5502=LINE('',#34467,#7323);
#5503=LINE('',#34471,#7324);
#5504=LINE('',#34475,#7325);
#5505=LINE('',#34480,#7326);
#5506=LINE('',#34484,#7327);
#5507=LINE('',#34488,#7328);
#5508=LINE('',#34493,#7329);
#5509=LINE('',#34497,#7330);
#5510=LINE('',#34501,#7331);
#5511=LINE('',#34506,#7332);
#5512=LINE('',#34510,#7333);
#5513=LINE('',#34514,#7334);
#5514=LINE('',#34520,#7335);
#5515=LINE('',#34524,#7336);
#5516=LINE('',#34528,#7337);
#5517=LINE('',#34535,#7338);
#5518=LINE('',#34541,#7339);
#5519=LINE('',#34545,#7340);
#5520=LINE('',#34549,#7341);
#5521=LINE('',#34556,#7342);
#5522=LINE('',#34562,#7343);
#5523=LINE('',#34566,#7344);
#5524=LINE('',#34570,#7345);
#5525=LINE('',#34577,#7346);
#5526=LINE('',#34583,#7347);
#5527=LINE('',#34587,#7348);
#5528=LINE('',#34591,#7349);
#5529=LINE('',#34598,#7350);
#5530=LINE('',#34604,#7351);
#5531=LINE('',#34608,#7352);
#5532=LINE('',#34612,#7353);
#5533=LINE('',#34619,#7354);
#5534=LINE('',#34625,#7355);
#5535=LINE('',#34629,#7356);
#5536=LINE('',#34633,#7357);
#5537=LINE('',#34640,#7358);
#5538=LINE('',#34646,#7359);
#5539=LINE('',#34650,#7360);
#5540=LINE('',#34654,#7361);
#5541=LINE('',#34661,#7362);
#5542=LINE('',#34667,#7363);
#5543=LINE('',#34671,#7364);
#5544=LINE('',#34675,#7365);
#5545=LINE('',#34682,#7366);
#5546=LINE('',#34688,#7367);
#5547=LINE('',#34692,#7368);
#5548=LINE('',#34696,#7369);
#5549=LINE('',#34703,#7370);
#5550=LINE('',#34709,#7371);
#5551=LINE('',#34713,#7372);
#5552=LINE('',#34717,#7373);
#5553=LINE('',#34724,#7374);
#5554=LINE('',#34730,#7375);
#5555=LINE('',#34734,#7376);
#5556=LINE('',#34738,#7377);
#5557=LINE('',#34745,#7378);
#5558=LINE('',#34751,#7379);
#5559=LINE('',#34755,#7380);
#5560=LINE('',#34759,#7381);
#5561=LINE('',#34766,#7382);
#5562=LINE('',#34772,#7383);
#5563=LINE('',#34781,#7384);
#5564=LINE('',#34787,#7385);
#5565=LINE('',#34798,#7386);
#5566=LINE('',#34805,#7387);
#5567=LINE('',#34812,#7388);
#5568=LINE('',#34816,#7389);
#5569=LINE('',#34820,#7390);
#5570=LINE('',#34828,#7391);
#5571=LINE('',#34832,#7392);
#5572=LINE('',#34836,#7393);
#5573=LINE('',#34840,#7394);
#5574=LINE('',#34850,#7395);
#5575=LINE('',#34853,#7396);
#5576=LINE('',#34856,#7397);
#5577=LINE('',#34860,#7398);
#5578=LINE('',#34868,#7399);
#5579=LINE('',#34872,#7400);
#5580=LINE('',#34876,#7401);
#5581=LINE('',#34880,#7402);
#5582=LINE('',#34890,#7403);
#5583=LINE('',#34893,#7404);
#5584=LINE('',#34896,#7405);
#5585=LINE('',#34900,#7406);
#5586=LINE('',#34908,#7407);
#5587=LINE('',#34912,#7408);
#5588=LINE('',#34916,#7409);
#5589=LINE('',#34920,#7410);
#5590=LINE('',#34930,#7411);
#5591=LINE('',#34933,#7412);
#5592=LINE('',#34936,#7413);
#5593=LINE('',#34940,#7414);
#5594=LINE('',#34944,#7415);
#5595=LINE('',#34948,#7416);
#5596=LINE('',#34952,#7417);
#5597=LINE('',#34956,#7418);
#5598=LINE('',#34960,#7419);
#5599=LINE('',#34964,#7420);
#5600=LINE('',#34968,#7421);
#5601=LINE('',#34972,#7422);
#5602=LINE('',#34976,#7423);
#5603=LINE('',#34980,#7424);
#5604=LINE('',#34984,#7425);
#5605=LINE('',#34988,#7426);
#5606=LINE('',#34992,#7427);
#5607=LINE('',#34996,#7428);
#5608=LINE('',#35000,#7429);
#5609=LINE('',#35004,#7430);
#5610=LINE('',#35008,#7431);
#5611=LINE('',#35012,#7432);
#5612=LINE('',#35016,#7433);
#5613=LINE('',#35020,#7434);
#5614=LINE('',#35024,#7435);
#5615=LINE('',#35028,#7436);
#5616=LINE('',#35032,#7437);
#5617=LINE('',#35036,#7438);
#5618=LINE('',#35040,#7439);
#5619=LINE('',#35044,#7440);
#5620=LINE('',#35048,#7441);
#5621=LINE('',#35052,#7442);
#5622=LINE('',#35056,#7443);
#5623=LINE('',#35060,#7444);
#5624=LINE('',#35064,#7445);
#5625=LINE('',#35068,#7446);
#5626=LINE('',#35072,#7447);
#5627=LINE('',#35076,#7448);
#5628=LINE('',#35080,#7449);
#5629=LINE('',#35084,#7450);
#5630=LINE('',#35088,#7451);
#5631=LINE('',#35092,#7452);
#5632=LINE('',#35096,#7453);
#5633=LINE('',#35100,#7454);
#5634=LINE('',#35104,#7455);
#5635=LINE('',#35108,#7456);
#5636=LINE('',#35112,#7457);
#5637=LINE('',#35116,#7458);
#5638=LINE('',#35120,#7459);
#5639=LINE('',#35124,#7460);
#5640=LINE('',#35128,#7461);
#5641=LINE('',#35132,#7462);
#5642=LINE('',#35136,#7463);
#5643=LINE('',#35140,#7464);
#5644=LINE('',#35144,#7465);
#5645=LINE('',#35148,#7466);
#5646=LINE('',#35154,#7467);
#5647=LINE('',#35157,#7468);
#5648=LINE('',#35162,#7469);
#5649=LINE('',#35163,#7470);
#5650=LINE('',#35166,#7471);
#5651=LINE('',#35167,#7472);
#5652=LINE('',#35172,#7473);
#5653=LINE('',#35173,#7474);
#5654=LINE('',#35175,#7475);
#5655=LINE('',#35181,#7476);
#5656=LINE('',#35182,#7477);
#5657=LINE('',#35185,#7478);
#5658=LINE('',#35186,#7479);
#5659=LINE('',#35191,#7480);
#5660=LINE('',#35192,#7481);
#5661=LINE('',#35194,#7482);
#5662=LINE('',#35196,#7483);
#5663=LINE('',#35199,#7484);
#5664=LINE('',#35205,#7485);
#5665=LINE('',#35206,#7486);
#5666=LINE('',#35209,#7487);
#5667=LINE('',#35210,#7488);
#5668=LINE('',#35215,#7489);
#5669=LINE('',#35216,#7490);
#5670=LINE('',#35218,#7491);
#5671=LINE('',#35220,#7492);
#5672=LINE('',#35223,#7493);
#5673=LINE('',#35227,#7494);
#5674=LINE('',#35230,#7495);
#5675=LINE('',#35235,#7496);
#5676=LINE('',#35236,#7497);
#5677=LINE('',#35239,#7498);
#5678=LINE('',#35240,#7499);
#5679=LINE('',#35245,#7500);
#5680=LINE('',#35246,#7501);
#5681=LINE('',#35248,#7502);
#5682=LINE('',#35250,#7503);
#5683=LINE('',#35253,#7504);
#5684=LINE('',#35259,#7505);
#5685=LINE('',#35260,#7506);
#5686=LINE('',#35263,#7507);
#5687=LINE('',#35264,#7508);
#5688=LINE('',#35269,#7509);
#5689=LINE('',#35270,#7510);
#5690=LINE('',#35272,#7511);
#5691=LINE('',#35274,#7512);
#5692=LINE('',#35277,#7513);
#5693=LINE('',#35283,#7514);
#5694=LINE('',#35284,#7515);
#5695=LINE('',#35287,#7516);
#5696=LINE('',#35288,#7517);
#5697=LINE('',#35293,#7518);
#5698=LINE('',#35294,#7519);
#5699=LINE('',#35297,#7520);
#5700=LINE('',#35302,#7521);
#5701=LINE('',#35304,#7522);
#5702=LINE('',#35306,#7523);
#5703=LINE('',#35311,#7524);
#5704=LINE('',#35312,#7525);
#5705=LINE('',#35315,#7526);
#5706=LINE('',#35316,#7527);
#5707=LINE('',#35321,#7528);
#5708=LINE('',#35322,#7529);
#5709=LINE('',#35324,#7530);
#5710=LINE('',#35326,#7531);
#5711=LINE('',#35329,#7532);
#5712=LINE('',#35335,#7533);
#5713=LINE('',#35336,#7534);
#5714=LINE('',#35339,#7535);
#5715=LINE('',#35340,#7536);
#5716=LINE('',#35345,#7537);
#5717=LINE('',#35346,#7538);
#5718=LINE('',#35348,#7539);
#5719=LINE('',#35350,#7540);
#5720=LINE('',#35353,#7541);
#5721=LINE('',#35357,#7542);
#5722=LINE('',#35360,#7543);
#5723=LINE('',#35363,#7544);
#5724=LINE('',#35367,#7545);
#5725=LINE('',#35370,#7546);
#5726=LINE('',#35372,#7547);
#5727=LINE('',#35374,#7548);
#5728=LINE('',#35379,#7549);
#5729=LINE('',#35380,#7550);
#5730=LINE('',#35383,#7551);
#5731=LINE('',#35384,#7552);
#5732=LINE('',#35389,#7553);
#5733=LINE('',#35390,#7554);
#5734=LINE('',#35392,#7555);
#5735=LINE('',#35394,#7556);
#5736=LINE('',#35397,#7557);
#5737=LINE('',#35403,#7558);
#5738=LINE('',#35404,#7559);
#5739=LINE('',#35407,#7560);
#5740=LINE('',#35408,#7561);
#5741=LINE('',#35413,#7562);
#5742=LINE('',#35414,#7563);
#5743=LINE('',#35416,#7564);
#5744=LINE('',#35418,#7565);
#5745=LINE('',#35421,#7566);
#5746=LINE('',#35427,#7567);
#5747=LINE('',#35428,#7568);
#5748=LINE('',#35431,#7569);
#5749=LINE('',#35432,#7570);
#5750=LINE('',#35437,#7571);
#5751=LINE('',#35438,#7572);
#5752=LINE('',#35441,#7573);
#5753=LINE('',#35446,#7574);
#5754=LINE('',#35448,#7575);
#5755=LINE('',#35450,#7576);
#5756=LINE('',#35455,#7577);
#5757=LINE('',#35456,#7578);
#5758=LINE('',#35459,#7579);
#5759=LINE('',#35460,#7580);
#5760=LINE('',#35465,#7581);
#5761=LINE('',#35466,#7582);
#5762=LINE('',#35468,#7583);
#5763=LINE('',#35470,#7584);
#5764=LINE('',#35473,#7585);
#5765=LINE('',#35479,#7586);
#5766=LINE('',#35480,#7587);
#5767=LINE('',#35483,#7588);
#5768=LINE('',#35484,#7589);
#5769=LINE('',#35489,#7590);
#5770=LINE('',#35490,#7591);
#5771=LINE('',#35492,#7592);
#5772=LINE('',#35494,#7593);
#5773=LINE('',#35497,#7594);
#5774=LINE('',#35503,#7595);
#5775=LINE('',#35504,#7596);
#5776=LINE('',#35507,#7597);
#5777=LINE('',#35508,#7598);
#5778=LINE('',#35513,#7599);
#5779=LINE('',#35514,#7600);
#5780=LINE('',#35516,#7601);
#5781=LINE('',#35518,#7602);
#5782=LINE('',#35521,#7603);
#5783=LINE('',#35525,#7604);
#5784=LINE('',#35528,#7605);
#5785=LINE('',#35533,#7606);
#5786=LINE('',#35534,#7607);
#5787=LINE('',#35537,#7608);
#5788=LINE('',#35538,#7609);
#5789=LINE('',#35543,#7610);
#5790=LINE('',#35544,#7611);
#5791=LINE('',#35546,#7612);
#5792=LINE('',#35548,#7613);
#5793=LINE('',#35551,#7614);
#5794=LINE('',#35557,#7615);
#5795=LINE('',#35558,#7616);
#5796=LINE('',#35561,#7617);
#5797=LINE('',#35562,#7618);
#5798=LINE('',#35567,#7619);
#5799=LINE('',#35568,#7620);
#5800=LINE('',#35570,#7621);
#5801=LINE('',#35572,#7622);
#5802=LINE('',#35575,#7623);
#5803=LINE('',#35579,#7624);
#5804=LINE('',#35582,#7625);
#5805=LINE('',#35585,#7626);
#5806=LINE('',#35589,#7627);
#5807=LINE('',#35592,#7628);
#5808=LINE('',#35594,#7629);
#5809=LINE('',#35596,#7630);
#5810=LINE('',#35601,#7631);
#5811=LINE('',#35602,#7632);
#5812=LINE('',#35605,#7633);
#5813=LINE('',#35606,#7634);
#5814=LINE('',#35611,#7635);
#5815=LINE('',#35612,#7636);
#5816=LINE('',#35614,#7637);
#5817=LINE('',#35616,#7638);
#5818=LINE('',#35619,#7639);
#5819=LINE('',#35625,#7640);
#5820=LINE('',#35626,#7641);
#5821=LINE('',#35629,#7642);
#5822=LINE('',#35630,#7643);
#5823=LINE('',#35635,#7644);
#5824=LINE('',#35636,#7645);
#5825=LINE('',#35638,#7646);
#5826=LINE('',#35640,#7647);
#5827=LINE('',#35643,#7648);
#5828=LINE('',#35647,#7649);
#5829=LINE('',#35650,#7650);
#5830=LINE('',#35655,#7651);
#5831=LINE('',#35656,#7652);
#5832=LINE('',#35658,#7653);
#5833=LINE('',#35660,#7654);
#5834=LINE('',#35663,#7655);
#5835=LINE('',#35668,#7656);
#5836=LINE('',#35669,#7657);
#5837=LINE('',#35672,#7658);
#5838=LINE('',#35673,#7659);
#5839=LINE('',#35678,#7660);
#5840=LINE('',#35679,#7661);
#5841=LINE('',#35681,#7662);
#5842=LINE('',#35683,#7663);
#5843=LINE('',#35686,#7664);
#5844=LINE('',#35692,#7665);
#5845=LINE('',#35693,#7666);
#5846=LINE('',#35696,#7667);
#5847=LINE('',#35697,#7668);
#5848=LINE('',#35702,#7669);
#5849=LINE('',#35703,#7670);
#5850=LINE('',#35705,#7671);
#5851=LINE('',#35707,#7672);
#5852=LINE('',#35710,#7673);
#5853=LINE('',#35716,#7674);
#5854=LINE('',#35717,#7675);
#5855=LINE('',#35720,#7676);
#5856=LINE('',#35721,#7677);
#5857=LINE('',#35726,#7678);
#5858=LINE('',#35727,#7679);
#5859=LINE('',#35729,#7680);
#5860=LINE('',#35731,#7681);
#5861=LINE('',#35734,#7682);
#5862=LINE('',#35740,#7683);
#5863=LINE('',#35741,#7684);
#5864=LINE('',#35743,#7685);
#5865=LINE('',#35745,#7686);
#5866=LINE('',#35748,#7687);
#5867=LINE('',#35753,#7688);
#5868=LINE('',#35754,#7689);
#5869=LINE('',#35757,#7690);
#5870=LINE('',#35758,#7691);
#5871=LINE('',#35763,#7692);
#5872=LINE('',#35764,#7693);
#5873=LINE('',#35766,#7694);
#5874=LINE('',#35772,#7695);
#5875=LINE('',#35773,#7696);
#5876=LINE('',#35775,#7697);
#5877=LINE('',#35777,#7698);
#5878=LINE('',#35780,#7699);
#5879=LINE('',#35785,#7700);
#5880=LINE('',#35786,#7701);
#5881=LINE('',#35788,#7702);
#5882=LINE('',#35794,#7703);
#5883=LINE('',#35795,#7704);
#5884=LINE('',#35797,#7705);
#5885=LINE('',#35799,#7706);
#5886=LINE('',#35802,#7707);
#5887=LINE('',#35807,#7708);
#5888=LINE('',#35808,#7709);
#5889=LINE('',#35810,#7710);
#5890=LINE('',#35818,#7711);
#5891=LINE('',#35823,#7712);
#5892=LINE('',#35856,#7713);
#5893=LINE('',#35862,#7714);
#5894=LINE('',#35864,#7715);
#5895=LINE('',#35870,#7716);
#5896=LINE('',#35876,#7717);
#5897=LINE('',#35885,#7718);
#5898=LINE('',#35894,#7719);
#5899=LINE('',#35899,#7720);
#5900=LINE('',#35905,#7721);
#5901=LINE('',#35911,#7722);
#5902=LINE('',#35918,#7723);
#5903=LINE('',#35922,#7724);
#5904=LINE('',#35925,#7725);
#5905=LINE('',#35935,#7726);
#5906=LINE('',#35937,#7727);
#5907=LINE('',#35944,#7728);
#5908=LINE('',#35952,#7729);
#5909=LINE('',#35955,#7730);
#5910=LINE('',#35961,#7731);
#5911=LINE('',#35975,#7732);
#5912=LINE('',#35979,#7733);
#5913=LINE('',#35983,#7734);
#5914=LINE('',#35986,#7735);
#5915=LINE('',#35995,#7736);
#5916=LINE('',#35999,#7737);
#5917=LINE('',#36003,#7738);
#5918=LINE('',#36008,#7739);
#5919=LINE('',#36017,#7740);
#5920=LINE('',#36021,#7741);
#5921=LINE('',#36053,#7742);
#5922=LINE('',#36061,#7743);
#5923=LINE('',#36066,#7744);
#5924=LINE('',#36074,#7745);
#5925=LINE('',#36077,#7746);
#5926=LINE('',#36081,#7747);
#5927=LINE('',#36085,#7748);
#5928=LINE('',#36090,#7749);
#5929=LINE('',#36094,#7750);
#5930=LINE('',#36098,#7751);
#5931=LINE('',#36103,#7752);
#5932=LINE('',#36111,#7753);
#5933=LINE('',#36117,#7754);
#5934=LINE('',#36123,#7755);
#5935=LINE('',#36127,#7756);
#5936=LINE('',#36133,#7757);
#5937=LINE('',#36139,#7758);
#5938=LINE('',#36145,#7759);
#5939=LINE('',#36151,#7760);
#5940=LINE('',#36157,#7761);
#5941=LINE('',#36163,#7762);
#5942=LINE('',#36169,#7763);
#5943=LINE('',#36178,#7764);
#5944=LINE('',#36184,#7765);
#5945=LINE('',#36191,#7766);
#5946=LINE('',#36197,#7767);
#5947=LINE('',#36202,#7768);
#5948=LINE('',#36207,#7769);
#5949=LINE('',#36211,#7770);
#5950=LINE('',#36216,#7771);
#5951=LINE('',#36220,#7772);
#5952=LINE('',#36226,#7773);
#5953=LINE('',#36235,#7774);
#5954=LINE('',#36239,#7775);
#5955=LINE('',#36244,#7776);
#5956=LINE('',#36255,#7777);
#5957=LINE('',#36262,#7778);
#5958=LINE('',#36264,#7779);
#5959=LINE('',#36268,#7780);
#5960=LINE('',#36275,#7781);
#5961=LINE('',#36282,#7782);
#5962=LINE('',#36286,#7783);
#5963=LINE('',#36293,#7784);
#5964=LINE('',#36302,#7785);
#5965=LINE('',#36309,#7786);
#5966=LINE('',#36312,#7787);
#5967=LINE('',#36321,#7788);
#5968=LINE('',#36367,#7789);
#5969=LINE('',#36378,#7790);
#5970=LINE('',#36703,#7791);
#5971=LINE('',#36807,#7792);
#5972=LINE('',#36831,#7793);
#5973=LINE('',#36917,#7794);
#5974=LINE('',#36921,#7795);
#5975=LINE('',#36933,#7796);
#5976=LINE('',#36943,#7797);
#5977=LINE('',#36947,#7798);
#5978=LINE('',#36950,#7799);
#5979=LINE('',#36953,#7800);
#5980=LINE('',#36957,#7801);
#5981=LINE('',#36960,#7802);
#5982=LINE('',#36965,#7803);
#5983=LINE('',#36971,#7804);
#5984=LINE('',#36976,#7805);
#5985=LINE('',#36982,#7806);
#5986=LINE('',#36991,#7807);
#5987=LINE('',#37010,#7808);
#5988=LINE('',#37026,#7809);
#5989=LINE('',#37032,#7810);
#5990=LINE('',#37035,#7811);
#5991=LINE('',#37039,#7812);
#5992=LINE('',#37042,#7813);
#5993=LINE('',#37045,#7814);
#5994=LINE('',#37049,#7815);
#5995=LINE('',#37052,#7816);
#5996=LINE('',#37055,#7817);
#5997=LINE('',#37059,#7818);
#5998=LINE('',#37062,#7819);
#5999=LINE('',#37064,#7820);
#6000=LINE('',#37069,#7821);
#6001=LINE('',#37071,#7822);
#6002=LINE('',#37073,#7823);
#6003=LINE('',#37074,#7824);
#6004=LINE('',#37078,#7825);
#6005=LINE('',#37080,#7826);
#6006=LINE('',#37082,#7827);
#6007=LINE('',#37083,#7828);
#6008=LINE('',#37085,#7829);
#6009=LINE('',#37086,#7830);
#6010=LINE('',#37097,#7831);
#6011=LINE('',#37101,#7832);
#6012=LINE('',#37105,#7833);
#6013=LINE('',#37109,#7834);
#6014=LINE('',#37113,#7835);
#6015=LINE('',#37117,#7836);
#6016=LINE('',#37121,#7837);
#6017=LINE('',#37125,#7838);
#6018=LINE('',#37129,#7839);
#6019=LINE('',#37133,#7840);
#6020=LINE('',#37137,#7841);
#6021=LINE('',#37141,#7842);
#6022=LINE('',#37150,#7843);
#6023=LINE('',#37154,#7844);
#6024=LINE('',#37158,#7845);
#6025=LINE('',#37161,#7846);
#6026=LINE('',#37163,#7847);
#6027=LINE('',#37164,#7848);
#6028=LINE('',#37167,#7849);
#6029=LINE('',#37171,#7850);
#6030=LINE('',#37172,#7851);
#6031=LINE('',#37177,#7852);
#6032=LINE('',#37179,#7853);
#6033=LINE('',#37180,#7854);
#6034=LINE('',#37183,#7855);
#6035=LINE('',#37187,#7856);
#6036=LINE('',#37188,#7857);
#6037=LINE('',#37193,#7858);
#6038=LINE('',#37195,#7859);
#6039=LINE('',#37196,#7860);
#6040=LINE('',#37199,#7861);
#6041=LINE('',#37203,#7862);
#6042=LINE('',#37204,#7863);
#6043=LINE('',#37209,#7864);
#6044=LINE('',#37211,#7865);
#6045=LINE('',#37212,#7866);
#6046=LINE('',#37215,#7867);
#6047=LINE('',#37219,#7868);
#6048=LINE('',#37220,#7869);
#6049=LINE('',#37225,#7870);
#6050=LINE('',#37227,#7871);
#6051=LINE('',#37228,#7872);
#6052=LINE('',#37231,#7873);
#6053=LINE('',#37235,#7874);
#6054=LINE('',#37236,#7875);
#6055=LINE('',#37241,#7876);
#6056=LINE('',#37243,#7877);
#6057=LINE('',#37244,#7878);
#6058=LINE('',#37247,#7879);
#6059=LINE('',#37251,#7880);
#6060=LINE('',#37252,#7881);
#6061=LINE('',#37258,#7882);
#6062=LINE('',#37264,#7883);
#6063=LINE('',#37266,#7884);
#6064=LINE('',#37268,#7885);
#6065=LINE('',#37269,#7886);
#6066=LINE('',#37272,#7887);
#6067=LINE('',#37274,#7888);
#6068=LINE('',#37275,#7889);
#6069=LINE('',#37278,#7890);
#6070=LINE('',#37280,#7891);
#6071=LINE('',#37282,#7892);
#6072=LINE('',#37284,#7893);
#6073=LINE('',#37286,#7894);
#6074=LINE('',#37288,#7895);
#6075=LINE('',#37290,#7896);
#6076=LINE('',#37292,#7897);
#6077=LINE('',#37294,#7898);
#6078=LINE('',#37296,#7899);
#6079=LINE('',#37298,#7900);
#6080=LINE('',#37300,#7901);
#6081=LINE('',#37302,#7902);
#6082=LINE('',#37303,#7903);
#6083=LINE('',#37306,#7904);
#6084=LINE('',#37308,#7905);
#6085=LINE('',#37309,#7906);
#6086=LINE('',#37312,#7907);
#6087=LINE('',#37313,#7908);
#6088=LINE('',#37316,#7909);
#6089=LINE('',#37318,#7910);
#6090=LINE('',#37320,#7911);
#6091=LINE('',#37322,#7912);
#6092=LINE('',#37324,#7913);
#6093=LINE('',#37326,#7914);
#6094=LINE('',#37327,#7915);
#6095=LINE('',#37329,#7916);
#6096=LINE('',#37331,#7917);
#6097=LINE('',#37333,#7918);
#6098=LINE('',#37335,#7919);
#6099=LINE('',#37336,#7920);
#6100=LINE('',#37338,#7921);
#6101=LINE('',#37340,#7922);
#6102=LINE('',#37343,#7923);
#6103=LINE('',#37345,#7924);
#6104=LINE('',#37347,#7925);
#6105=LINE('',#37348,#7926);
#6106=LINE('',#37350,#7927);
#6107=LINE('',#37352,#7928);
#6108=LINE('',#37354,#7929);
#6109=LINE('',#37356,#7930);
#6110=LINE('',#37359,#7931);
#6111=LINE('',#37361,#7932);
#6112=LINE('',#37363,#7933);
#6113=LINE('',#37364,#7934);
#6114=LINE('',#37367,#7935);
#6115=LINE('',#37368,#7936);
#6116=LINE('',#37372,#7937);
#6117=LINE('',#37374,#7938);
#6118=LINE('',#37376,#7939);
#6119=LINE('',#37377,#7940);
#6120=LINE('',#37382,#7941);
#6121=LINE('',#37384,#7942);
#6122=LINE('',#37389,#7943);
#6123=LINE('',#37393,#7944);
#6124=LINE('',#37396,#7945);
#6125=LINE('',#37398,#7946);
#6126=LINE('',#37399,#7947);
#6127=LINE('',#37402,#7948);
#6128=LINE('',#37404,#7949);
#6129=LINE('',#37405,#7950);
#6130=LINE('',#37407,#7951);
#6131=LINE('',#37408,#7952);
#6132=LINE('',#37414,#7953);
#6133=LINE('',#37415,#7954);
#6134=LINE('',#37416,#7955);
#6135=LINE('',#37419,#7956);
#6136=LINE('',#37420,#7957);
#6137=LINE('',#37423,#7958);
#6138=LINE('',#37424,#7959);
#6139=LINE('',#37426,#7960);
#6140=LINE('',#37430,#7961);
#6141=LINE('',#37432,#7962);
#6142=LINE('',#37433,#7963);
#6143=LINE('',#37436,#7964);
#6144=LINE('',#37437,#7965);
#6145=LINE('',#37440,#7966);
#6146=LINE('',#37441,#7967);
#6147=LINE('',#37443,#7968);
#6148=LINE('',#37452,#7969);
#6149=LINE('',#37455,#7970);
#6150=LINE('',#37458,#7971);
#6151=LINE('',#37462,#7972);
#6152=LINE('',#37464,#7973);
#6153=LINE('',#37468,#7974);
#6154=LINE('',#37472,#7975);
#6155=LINE('',#37476,#7976);
#6156=LINE('',#37477,#7977);
#6157=LINE('',#37480,#7978);
#6158=LINE('',#37481,#7979);
#6159=LINE('',#37485,#7980);
#6160=LINE('',#37490,#7981);
#6161=LINE('',#37496,#7982);
#6162=LINE('',#37500,#7983);
#6163=LINE('',#37502,#7984);
#6164=LINE('',#37503,#7985);
#6165=LINE('',#37506,#7986);
#6166=LINE('',#37510,#7987);
#6167=LINE('',#37511,#7988);
#6168=LINE('',#37516,#7989);
#6169=LINE('',#37522,#7990);
#6170=LINE('',#37525,#7991);
#6171=LINE('',#37526,#7992);
#6172=LINE('',#37529,#7993);
#6173=LINE('',#37530,#7994);
#6174=LINE('',#37534,#7995);
#6175=LINE('',#37536,#7996);
#6176=LINE('',#37538,#7997);
#6177=LINE('',#37539,#7998);
#6178=LINE('',#37541,#7999);
#6179=LINE('',#37543,#8000);
#6180=LINE('',#37545,#8001);
#6181=LINE('',#37546,#8002);
#6182=LINE('',#37549,#8003);
#6183=LINE('',#37551,#8004);
#6184=LINE('',#37552,#8005);
#6185=LINE('',#37554,#8006);
#6186=LINE('',#37555,#8007);
#6187=LINE('',#37562,#8008);
#6188=LINE('',#37564,#8009);
#6189=LINE('',#37566,#8010);
#6190=LINE('',#37567,#8011);
#6191=LINE('',#37570,#8012);
#6192=LINE('',#37572,#8013);
#6193=LINE('',#37573,#8014);
#6194=LINE('',#37576,#8015);
#6195=LINE('',#37578,#8016);
#6196=LINE('',#37579,#8017);
#6197=LINE('',#37581,#8018);
#6198=LINE('',#37582,#8019);
#6199=LINE('',#37587,#8020);
#6200=LINE('',#37589,#8021);
#6201=LINE('',#37591,#8022);
#6202=LINE('',#37592,#8023);
#6203=LINE('',#37595,#8024);
#6204=LINE('',#37597,#8025);
#6205=LINE('',#37598,#8026);
#6206=LINE('',#37601,#8027);
#6207=LINE('',#37603,#8028);
#6208=LINE('',#37604,#8029);
#6209=LINE('',#37606,#8030);
#6210=LINE('',#37607,#8031);
#6211=LINE('',#37613,#8032);
#6212=LINE('',#37619,#8033);
#6213=LINE('',#37621,#8034);
#6214=LINE('',#37623,#8035);
#6215=LINE('',#37624,#8036);
#6216=LINE('',#37627,#8037);
#6217=LINE('',#37629,#8038);
#6218=LINE('',#37630,#8039);
#6219=LINE('',#37633,#8040);
#6220=LINE('',#37635,#8041);
#6221=LINE('',#37636,#8042);
#6222=LINE('',#37638,#8043);
#6223=LINE('',#37639,#8044);
#6224=LINE('',#37644,#8045);
#6225=LINE('',#37646,#8046);
#6226=LINE('',#37648,#8047);
#6227=LINE('',#37649,#8048);
#6228=LINE('',#37652,#8049);
#6229=LINE('',#37654,#8050);
#6230=LINE('',#37655,#8051);
#6231=LINE('',#37658,#8052);
#6232=LINE('',#37660,#8053);
#6233=LINE('',#37661,#8054);
#6234=LINE('',#37663,#8055);
#6235=LINE('',#37664,#8056);
#6236=LINE('',#37669,#8057);
#6237=LINE('',#37671,#8058);
#6238=LINE('',#37673,#8059);
#6239=LINE('',#37674,#8060);
#6240=LINE('',#37677,#8061);
#6241=LINE('',#37679,#8062);
#6242=LINE('',#37680,#8063);
#6243=LINE('',#37683,#8064);
#6244=LINE('',#37685,#8065);
#6245=LINE('',#37686,#8066);
#6246=LINE('',#37688,#8067);
#6247=LINE('',#37689,#8068);
#6248=LINE('',#37694,#8069);
#6249=LINE('',#37696,#8070);
#6250=LINE('',#37698,#8071);
#6251=LINE('',#37699,#8072);
#6252=LINE('',#37702,#8073);
#6253=LINE('',#37704,#8074);
#6254=LINE('',#37705,#8075);
#6255=LINE('',#37708,#8076);
#6256=LINE('',#37710,#8077);
#6257=LINE('',#37711,#8078);
#6258=LINE('',#37713,#8079);
#6259=LINE('',#37714,#8080);
#6260=LINE('',#37720,#8081);
#6261=LINE('',#37726,#8082);
#6262=LINE('',#37732,#8083);
#6263=LINE('',#37738,#8084);
#6264=LINE('',#37746,#8085);
#6265=LINE('',#37752,#8086);
#6266=LINE('',#37777,#8087);
#6267=LINE('',#37808,#8088);
#6268=LINE('',#37862,#8089);
#6269=LINE('',#37910,#8090);
#6270=LINE('',#37928,#8091);
#6271=LINE('',#37952,#8092);
#6272=LINE('',#37977,#8093);
#6273=LINE('',#38479,#8094);
#6274=LINE('',#38484,#8095);
#6275=LINE('',#38486,#8096);
#6276=LINE('',#38488,#8097);
#6277=LINE('',#38489,#8098);
#6278=LINE('',#38492,#8099);
#6279=LINE('',#38494,#8100);
#6280=LINE('',#38495,#8101);
#6281=LINE('',#38498,#8102);
#6282=LINE('',#38500,#8103);
#6283=LINE('',#38501,#8104);
#6284=LINE('',#38504,#8105);
#6285=LINE('',#38506,#8106);
#6286=LINE('',#38507,#8107);
#6287=LINE('',#38510,#8108);
#6288=LINE('',#38512,#8109);
#6289=LINE('',#38513,#8110);
#6290=LINE('',#38515,#8111);
#6291=LINE('',#38516,#8112);
#6292=LINE('',#38522,#8113);
#6293=LINE('',#38526,#8114);
#6294=LINE('',#38532,#8115);
#6295=LINE('',#38556,#8116);
#6296=LINE('',#38579,#8117);
#6297=LINE('',#38627,#8118);
#6298=LINE('',#38675,#8119);
#6299=LINE('',#38729,#8120);
#6300=LINE('',#38777,#8121);
#6301=LINE('',#38825,#8122);
#6302=LINE('',#38876,#8123);
#6303=LINE('',#38924,#8124);
#6304=LINE('',#38948,#8125);
#6305=LINE('',#38973,#8126);
#6306=LINE('',#38998,#8127);
#6307=LINE('',#39022,#8128);
#6308=LINE('',#39047,#8129);
#6309=LINE('',#39072,#8130);
#6310=LINE('',#39096,#8131);
#6311=LINE('',#39801,#8132);
#6312=LINE('',#39805,#8133);
#6313=LINE('',#39809,#8134);
#6314=LINE('',#39879,#8135);
#6315=LINE('',#39885,#8136);
#6316=LINE('',#39890,#8137);
#6317=LINE('',#39891,#8138);
#6318=LINE('',#39898,#8139);
#6319=LINE('',#39903,#8140);
#6320=LINE('',#39904,#8141);
#6321=LINE('',#39911,#8142);
#6322=LINE('',#39916,#8143);
#6323=LINE('',#39917,#8144);
#6324=LINE('',#39919,#8145);
#6325=LINE('',#39920,#8146);
#6326=LINE('',#39921,#8147);
#6327=LINE('',#39928,#8148);
#6328=LINE('',#39933,#8149);
#6329=LINE('',#39964,#8150);
#6330=LINE('',#39965,#8151);
#6331=LINE('',#39970,#8152);
#6332=LINE('',#39972,#8153);
#6333=LINE('',#39978,#8154);
#6334=LINE('',#39996,#8155);
#6335=LINE('',#40013,#8156);
#6336=LINE('',#40061,#8157);
#6337=LINE('',#40112,#8158);
#6338=LINE('',#40160,#8159);
#6339=LINE('',#40208,#8160);
#6340=LINE('',#40262,#8161);
#6341=LINE('',#40310,#8162);
#6342=LINE('',#40358,#8163);
#6343=LINE('',#40412,#8164);
#6344=LINE('',#40460,#8165);
#6345=LINE('',#40508,#8166);
#6346=LINE('',#40556,#8167);
#6347=LINE('',#40607,#8168);
#6348=LINE('',#40655,#8169);
#6349=LINE('',#40703,#8170);
#6350=LINE('',#40757,#8171);
#6351=LINE('',#40805,#8172);
#6352=LINE('',#40853,#8173);
#6353=LINE('',#40907,#8174);
#6354=LINE('',#40955,#8175);
#6355=LINE('',#41003,#8176);
#6356=LINE('',#41051,#8177);
#6357=LINE('',#41102,#8178);
#6358=LINE('',#41150,#8179);
#6359=LINE('',#41198,#8180);
#6360=LINE('',#41252,#8181);
#6361=LINE('',#41300,#8182);
#6362=LINE('',#41348,#8183);
#6363=LINE('',#41367,#8184);
#6364=LINE('',#41392,#8185);
#6365=LINE('',#41416,#8186);
#6366=LINE('',#41441,#8187);
#6367=LINE('',#41466,#8188);
#6368=LINE('',#41490,#8189);
#6369=LINE('',#41515,#8190);
#6370=LINE('',#41539,#8191);
#6371=LINE('',#41564,#8192);
#6372=LINE('',#41588,#8193);
#6373=LINE('',#41613,#8194);
#6374=LINE('',#41638,#8195);
#6375=LINE('',#41662,#8196);
#6376=LINE('',#41687,#8197);
#6377=LINE('',#41712,#8198);
#6378=LINE('',#41736,#8199);
#6379=LINE('',#41761,#8200);
#6380=LINE('',#41786,#8201);
#6381=LINE('',#41810,#8202);
#6382=LINE('',#41834,#8203);
#6383=LINE('',#41859,#8204);
#6384=LINE('',#41884,#8205);
#6385=LINE('',#41908,#8206);
#6386=LINE('',#41933,#8207);
#6387=LINE('',#41958,#8208);
#6388=LINE('',#41982,#8209);
#6389=LINE('',#42007,#8210);
#6390=LINE('',#42032,#8211);
#6391=LINE('',#43776,#8212);
#6392=LINE('',#43777,#8213);
#6393=LINE('',#43780,#8214);
#6394=LINE('',#43782,#8215);
#6395=LINE('',#43788,#8216);
#6396=LINE('',#43797,#8217);
#6397=LINE('',#43798,#8218);
#6398=LINE('',#43801,#8219);
#6399=LINE('',#43803,#8220);
#6400=LINE('',#43809,#8221);
#6401=LINE('',#43818,#8222);
#6402=LINE('',#43819,#8223);
#6403=LINE('',#43822,#8224);
#6404=LINE('',#43824,#8225);
#6405=LINE('',#43830,#8226);
#6406=LINE('',#43839,#8227);
#6407=LINE('',#43840,#8228);
#6408=LINE('',#43843,#8229);
#6409=LINE('',#43845,#8230);
#6410=LINE('',#43851,#8231);
#6411=LINE('',#43860,#8232);
#6412=LINE('',#43861,#8233);
#6413=LINE('',#43864,#8234);
#6414=LINE('',#43866,#8235);
#6415=LINE('',#43872,#8236);
#6416=LINE('',#43881,#8237);
#6417=LINE('',#43882,#8238);
#6418=LINE('',#43885,#8239);
#6419=LINE('',#43887,#8240);
#6420=LINE('',#43893,#8241);
#6421=LINE('',#43902,#8242);
#6422=LINE('',#43903,#8243);
#6423=LINE('',#43906,#8244);
#6424=LINE('',#43908,#8245);
#6425=LINE('',#43914,#8246);
#6426=LINE('',#43923,#8247);
#6427=LINE('',#43924,#8248);
#6428=LINE('',#43927,#8249);
#6429=LINE('',#43929,#8250);
#6430=LINE('',#43935,#8251);
#6431=LINE('',#43944,#8252);
#6432=LINE('',#43945,#8253);
#6433=LINE('',#43948,#8254);
#6434=LINE('',#43950,#8255);
#6435=LINE('',#43956,#8256);
#6436=LINE('',#43965,#8257);
#6437=LINE('',#43966,#8258);
#6438=LINE('',#43969,#8259);
#6439=LINE('',#43971,#8260);
#6440=LINE('',#43977,#8261);
#6441=LINE('',#43986,#8262);
#6442=LINE('',#43987,#8263);
#6443=LINE('',#43990,#8264);
#6444=LINE('',#43992,#8265);
#6445=LINE('',#43998,#8266);
#6446=LINE('',#44007,#8267);
#6447=LINE('',#44008,#8268);
#6448=LINE('',#44011,#8269);
#6449=LINE('',#44013,#8270);
#6450=LINE('',#44019,#8271);
#6451=LINE('',#44028,#8272);
#6452=LINE('',#44029,#8273);
#6453=LINE('',#44032,#8274);
#6454=LINE('',#44034,#8275);
#6455=LINE('',#44040,#8276);
#6456=LINE('',#44049,#8277);
#6457=LINE('',#44050,#8278);
#6458=LINE('',#44053,#8279);
#6459=LINE('',#44055,#8280);
#6460=LINE('',#44061,#8281);
#6461=LINE('',#44070,#8282);
#6462=LINE('',#44071,#8283);
#6463=LINE('',#44074,#8284);
#6464=LINE('',#44076,#8285);
#6465=LINE('',#44082,#8286);
#6466=LINE('',#44091,#8287);
#6467=LINE('',#44092,#8288);
#6468=LINE('',#44095,#8289);
#6469=LINE('',#44097,#8290);
#6470=LINE('',#44103,#8291);
#6471=LINE('',#44112,#8292);
#6472=LINE('',#44113,#8293);
#6473=LINE('',#44116,#8294);
#6474=LINE('',#44118,#8295);
#6475=LINE('',#44124,#8296);
#6476=LINE('',#44133,#8297);
#6477=LINE('',#44135,#8298);
#6478=LINE('',#44139,#8299);
#6479=LINE('',#44141,#8300);
#6480=LINE('',#44147,#8301);
#6481=LINE('',#44156,#8302);
#6482=LINE('',#44157,#8303);
#6483=LINE('',#44160,#8304);
#6484=LINE('',#44162,#8305);
#6485=LINE('',#44168,#8306);
#6486=LINE('',#44177,#8307);
#6487=LINE('',#44178,#8308);
#6488=LINE('',#44181,#8309);
#6489=LINE('',#44183,#8310);
#6490=LINE('',#44189,#8311);
#6491=LINE('',#44198,#8312);
#6492=LINE('',#44199,#8313);
#6493=LINE('',#44202,#8314);
#6494=LINE('',#44204,#8315);
#6495=LINE('',#44210,#8316);
#6496=LINE('',#44219,#8317);
#6497=LINE('',#44220,#8318);
#6498=LINE('',#44223,#8319);
#6499=LINE('',#44225,#8320);
#6500=LINE('',#44231,#8321);
#6501=LINE('',#44240,#8322);
#6502=LINE('',#44241,#8323);
#6503=LINE('',#44244,#8324);
#6504=LINE('',#44246,#8325);
#6505=LINE('',#44252,#8326);
#6506=LINE('',#44261,#8327);
#6507=LINE('',#44262,#8328);
#6508=LINE('',#44265,#8329);
#6509=LINE('',#44267,#8330);
#6510=LINE('',#44273,#8331);
#6511=LINE('',#44282,#8332);
#6512=LINE('',#44283,#8333);
#6513=LINE('',#44286,#8334);
#6514=LINE('',#44288,#8335);
#6515=LINE('',#44294,#8336);
#6516=LINE('',#44303,#8337);
#6517=LINE('',#44304,#8338);
#6518=LINE('',#44307,#8339);
#6519=LINE('',#44309,#8340);
#6520=LINE('',#44315,#8341);
#6521=LINE('',#44324,#8342);
#6522=LINE('',#44325,#8343);
#6523=LINE('',#44328,#8344);
#6524=LINE('',#44330,#8345);
#6525=LINE('',#44336,#8346);
#6526=LINE('',#44345,#8347);
#6527=LINE('',#44346,#8348);
#6528=LINE('',#44349,#8349);
#6529=LINE('',#44351,#8350);
#6530=LINE('',#44357,#8351);
#6531=LINE('',#44366,#8352);
#6532=LINE('',#44367,#8353);
#6533=LINE('',#44370,#8354);
#6534=LINE('',#44372,#8355);
#6535=LINE('',#44378,#8356);
#6536=LINE('',#44387,#8357);
#6537=LINE('',#44388,#8358);
#6538=LINE('',#44391,#8359);
#6539=LINE('',#44393,#8360);
#6540=LINE('',#44399,#8361);
#6541=LINE('',#44408,#8362);
#6542=LINE('',#44409,#8363);
#6543=LINE('',#44412,#8364);
#6544=LINE('',#44414,#8365);
#6545=LINE('',#44420,#8366);
#6546=LINE('',#44429,#8367);
#6547=LINE('',#44430,#8368);
#6548=LINE('',#44433,#8369);
#6549=LINE('',#44435,#8370);
#6550=LINE('',#44441,#8371);
#6551=LINE('',#44450,#8372);
#6552=LINE('',#44451,#8373);
#6553=LINE('',#44454,#8374);
#6554=LINE('',#44456,#8375);
#6555=LINE('',#44462,#8376);
#6556=LINE('',#44471,#8377);
#6557=LINE('',#44472,#8378);
#6558=LINE('',#44475,#8379);
#6559=LINE('',#44477,#8380);
#6560=LINE('',#44483,#8381);
#6561=LINE('',#44492,#8382);
#6562=LINE('',#44493,#8383);
#6563=LINE('',#44496,#8384);
#6564=LINE('',#44498,#8385);
#6565=LINE('',#44504,#8386);
#6566=LINE('',#44527,#8387);
#6567=LINE('',#44549,#8388);
#6568=LINE('',#44553,#8389);
#6569=LINE('',#44557,#8390);
#6570=LINE('',#44559,#8391);
#6571=LINE('',#44567,#8392);
#6572=LINE('',#44572,#8393);
#6573=LINE('',#44576,#8394);
#6574=LINE('',#44581,#8395);
#6575=LINE('',#44583,#8396);
#6576=LINE('',#44585,#8397);
#6577=LINE('',#44586,#8398);
#6578=LINE('',#44589,#8399);
#6579=LINE('',#44591,#8400);
#6580=LINE('',#44592,#8401);
#6581=LINE('',#44595,#8402);
#6582=LINE('',#44597,#8403);
#6583=LINE('',#44598,#8404);
#6584=LINE('',#44601,#8405);
#6585=LINE('',#44603,#8406);
#6586=LINE('',#44604,#8407);
#6587=LINE('',#44607,#8408);
#6588=LINE('',#44609,#8409);
#6589=LINE('',#44610,#8410);
#6590=LINE('',#44612,#8411);
#6591=LINE('',#44613,#8412);
#6592=LINE('',#44619,#8413);
#6593=LINE('',#44625,#8414);
#6594=LINE('',#44632,#8415);
#6595=LINE('',#44650,#8416);
#6596=LINE('',#44667,#8417);
#6597=LINE('',#44721,#8418);
#6598=LINE('',#44769,#8419);
#6599=LINE('',#44817,#8420);
#6600=LINE('',#44865,#8421);
#6601=LINE('',#44919,#8422);
#6602=LINE('',#44967,#8423);
#6603=LINE('',#45015,#8424);
#6604=LINE('',#45069,#8425);
#6605=LINE('',#45117,#8426);
#6606=LINE('',#45165,#8427);
#6607=LINE('',#45219,#8428);
#6608=LINE('',#45267,#8429);
#6609=LINE('',#45315,#8430);
#6610=LINE('',#45369,#8431);
#6611=LINE('',#45417,#8432);
#6612=LINE('',#45465,#8433);
#6613=LINE('',#45519,#8434);
#6614=LINE('',#45567,#8435);
#6615=LINE('',#45615,#8436);
#6616=LINE('',#45669,#8437);
#6617=LINE('',#45717,#8438);
#6618=LINE('',#45765,#8439);
#6619=LINE('',#45784,#8440);
#6620=LINE('',#45809,#8441);
#6621=LINE('',#45833,#8442);
#6622=LINE('',#45858,#8443);
#6623=LINE('',#45883,#8444);
#6624=LINE('',#45907,#8445);
#6625=LINE('',#45932,#8446);
#6626=LINE('',#45957,#8447);
#6627=LINE('',#45981,#8448);
#6628=LINE('',#46006,#8449);
#6629=LINE('',#46031,#8450);
#6630=LINE('',#46055,#8451);
#6631=LINE('',#46080,#8452);
#6632=LINE('',#46105,#8453);
#6633=LINE('',#46129,#8454);
#6634=LINE('',#46154,#8455);
#6635=LINE('',#46179,#8456);
#6636=LINE('',#46203,#8457);
#6637=LINE('',#46228,#8458);
#6638=LINE('',#46253,#8459);
#6639=LINE('',#46277,#8460);
#6640=LINE('',#46301,#8461);
#6641=LINE('',#46326,#8462);
#6642=LINE('',#47817,#8463);
#6643=LINE('',#47818,#8464);
#6644=LINE('',#47821,#8465);
#6645=LINE('',#47823,#8466);
#6646=LINE('',#47829,#8467);
#6647=LINE('',#47838,#8468);
#6648=LINE('',#47839,#8469);
#6649=LINE('',#47842,#8470);
#6650=LINE('',#47844,#8471);
#6651=LINE('',#47850,#8472);
#6652=LINE('',#47859,#8473);
#6653=LINE('',#47860,#8474);
#6654=LINE('',#47863,#8475);
#6655=LINE('',#47865,#8476);
#6656=LINE('',#47871,#8477);
#6657=LINE('',#47880,#8478);
#6658=LINE('',#47881,#8479);
#6659=LINE('',#47884,#8480);
#6660=LINE('',#47886,#8481);
#6661=LINE('',#47892,#8482);
#6662=LINE('',#47901,#8483);
#6663=LINE('',#47902,#8484);
#6664=LINE('',#47905,#8485);
#6665=LINE('',#47907,#8486);
#6666=LINE('',#47913,#8487);
#6667=LINE('',#47922,#8488);
#6668=LINE('',#47923,#8489);
#6669=LINE('',#47926,#8490);
#6670=LINE('',#47928,#8491);
#6671=LINE('',#47934,#8492);
#6672=LINE('',#47943,#8493);
#6673=LINE('',#47944,#8494);
#6674=LINE('',#47947,#8495);
#6675=LINE('',#47949,#8496);
#6676=LINE('',#47955,#8497);
#6677=LINE('',#47964,#8498);
#6678=LINE('',#47965,#8499);
#6679=LINE('',#47968,#8500);
#6680=LINE('',#47970,#8501);
#6681=LINE('',#47976,#8502);
#6682=LINE('',#47985,#8503);
#6683=LINE('',#47986,#8504);
#6684=LINE('',#47989,#8505);
#6685=LINE('',#47991,#8506);
#6686=LINE('',#47997,#8507);
#6687=LINE('',#48006,#8508);
#6688=LINE('',#48007,#8509);
#6689=LINE('',#48010,#8510);
#6690=LINE('',#48012,#8511);
#6691=LINE('',#48018,#8512);
#6692=LINE('',#48027,#8513);
#6693=LINE('',#48028,#8514);
#6694=LINE('',#48031,#8515);
#6695=LINE('',#48033,#8516);
#6696=LINE('',#48039,#8517);
#6697=LINE('',#48048,#8518);
#6698=LINE('',#48049,#8519);
#6699=LINE('',#48052,#8520);
#6700=LINE('',#48054,#8521);
#6701=LINE('',#48060,#8522);
#6702=LINE('',#48069,#8523);
#6703=LINE('',#48070,#8524);
#6704=LINE('',#48073,#8525);
#6705=LINE('',#48075,#8526);
#6706=LINE('',#48081,#8527);
#6707=LINE('',#48090,#8528);
#6708=LINE('',#48091,#8529);
#6709=LINE('',#48094,#8530);
#6710=LINE('',#48096,#8531);
#6711=LINE('',#48102,#8532);
#6712=LINE('',#48111,#8533);
#6713=LINE('',#48112,#8534);
#6714=LINE('',#48115,#8535);
#6715=LINE('',#48117,#8536);
#6716=LINE('',#48123,#8537);
#6717=LINE('',#48132,#8538);
#6718=LINE('',#48133,#8539);
#6719=LINE('',#48136,#8540);
#6720=LINE('',#48138,#8541);
#6721=LINE('',#48144,#8542);
#6722=LINE('',#48153,#8543);
#6723=LINE('',#48154,#8544);
#6724=LINE('',#48157,#8545);
#6725=LINE('',#48159,#8546);
#6726=LINE('',#48165,#8547);
#6727=LINE('',#48174,#8548);
#6728=LINE('',#48176,#8549);
#6729=LINE('',#48180,#8550);
#6730=LINE('',#48182,#8551);
#6731=LINE('',#48188,#8552);
#6732=LINE('',#48197,#8553);
#6733=LINE('',#48198,#8554);
#6734=LINE('',#48201,#8555);
#6735=LINE('',#48203,#8556);
#6736=LINE('',#48209,#8557);
#6737=LINE('',#48218,#8558);
#6738=LINE('',#48219,#8559);
#6739=LINE('',#48222,#8560);
#6740=LINE('',#48224,#8561);
#6741=LINE('',#48230,#8562);
#6742=LINE('',#48239,#8563);
#6743=LINE('',#48240,#8564);
#6744=LINE('',#48243,#8565);
#6745=LINE('',#48245,#8566);
#6746=LINE('',#48251,#8567);
#6747=LINE('',#48260,#8568);
#6748=LINE('',#48261,#8569);
#6749=LINE('',#48264,#8570);
#6750=LINE('',#48266,#8571);
#6751=LINE('',#48272,#8572);
#6752=LINE('',#48281,#8573);
#6753=LINE('',#48282,#8574);
#6754=LINE('',#48285,#8575);
#6755=LINE('',#48287,#8576);
#6756=LINE('',#48293,#8577);
#6757=LINE('',#48302,#8578);
#6758=LINE('',#48303,#8579);
#6759=LINE('',#48306,#8580);
#6760=LINE('',#48308,#8581);
#6761=LINE('',#48314,#8582);
#6762=LINE('',#48323,#8583);
#6763=LINE('',#48324,#8584);
#6764=LINE('',#48327,#8585);
#6765=LINE('',#48329,#8586);
#6766=LINE('',#48335,#8587);
#6767=LINE('',#48344,#8588);
#6768=LINE('',#48345,#8589);
#6769=LINE('',#48348,#8590);
#6770=LINE('',#48350,#8591);
#6771=LINE('',#48356,#8592);
#6772=LINE('',#48365,#8593);
#6773=LINE('',#48366,#8594);
#6774=LINE('',#48369,#8595);
#6775=LINE('',#48371,#8596);
#6776=LINE('',#48377,#8597);
#6777=LINE('',#48386,#8598);
#6778=LINE('',#48387,#8599);
#6779=LINE('',#48390,#8600);
#6780=LINE('',#48392,#8601);
#6781=LINE('',#48398,#8602);
#6782=LINE('',#48407,#8603);
#6783=LINE('',#48408,#8604);
#6784=LINE('',#48411,#8605);
#6785=LINE('',#48413,#8606);
#6786=LINE('',#48419,#8607);
#6787=LINE('',#48428,#8608);
#6788=LINE('',#48429,#8609);
#6789=LINE('',#48432,#8610);
#6790=LINE('',#48434,#8611);
#6791=LINE('',#48440,#8612);
#6792=LINE('',#48449,#8613);
#6793=LINE('',#48450,#8614);
#6794=LINE('',#48453,#8615);
#6795=LINE('',#48455,#8616);
#6796=LINE('',#48461,#8617);
#6797=LINE('',#48470,#8618);
#6798=LINE('',#48471,#8619);
#6799=LINE('',#48474,#8620);
#6800=LINE('',#48476,#8621);
#6801=LINE('',#48482,#8622);
#6802=LINE('',#48491,#8623);
#6803=LINE('',#48492,#8624);
#6804=LINE('',#48495,#8625);
#6805=LINE('',#48497,#8626);
#6806=LINE('',#48503,#8627);
#6807=LINE('',#48512,#8628);
#6808=LINE('',#48513,#8629);
#6809=LINE('',#48516,#8630);
#6810=LINE('',#48518,#8631);
#6811=LINE('',#48524,#8632);
#6812=LINE('',#48533,#8633);
#6813=LINE('',#48534,#8634);
#6814=LINE('',#48537,#8635);
#6815=LINE('',#48539,#8636);
#6816=LINE('',#48545,#8637);
#6817=LINE('',#48568,#8638);
#6818=LINE('',#48590,#8639);
#6819=LINE('',#48594,#8640);
#6820=LINE('',#48598,#8641);
#6821=LINE('',#48600,#8642);
#6822=LINE('',#48608,#8643);
#6823=LINE('',#48613,#8644);
#6824=LINE('',#48617,#8645);
#6825=LINE('',#48622,#8646);
#6826=LINE('',#48624,#8647);
#6827=LINE('',#48626,#8648);
#6828=LINE('',#48627,#8649);
#6829=LINE('',#48630,#8650);
#6830=LINE('',#48632,#8651);
#6831=LINE('',#48633,#8652);
#6832=LINE('',#48636,#8653);
#6833=LINE('',#48638,#8654);
#6834=LINE('',#48639,#8655);
#6835=LINE('',#48642,#8656);
#6836=LINE('',#48644,#8657);
#6837=LINE('',#48645,#8658);
#6838=LINE('',#48648,#8659);
#6839=LINE('',#48650,#8660);
#6840=LINE('',#48651,#8661);
#6841=LINE('',#48653,#8662);
#6842=LINE('',#48654,#8663);
#6843=LINE('',#48660,#8664);
#6844=LINE('',#48666,#8665);
#6845=LINE('',#48673,#8666);
#6846=LINE('',#48694,#8667);
#6847=LINE('',#48714,#8668);
#6848=LINE('',#48762,#8669);
#6849=LINE('',#48810,#8670);
#6850=LINE('',#48864,#8671);
#6851=LINE('',#48912,#8672);
#6852=LINE('',#48966,#8673);
#6853=LINE('',#49014,#8674);
#6854=LINE('',#49062,#8675);
#6855=LINE('',#49116,#8676);
#6856=LINE('',#49164,#8677);
#6857=LINE('',#49212,#8678);
#6858=LINE('',#49266,#8679);
#6859=LINE('',#49289,#8680);
#6860=LINE('',#49314,#8681);
#6861=LINE('',#49338,#8682);
#6862=LINE('',#49363,#8683);
#6863=LINE('',#49388,#8684);
#6864=LINE('',#49412,#8685);
#6865=LINE('',#49437,#8686);
#6866=LINE('',#49462,#8687);
#6867=LINE('',#49487,#8688);
#6868=LINE('',#49512,#8689);
#6869=LINE('',#49536,#8690);
#6870=LINE('',#50428,#8691);
#6871=LINE('',#50429,#8692);
#6872=LINE('',#50432,#8693);
#6873=LINE('',#50434,#8694);
#6874=LINE('',#50440,#8695);
#6875=LINE('',#50449,#8696);
#6876=LINE('',#50450,#8697);
#6877=LINE('',#50453,#8698);
#6878=LINE('',#50455,#8699);
#6879=LINE('',#50461,#8700);
#6880=LINE('',#50470,#8701);
#6881=LINE('',#50471,#8702);
#6882=LINE('',#50474,#8703);
#6883=LINE('',#50476,#8704);
#6884=LINE('',#50482,#8705);
#6885=LINE('',#50491,#8706);
#6886=LINE('',#50492,#8707);
#6887=LINE('',#50495,#8708);
#6888=LINE('',#50497,#8709);
#6889=LINE('',#50503,#8710);
#6890=LINE('',#50512,#8711);
#6891=LINE('',#50513,#8712);
#6892=LINE('',#50516,#8713);
#6893=LINE('',#50518,#8714);
#6894=LINE('',#50524,#8715);
#6895=LINE('',#50533,#8716);
#6896=LINE('',#50534,#8717);
#6897=LINE('',#50537,#8718);
#6898=LINE('',#50539,#8719);
#6899=LINE('',#50545,#8720);
#6900=LINE('',#50554,#8721);
#6901=LINE('',#50555,#8722);
#6902=LINE('',#50558,#8723);
#6903=LINE('',#50560,#8724);
#6904=LINE('',#50566,#8725);
#6905=LINE('',#50575,#8726);
#6906=LINE('',#50576,#8727);
#6907=LINE('',#50579,#8728);
#6908=LINE('',#50581,#8729);
#6909=LINE('',#50587,#8730);
#6910=LINE('',#50596,#8731);
#6911=LINE('',#50597,#8732);
#6912=LINE('',#50600,#8733);
#6913=LINE('',#50602,#8734);
#6914=LINE('',#50608,#8735);
#6915=LINE('',#50617,#8736);
#6916=LINE('',#50618,#8737);
#6917=LINE('',#50621,#8738);
#6918=LINE('',#50623,#8739);
#6919=LINE('',#50629,#8740);
#6920=LINE('',#50638,#8741);
#6921=LINE('',#50639,#8742);
#6922=LINE('',#50642,#8743);
#6923=LINE('',#50644,#8744);
#6924=LINE('',#50650,#8745);
#6925=LINE('',#50659,#8746);
#6926=LINE('',#50660,#8747);
#6927=LINE('',#50663,#8748);
#6928=LINE('',#50665,#8749);
#6929=LINE('',#50671,#8750);
#6930=LINE('',#50680,#8751);
#6931=LINE('',#50681,#8752);
#6932=LINE('',#50684,#8753);
#6933=LINE('',#50686,#8754);
#6934=LINE('',#50692,#8755);
#6935=LINE('',#50701,#8756);
#6936=LINE('',#50702,#8757);
#6937=LINE('',#50705,#8758);
#6938=LINE('',#50707,#8759);
#6939=LINE('',#50713,#8760);
#6940=LINE('',#50722,#8761);
#6941=LINE('',#50723,#8762);
#6942=LINE('',#50726,#8763);
#6943=LINE('',#50728,#8764);
#6944=LINE('',#50734,#8765);
#6945=LINE('',#50743,#8766);
#6946=LINE('',#50744,#8767);
#6947=LINE('',#50747,#8768);
#6948=LINE('',#50749,#8769);
#6949=LINE('',#50755,#8770);
#6950=LINE('',#50764,#8771);
#6951=LINE('',#50765,#8772);
#6952=LINE('',#50768,#8773);
#6953=LINE('',#50770,#8774);
#6954=LINE('',#50776,#8775);
#6955=LINE('',#50785,#8776);
#6956=LINE('',#50787,#8777);
#6957=LINE('',#50791,#8778);
#6958=LINE('',#50793,#8779);
#6959=LINE('',#50799,#8780);
#6960=LINE('',#50808,#8781);
#6961=LINE('',#50809,#8782);
#6962=LINE('',#50812,#8783);
#6963=LINE('',#50814,#8784);
#6964=LINE('',#50820,#8785);
#6965=LINE('',#50829,#8786);
#6966=LINE('',#50830,#8787);
#6967=LINE('',#50833,#8788);
#6968=LINE('',#50835,#8789);
#6969=LINE('',#50841,#8790);
#6970=LINE('',#50850,#8791);
#6971=LINE('',#50851,#8792);
#6972=LINE('',#50854,#8793);
#6973=LINE('',#50856,#8794);
#6974=LINE('',#50862,#8795);
#6975=LINE('',#50871,#8796);
#6976=LINE('',#50872,#8797);
#6977=LINE('',#50875,#8798);
#6978=LINE('',#50877,#8799);
#6979=LINE('',#50883,#8800);
#6980=LINE('',#50892,#8801);
#6981=LINE('',#50893,#8802);
#6982=LINE('',#50896,#8803);
#6983=LINE('',#50898,#8804);
#6984=LINE('',#50904,#8805);
#6985=LINE('',#50913,#8806);
#6986=LINE('',#50914,#8807);
#6987=LINE('',#50917,#8808);
#6988=LINE('',#50919,#8809);
#6989=LINE('',#50925,#8810);
#6990=LINE('',#50934,#8811);
#6991=LINE('',#50935,#8812);
#6992=LINE('',#50938,#8813);
#6993=LINE('',#50940,#8814);
#6994=LINE('',#50946,#8815);
#6995=LINE('',#50955,#8816);
#6996=LINE('',#50956,#8817);
#6997=LINE('',#50959,#8818);
#6998=LINE('',#50961,#8819);
#6999=LINE('',#50967,#8820);
#7000=LINE('',#50976,#8821);
#7001=LINE('',#50977,#8822);
#7002=LINE('',#50980,#8823);
#7003=LINE('',#50982,#8824);
#7004=LINE('',#50988,#8825);
#7005=LINE('',#50997,#8826);
#7006=LINE('',#50998,#8827);
#7007=LINE('',#51001,#8828);
#7008=LINE('',#51003,#8829);
#7009=LINE('',#51009,#8830);
#7010=LINE('',#51018,#8831);
#7011=LINE('',#51019,#8832);
#7012=LINE('',#51022,#8833);
#7013=LINE('',#51024,#8834);
#7014=LINE('',#51030,#8835);
#7015=LINE('',#51039,#8836);
#7016=LINE('',#51040,#8837);
#7017=LINE('',#51043,#8838);
#7018=LINE('',#51045,#8839);
#7019=LINE('',#51051,#8840);
#7020=LINE('',#51060,#8841);
#7021=LINE('',#51061,#8842);
#7022=LINE('',#51064,#8843);
#7023=LINE('',#51066,#8844);
#7024=LINE('',#51072,#8845);
#7025=LINE('',#51081,#8846);
#7026=LINE('',#51082,#8847);
#7027=LINE('',#51085,#8848);
#7028=LINE('',#51087,#8849);
#7029=LINE('',#51093,#8850);
#7030=LINE('',#51102,#8851);
#7031=LINE('',#51103,#8852);
#7032=LINE('',#51106,#8853);
#7033=LINE('',#51108,#8854);
#7034=LINE('',#51114,#8855);
#7035=LINE('',#51123,#8856);
#7036=LINE('',#51124,#8857);
#7037=LINE('',#51127,#8858);
#7038=LINE('',#51129,#8859);
#7039=LINE('',#51135,#8860);
#7040=LINE('',#51144,#8861);
#7041=LINE('',#51145,#8862);
#7042=LINE('',#51148,#8863);
#7043=LINE('',#51150,#8864);
#7044=LINE('',#51156,#8865);
#7045=LINE('',#51179,#8866);
#7046=LINE('',#51201,#8867);
#7047=LINE('',#51205,#8868);
#7048=LINE('',#51209,#8869);
#7049=LINE('',#51211,#8870);
#7050=LINE('',#51219,#8871);
#7051=LINE('',#51224,#8872);
#7052=LINE('',#51228,#8873);
#7053=LINE('',#51233,#8874);
#7054=LINE('',#51235,#8875);
#7055=LINE('',#51237,#8876);
#7056=LINE('',#51238,#8877);
#7057=LINE('',#51241,#8878);
#7058=LINE('',#51243,#8879);
#7059=LINE('',#51244,#8880);
#7060=LINE('',#51247,#8881);
#7061=LINE('',#51249,#8882);
#7062=LINE('',#51250,#8883);
#7063=LINE('',#51253,#8884);
#7064=LINE('',#51255,#8885);
#7065=LINE('',#51256,#8886);
#7066=LINE('',#51259,#8887);
#7067=LINE('',#51261,#8888);
#7068=LINE('',#51262,#8889);
#7069=LINE('',#51264,#8890);
#7070=LINE('',#51265,#8891);
#7071=LINE('',#51271,#8892);
#7072=LINE('',#51275,#8893);
#7073=LINE('',#51282,#8894);
#7074=LINE('',#51303,#8895);
#7075=LINE('',#51323,#8896);
#7076=LINE('',#51371,#8897);
#7077=LINE('',#51419,#8898);
#7078=LINE('',#51473,#8899);
#7079=LINE('',#51521,#8900);
#7080=LINE('',#51569,#8901);
#7081=LINE('',#51623,#8902);
#7082=LINE('',#51641,#8903);
#7083=LINE('',#51666,#8904);
#7084=LINE('',#51691,#8905);
#7085=LINE('',#51715,#8906);
#7086=LINE('',#51740,#8907);
#7087=LINE('',#51765,#8908);
#7088=LINE('',#51789,#8909);
#7089=LINE('',#52461,#8910);
#7090=LINE('',#52463,#8911);
#7091=LINE('',#52465,#8912);
#7092=LINE('',#52466,#8913);
#7093=LINE('',#52470,#8914);
#7094=LINE('',#52472,#8915);
#7095=LINE('',#52474,#8916);
#7096=LINE('',#52475,#8917);
#7097=LINE('',#52479,#8918);
#7098=LINE('',#52481,#8919);
#7099=LINE('',#52483,#8920);
#7100=LINE('',#52484,#8921);
#7101=LINE('',#52487,#8922);
#7102=LINE('',#52489,#8923);
#7103=LINE('',#52490,#8924);
#7104=LINE('',#52492,#8925);
#7105=LINE('',#52493,#8926);
#7106=LINE('',#52496,#8927);
#7107=LINE('',#52498,#8928);
#7108=LINE('',#52499,#8929);
#7109=LINE('',#52504,#8930);
#7110=LINE('',#52506,#8931);
#7111=LINE('',#52507,#8932);
#7112=LINE('',#52509,#8933);
#7113=LINE('',#52511,#8934);
#7114=LINE('',#52512,#8935);
#7115=LINE('',#52515,#8936);
#7116=LINE('',#52516,#8937);
#7117=LINE('',#52519,#8938);
#7118=LINE('',#52520,#8939);
#7119=LINE('',#52523,#8940);
#7120=LINE('',#52524,#8941);
#7121=LINE('',#52527,#8942);
#7122=LINE('',#52528,#8943);
#7123=LINE('',#52530,#8944);
#7124=LINE('',#52532,#8945);
#7125=LINE('',#52538,#8946);
#7126=LINE('',#52547,#8947);
#7127=LINE('',#52549,#8948);
#7128=LINE('',#52554,#8949);
#7129=LINE('',#52575,#8950);
#7130=LINE('',#52595,#8951);
#7131=LINE('',#52643,#8952);
#7132=LINE('',#52691,#8953);
#7133=LINE('',#52745,#8954);
#7134=LINE('',#52793,#8955);
#7135=LINE('',#52841,#8956);
#7136=LINE('',#52895,#8957);
#7137=LINE('',#52943,#8958);
#7138=LINE('',#52991,#8959);
#7139=LINE('',#53039,#8960);
#7140=LINE('',#53093,#8961);
#7141=LINE('',#53141,#8962);
#7142=LINE('',#53189,#8963);
#7143=LINE('',#53243,#8964);
#7144=LINE('',#53291,#8965);
#7145=LINE('',#53339,#8966);
#7146=LINE('',#53349,#8967);
#7147=LINE('',#53374,#8968);
#7148=LINE('',#53398,#8969);
#7149=LINE('',#53423,#8970);
#7150=LINE('',#53448,#8971);
#7151=LINE('',#53472,#8972);
#7152=LINE('',#53497,#8973);
#7153=LINE('',#53522,#8974);
#7154=LINE('',#53546,#8975);
#7155=LINE('',#53570,#8976);
#7156=LINE('',#53595,#8977);
#7157=LINE('',#53620,#8978);
#7158=LINE('',#53644,#8979);
#7159=LINE('',#53669,#8980);
#7160=LINE('',#53694,#8981);
#7161=LINE('',#53718,#8982);
#7162=LINE('',#54818,#8983);
#7163=LINE('',#54820,#8984);
#7164=LINE('',#54822,#8985);
#7165=LINE('',#54823,#8986);
#7166=LINE('',#54827,#8987);
#7167=LINE('',#54829,#8988);
#7168=LINE('',#54831,#8989);
#7169=LINE('',#54832,#8990);
#7170=LINE('',#54836,#8991);
#7171=LINE('',#54838,#8992);
#7172=LINE('',#54840,#8993);
#7173=LINE('',#54841,#8994);
#7174=LINE('',#54844,#8995);
#7175=LINE('',#54846,#8996);
#7176=LINE('',#54847,#8997);
#7177=LINE('',#54849,#8998);
#7178=LINE('',#54850,#8999);
#7179=LINE('',#54853,#9000);
#7180=LINE('',#54855,#9001);
#7181=LINE('',#54856,#9002);
#7182=LINE('',#54861,#9003);
#7183=LINE('',#54863,#9004);
#7184=LINE('',#54864,#9005);
#7185=LINE('',#54866,#9006);
#7186=LINE('',#54868,#9007);
#7187=LINE('',#54869,#9008);
#7188=LINE('',#54872,#9009);
#7189=LINE('',#54873,#9010);
#7190=LINE('',#54876,#9011);
#7191=LINE('',#54877,#9012);
#7192=LINE('',#54880,#9013);
#7193=LINE('',#54881,#9014);
#7194=LINE('',#54884,#9015);
#7195=LINE('',#54885,#9016);
#7196=LINE('',#54887,#9017);
#7197=LINE('',#54889,#9018);
#7198=LINE('',#54895,#9019);
#7199=LINE('',#54902,#9020);
#7200=LINE('',#54904,#9021);
#7201=VECTOR('',#27204,4.7393933982822);
#7202=VECTOR('',#27211,4.71);
#7203=VECTOR('',#27218,4.75);
#7204=VECTOR('',#27223,4.6656066017178);
#7205=VECTOR('',#27228,4.71);
#7206=VECTOR('',#27249,4.6656066017178);
#7207=VECTOR('',#27272,0.754393398282202);
#7208=VECTOR('',#27275,0.725);
#7209=VECTOR('',#27280,0.710606601717798);
#7210=VECTOR('',#27291,0.7);
#7211=VECTOR('',#27296,0.710606601717798);
#7212=VECTOR('',#27299,0.725);
#7213=VECTOR('',#27304,0.754393398282202);
#7214=VECTOR('',#27319,0.225);
#7215=VECTOR('',#27328,0.21);
#7216=VECTOR('',#27331,0.225);
#7217=VECTOR('',#27340,0.21);
#7218=VECTOR('',#27343,0.225);
#7219=VECTOR('',#27352,0.21);
#7220=VECTOR('',#27355,0.225);
#7221=VECTOR('',#27364,0.21);
#7222=VECTOR('',#27367,0.225);
#7223=VECTOR('',#27376,0.21);
#7224=VECTOR('',#27379,0.225);
#7225=VECTOR('',#27388,0.21);
#7226=VECTOR('',#27391,4.7393933982822);
#7227=VECTOR('',#27398,4.75);
#7228=VECTOR('',#27403,4.735);
#7229=VECTOR('',#27412,4.735);
#7230=VECTOR('',#27421,4.66);
#7231=VECTOR('',#27424,0.0649999999999999);
#7232=VECTOR('',#27429,0.13);
#7233=VECTOR('',#27434,0.18);
#7234=VECTOR('',#27437,0.0649999999999999);
#7235=VECTOR('',#27442,0.13);
#7236=VECTOR('',#27447,0.18);
#7237=VECTOR('',#27450,0.065);
#7238=VECTOR('',#27455,0.13);
#7239=VECTOR('',#27460,0.18);
#7240=VECTOR('',#27463,0.1325);
#7241=VECTOR('',#27468,0.12);
#7242=VECTOR('',#27473,0.1325);
#7243=VECTOR('',#27480,0.1325);
#7244=VECTOR('',#27485,0.12);
#7245=VECTOR('',#27490,0.1325);
#7246=VECTOR('',#27497,0.1325);
#7247=VECTOR('',#27502,0.12);
#7248=VECTOR('',#27507,0.1325);
#7249=VECTOR('',#27514,0.132499999999999);
#7250=VECTOR('',#27519,0.12);
#7251=VECTOR('',#27524,0.132499999999999);
#7252=VECTOR('',#27531,0.1325);
#7253=VECTOR('',#27536,0.12);
#7254=VECTOR('',#27541,0.1325);
#7255=VECTOR('',#27548,0.1325);
#7256=VECTOR('',#27553,0.12);
#7257=VECTOR('',#27558,0.1325);
#7258=VECTOR('',#27565,4.075);
#7259=VECTOR('',#27572,4.095);
#7260=VECTOR('',#27577,0.0524999999999998);
#7261=VECTOR('',#27582,0.105);
#7262=VECTOR('',#27587,0.155);
#7263=VECTOR('',#27592,0.0525000000000002);
#7264=VECTOR('',#27597,0.105);
#7265=VECTOR('',#27602,0.155);
#7266=VECTOR('',#27607,0.0525000000000002);
#7267=VECTOR('',#27612,0.105);
#7268=VECTOR('',#27617,0.154999999999999);
#7269=VECTOR('',#27622,0.0525000000000002);
#7270=VECTOR('',#27627,0.105);
#7271=VECTOR('',#27632,0.155);
#7272=VECTOR('',#27637,0.0524999999999998);
#7273=VECTOR('',#27642,0.105);
#7274=VECTOR('',#27647,0.155);
#7275=VECTOR('',#27652,0.0525000000000002);
#7276=VECTOR('',#27657,0.105);
#7277=VECTOR('',#27662,0.154999999999999);
#7278=VECTOR('',#27667,0.0525000000000002);
#7279=VECTOR('',#27672,0.105);
#7280=VECTOR('',#27677,0.154999999999999);
#7281=VECTOR('',#27682,0.0524999999999998);
#7282=VECTOR('',#27687,0.105);
#7283=VECTOR('',#27692,0.155);
#7284=VECTOR('',#27697,0.0525);
#7285=VECTOR('',#27702,0.105);
#7286=VECTOR('',#27707,0.155);
#7287=VECTOR('',#27712,0.0525);
#7288=VECTOR('',#27717,0.105);
#7289=VECTOR('',#27722,0.155);
#7290=VECTOR('',#27727,0.0525000000000002);
#7291=VECTOR('',#27732,0.105);
#7292=VECTOR('',#27737,0.155);
#7293=VECTOR('',#27742,0.0525000000000002);
#7294=VECTOR('',#27747,0.105);
#7295=VECTOR('',#27752,0.155);
#7296=VECTOR('',#27757,0.0524999999999993);
#7297=VECTOR('',#27762,0.105);
#7298=VECTOR('',#27767,0.155);
#7299=VECTOR('',#27772,0.0525000000000002);
#7300=VECTOR('',#27777,0.105);
#7301=VECTOR('',#27782,0.155);
#7302=VECTOR('',#27787,0.0525);
#7303=VECTOR('',#27792,0.105);
#7304=VECTOR('',#27797,0.155);
#7305=VECTOR('',#27802,0.0525);
#7306=VECTOR('',#27807,0.105);
#7307=VECTOR('',#27812,0.155);
#7308=VECTOR('',#27817,0.0524999999999998);
#7309=VECTOR('',#27822,0.105);
#7310=VECTOR('',#27827,0.155);
#7311=VECTOR('',#27832,0.0525000000000002);
#7312=VECTOR('',#27837,0.105);
#7313=VECTOR('',#27842,0.154999999999999);
#7314=VECTOR('',#27849,4.115);
#7315=VECTOR('',#27860,4.1);
#7316=VECTOR('',#27867,4.115);
#7317=VECTOR('',#27876,4.58);
#7318=VECTOR('',#27883,4.6);
#7319=VECTOR('',#27890,4.58);
#7320=VECTOR('',#27895,0.0525);
#7321=VECTOR('',#27900,0.105);
#7322=VECTOR('',#27905,0.155);
#7323=VECTOR('',#27910,0.0525);
#7324=VECTOR('',#27915,0.105);
#7325=VECTOR('',#27920,0.155);
#7326=VECTOR('',#27925,0.0650000000000004);
#7327=VECTOR('',#27930,0.13);
#7328=VECTOR('',#27935,0.180000000000001);
#7329=VECTOR('',#27940,0.0649999999999999);
#7330=VECTOR('',#27945,0.13);
#7331=VECTOR('',#27950,0.18);
#7332=VECTOR('',#27955,0.065);
#7333=VECTOR('',#27960,0.13);
#7334=VECTOR('',#27965,0.18);
#7335=VECTOR('',#27972,0.1325);
#7336=VECTOR('',#27977,0.12);
#7337=VECTOR('',#27982,0.1325);
#7338=VECTOR('',#27991,0.21);
#7339=VECTOR('',#27998,0.1325);
#7340=VECTOR('',#28003,0.12);
#7341=VECTOR('',#28008,0.1325);
#7342=VECTOR('',#28017,0.21);
#7343=VECTOR('',#28024,0.1325);
#7344=VECTOR('',#28029,0.12);
#7345=VECTOR('',#28034,0.1325);
#7346=VECTOR('',#28043,0.21);
#7347=VECTOR('',#28050,0.1325);
#7348=VECTOR('',#28055,0.12);
#7349=VECTOR('',#28060,0.1325);
#7350=VECTOR('',#28069,0.21);
#7351=VECTOR('',#28076,0.1325);
#7352=VECTOR('',#28081,0.12);
#7353=VECTOR('',#28086,0.1325);
#7354=VECTOR('',#28095,0.21);
#7355=VECTOR('',#28102,0.1325);
#7356=VECTOR('',#28107,0.120000000000001);
#7357=VECTOR('',#28112,0.1325);
#7358=VECTOR('',#28121,0.21);
#7359=VECTOR('',#28128,0.1325);
#7360=VECTOR('',#28133,0.12);
#7361=VECTOR('',#28138,0.1325);
#7362=VECTOR('',#28147,0.21);
#7363=VECTOR('',#28154,0.132499999999999);
#7364=VECTOR('',#28159,0.12);
#7365=VECTOR('',#28164,0.132499999999999);
#7366=VECTOR('',#28173,0.21);
#7367=VECTOR('',#28180,0.1325);
#7368=VECTOR('',#28185,0.12);
#7369=VECTOR('',#28190,0.1325);
#7370=VECTOR('',#28199,0.21);
#7371=VECTOR('',#28206,0.1325);
#7372=VECTOR('',#28211,0.12);
#7373=VECTOR('',#28216,0.1325);
#7374=VECTOR('',#28225,0.21);
#7375=VECTOR('',#28232,0.1325);
#7376=VECTOR('',#28237,0.12);
#7377=VECTOR('',#28242,0.1325);
#7378=VECTOR('',#28251,0.21);
#7379=VECTOR('',#28258,0.1325);
#7380=VECTOR('',#28263,0.12);
#7381=VECTOR('',#28268,0.1325);
#7382=VECTOR('',#28277,0.21);
#7383=VECTOR('',#28284,0.72);
#7384=VECTOR('',#28295,0.7);
#7385=VECTOR('',#28302,0.72);
#7386=VECTOR('',#28315,4.585);
#7387=VECTOR('',#28324,4.6);
#7388=VECTOR('',#28333,4.585);
#7389=VECTOR('',#28336,1.);
#7390=VECTOR('',#28339,1.);
#7391=VECTOR('',#28346,1.);
#7392=VECTOR('',#28349,1.);
#7393=VECTOR('',#28352,1.);
#7394=VECTOR('',#28355,1.);
#7395=VECTOR('',#28364,1.);
#7396=VECTOR('',#28367,1.);
#7397=VECTOR('',#28368,1.);
#7398=VECTOR('',#28371,1.);
#7399=VECTOR('',#28378,1.);
#7400=VECTOR('',#28381,1.);
#7401=VECTOR('',#28384,1.);
#7402=VECTOR('',#28387,1.);
#7403=VECTOR('',#28396,1.);
#7404=VECTOR('',#28399,1.);
#7405=VECTOR('',#28400,1.);
#7406=VECTOR('',#28403,1.);
#7407=VECTOR('',#28410,1.);
#7408=VECTOR('',#28413,1.);
#7409=VECTOR('',#28416,1.);
#7410=VECTOR('',#28419,1.);
#7411=VECTOR('',#28428,1.);
#7412=VECTOR('',#28431,1.);
#7413=VECTOR('',#28432,1.);
#7414=VECTOR('',#28435,1.);
#7415=VECTOR('',#28438,1.);
#7416=VECTOR('',#28441,1.);
#7417=VECTOR('',#28444,1.);
#7418=VECTOR('',#28447,1.);
#7419=VECTOR('',#28450,1.);
#7420=VECTOR('',#28453,1.);
#7421=VECTOR('',#28456,1.);
#7422=VECTOR('',#28459,1.);
#7423=VECTOR('',#28462,1.);
#7424=VECTOR('',#28465,1.);
#7425=VECTOR('',#28468,1.);
#7426=VECTOR('',#28471,1.);
#7427=VECTOR('',#28474,1.);
#7428=VECTOR('',#28477,1.);
#7429=VECTOR('',#28480,1.);
#7430=VECTOR('',#28483,1.);
#7431=VECTOR('',#28486,1.);
#7432=VECTOR('',#28489,1.);
#7433=VECTOR('',#28492,1.);
#7434=VECTOR('',#28495,1.);
#7435=VECTOR('',#28498,1.);
#7436=VECTOR('',#28501,1.);
#7437=VECTOR('',#28504,1.);
#7438=VECTOR('',#28507,1.);
#7439=VECTOR('',#28510,1.);
#7440=VECTOR('',#28513,1.);
#7441=VECTOR('',#28516,1.);
#7442=VECTOR('',#28519,1.);
#7443=VECTOR('',#28522,1.);
#7444=VECTOR('',#28525,1.);
#7445=VECTOR('',#28528,1.);
#7446=VECTOR('',#28531,1.);
#7447=VECTOR('',#28534,1.);
#7448=VECTOR('',#28537,1.);
#7449=VECTOR('',#28540,1.);
#7450=VECTOR('',#28543,1.);
#7451=VECTOR('',#28546,1.);
#7452=VECTOR('',#28549,1.);
#7453=VECTOR('',#28552,1.);
#7454=VECTOR('',#28555,1.);
#7455=VECTOR('',#28558,1.);
#7456=VECTOR('',#28561,1.);
#7457=VECTOR('',#28564,1.);
#7458=VECTOR('',#28567,1.);
#7459=VECTOR('',#28570,1.);
#7460=VECTOR('',#28573,1.);
#7461=VECTOR('',#28576,1.);
#7462=VECTOR('',#28579,1.);
#7463=VECTOR('',#28582,1.);
#7464=VECTOR('',#28585,1.);
#7465=VECTOR('',#28588,1.);
#7466=VECTOR('',#28591,1.);
#7467=VECTOR('',#28598,0.12);
#7468=VECTOR('',#28601,1.);
#7469=VECTOR('',#28606,1.);
#7470=VECTOR('',#28607,1.);
#7471=VECTOR('',#28610,1.);
#7472=VECTOR('',#28611,1.);
#7473=VECTOR('',#28616,0.12);
#7474=VECTOR('',#28617,1.);
#7475=VECTOR('',#28620,1.);
#7476=VECTOR('',#28627,1.);
#7477=VECTOR('',#28628,1.);
#7478=VECTOR('',#28631,1.);
#7479=VECTOR('',#28632,1.);
#7480=VECTOR('',#28637,1.);
#7481=VECTOR('',#28638,1.);
#7482=VECTOR('',#28641,1.);
#7483=VECTOR('',#28642,1.);
#7484=VECTOR('',#28647,1.);
#7485=VECTOR('',#28654,1.);
#7486=VECTOR('',#28655,1.);
#7487=VECTOR('',#28658,1.);
#7488=VECTOR('',#28659,1.);
#7489=VECTOR('',#28664,1.);
#7490=VECTOR('',#28665,1.);
#7491=VECTOR('',#28668,1.);
#7492=VECTOR('',#28669,1.);
#7493=VECTOR('',#28674,1.);
#7494=VECTOR('',#28679,0.12);
#7495=VECTOR('',#28682,1.);
#7496=VECTOR('',#28687,1.);
#7497=VECTOR('',#28688,1.);
#7498=VECTOR('',#28691,1.);
#7499=VECTOR('',#28692,1.);
#7500=VECTOR('',#28697,1.);
#7501=VECTOR('',#28698,1.);
#7502=VECTOR('',#28701,1.);
#7503=VECTOR('',#28702,1.);
#7504=VECTOR('',#28707,1.);
#7505=VECTOR('',#28714,1.);
#7506=VECTOR('',#28715,1.);
#7507=VECTOR('',#28718,1.);
#7508=VECTOR('',#28719,1.);
#7509=VECTOR('',#28724,1.);
#7510=VECTOR('',#28725,1.);
#7511=VECTOR('',#28728,1.);
#7512=VECTOR('',#28729,1.);
#7513=VECTOR('',#28734,1.);
#7514=VECTOR('',#28741,1.);
#7515=VECTOR('',#28742,1.);
#7516=VECTOR('',#28745,1.);
#7517=VECTOR('',#28746,1.);
#7518=VECTOR('',#28751,1.);
#7519=VECTOR('',#28752,1.);
#7520=VECTOR('',#28755,1.);
#7521=VECTOR('',#28760,1.);
#7522=VECTOR('',#28763,0.12);
#7523=VECTOR('',#28766,1.);
#7524=VECTOR('',#28771,1.);
#7525=VECTOR('',#28772,1.);
#7526=VECTOR('',#28775,1.);
#7527=VECTOR('',#28776,1.);
#7528=VECTOR('',#28781,1.);
#7529=VECTOR('',#28782,1.);
#7530=VECTOR('',#28785,1.);
#7531=VECTOR('',#28786,1.);
#7532=VECTOR('',#28791,1.);
#7533=VECTOR('',#28798,1.);
#7534=VECTOR('',#28799,1.);
#7535=VECTOR('',#28802,1.);
#7536=VECTOR('',#28803,1.);
#7537=VECTOR('',#28808,1.);
#7538=VECTOR('',#28809,1.);
#7539=VECTOR('',#28812,1.);
#7540=VECTOR('',#28813,1.);
#7541=VECTOR('',#28818,1.);
#7542=VECTOR('',#28823,0.12);
#7543=VECTOR('',#28826,1.);
#7544=VECTOR('',#28829,1.);
#7545=VECTOR('',#28832,1.);
#7546=VECTOR('',#28837,1.);
#7547=VECTOR('',#28840,1.);
#7548=VECTOR('',#28843,1.);
#7549=VECTOR('',#28848,1.);
#7550=VECTOR('',#28849,1.);
#7551=VECTOR('',#28852,1.);
#7552=VECTOR('',#28853,1.);
#7553=VECTOR('',#28858,1.);
#7554=VECTOR('',#28859,1.);
#7555=VECTOR('',#28862,1.);
#7556=VECTOR('',#28863,1.);
#7557=VECTOR('',#28868,1.);
#7558=VECTOR('',#28875,1.);
#7559=VECTOR('',#28876,1.);
#7560=VECTOR('',#28879,1.);
#7561=VECTOR('',#28880,1.);
#7562=VECTOR('',#28885,1.);
#7563=VECTOR('',#28886,1.);
#7564=VECTOR('',#28889,1.);
#7565=VECTOR('',#28890,1.);
#7566=VECTOR('',#28895,1.);
#7567=VECTOR('',#28902,1.);
#7568=VECTOR('',#28903,1.);
#7569=VECTOR('',#28906,1.);
#7570=VECTOR('',#28907,1.);
#7571=VECTOR('',#28912,1.);
#7572=VECTOR('',#28913,1.);
#7573=VECTOR('',#28916,1.);
#7574=VECTOR('',#28921,1.);
#7575=VECTOR('',#28924,0.12);
#7576=VECTOR('',#28927,1.);
#7577=VECTOR('',#28932,1.);
#7578=VECTOR('',#28933,1.);
#7579=VECTOR('',#28936,1.);
#7580=VECTOR('',#28937,1.);
#7581=VECTOR('',#28942,1.);
#7582=VECTOR('',#28943,1.);
#7583=VECTOR('',#28946,1.);
#7584=VECTOR('',#28947,1.);
#7585=VECTOR('',#28952,1.);
#7586=VECTOR('',#28959,1.);
#7587=VECTOR('',#28960,1.);
#7588=VECTOR('',#28963,1.);
#7589=VECTOR('',#28964,1.);
#7590=VECTOR('',#28969,1.);
#7591=VECTOR('',#28970,1.);
#7592=VECTOR('',#28973,1.);
#7593=VECTOR('',#28974,1.);
#7594=VECTOR('',#28979,1.);
#7595=VECTOR('',#28986,1.);
#7596=VECTOR('',#28987,1.);
#7597=VECTOR('',#28990,1.);
#7598=VECTOR('',#28991,1.);
#7599=VECTOR('',#28996,1.);
#7600=VECTOR('',#28997,1.);
#7601=VECTOR('',#29000,1.);
#7602=VECTOR('',#29001,1.);
#7603=VECTOR('',#29006,1.);
#7604=VECTOR('',#29011,0.12);
#7605=VECTOR('',#29014,1.);
#7606=VECTOR('',#29019,1.);
#7607=VECTOR('',#29020,1.);
#7608=VECTOR('',#29023,1.);
#7609=VECTOR('',#29024,1.);
#7610=VECTOR('',#29029,1.);
#7611=VECTOR('',#29030,1.);
#7612=VECTOR('',#29033,1.);
#7613=VECTOR('',#29034,1.);
#7614=VECTOR('',#29039,1.);
#7615=VECTOR('',#29046,1.);
#7616=VECTOR('',#29047,1.);
#7617=VECTOR('',#29050,1.);
#7618=VECTOR('',#29051,1.);
#7619=VECTOR('',#29056,1.);
#7620=VECTOR('',#29057,1.);
#7621=VECTOR('',#29060,1.);
#7622=VECTOR('',#29061,1.);
#7623=VECTOR('',#29066,1.);
#7624=VECTOR('',#29071,0.12);
#7625=VECTOR('',#29074,1.);
#7626=VECTOR('',#29077,1.);
#7627=VECTOR('',#29080,1.);
#7628=VECTOR('',#29085,1.);
#7629=VECTOR('',#29088,1.);
#7630=VECTOR('',#29091,1.);
#7631=VECTOR('',#29096,1.);
#7632=VECTOR('',#29097,1.);
#7633=VECTOR('',#29100,1.);
#7634=VECTOR('',#29101,1.);
#7635=VECTOR('',#29106,1.);
#7636=VECTOR('',#29107,1.);
#7637=VECTOR('',#29110,1.);
#7638=VECTOR('',#29111,1.);
#7639=VECTOR('',#29116,1.);
#7640=VECTOR('',#29123,1.);
#7641=VECTOR('',#29124,1.);
#7642=VECTOR('',#29127,1.);
#7643=VECTOR('',#29128,1.);
#7644=VECTOR('',#29133,1.);
#7645=VECTOR('',#29134,1.);
#7646=VECTOR('',#29137,1.);
#7647=VECTOR('',#29138,1.);
#7648=VECTOR('',#29143,1.);
#7649=VECTOR('',#29148,0.12);
#7650=VECTOR('',#29151,1.);
#7651=VECTOR('',#29156,1.);
#7652=VECTOR('',#29157,1.);
#7653=VECTOR('',#29160,1.);
#7654=VECTOR('',#29161,1.);
#7655=VECTOR('',#29166,1.);
#7656=VECTOR('',#29171,1.);
#7657=VECTOR('',#29172,1.);
#7658=VECTOR('',#29175,1.);
#7659=VECTOR('',#29176,1.);
#7660=VECTOR('',#29181,1.);
#7661=VECTOR('',#29182,1.);
#7662=VECTOR('',#29185,1.);
#7663=VECTOR('',#29186,1.);
#7664=VECTOR('',#29191,1.);
#7665=VECTOR('',#29198,1.);
#7666=VECTOR('',#29199,1.);
#7667=VECTOR('',#29202,1.);
#7668=VECTOR('',#29203,1.);
#7669=VECTOR('',#29208,1.);
#7670=VECTOR('',#29209,1.);
#7671=VECTOR('',#29212,1.);
#7672=VECTOR('',#29213,1.);
#7673=VECTOR('',#29218,1.);
#7674=VECTOR('',#29225,1.);
#7675=VECTOR('',#29226,1.);
#7676=VECTOR('',#29229,1.);
#7677=VECTOR('',#29230,1.);
#7678=VECTOR('',#29235,1.);
#7679=VECTOR('',#29236,1.);
#7680=VECTOR('',#29239,1.);
#7681=VECTOR('',#29240,1.);
#7682=VECTOR('',#29245,1.);
#7683=VECTOR('',#29252,1.);
#7684=VECTOR('',#29253,1.);
#7685=VECTOR('',#29256,1.);
#7686=VECTOR('',#29257,1.);
#7687=VECTOR('',#29262,1.);
#7688=VECTOR('',#29267,1.);
#7689=VECTOR('',#29268,1.);
#7690=VECTOR('',#29271,1.);
#7691=VECTOR('',#29272,1.);
#7692=VECTOR('',#29277,0.12);
#7693=VECTOR('',#29278,1.);
#7694=VECTOR('',#29281,1.);
#7695=VECTOR('',#29288,1.);
#7696=VECTOR('',#29289,1.);
#7697=VECTOR('',#29292,1.);
#7698=VECTOR('',#29293,1.);
#7699=VECTOR('',#29298,1.);
#7700=VECTOR('',#29303,0.12);
#7701=VECTOR('',#29304,1.);
#7702=VECTOR('',#29307,1.);
#7703=VECTOR('',#29314,1.);
#7704=VECTOR('',#29315,1.);
#7705=VECTOR('',#29318,1.);
#7706=VECTOR('',#29319,1.);
#7707=VECTOR('',#29324,1.);
#7708=VECTOR('',#29329,0.12);
#7709=VECTOR('',#29330,1.);
#7710=VECTOR('',#29333,1.);
#7711=VECTOR('',#29348,1.);
#7712=VECTOR('',#29357,1.);
#7713=VECTOR('',#29420,3.8);
#7714=VECTOR('',#29429,4.095);
#7715=VECTOR('',#29432,0.9025);
#7716=VECTOR('',#29439,1.035);
#7717=VECTOR('',#29446,1.05);
#7718=VECTOR('',#29457,1.035);
#7719=VECTOR('',#29468,0.6543933982822);
#7720=VECTOR('',#29475,0.625);
#7721=VECTOR('',#29482,0.610606601717797);
#7722=VECTOR('',#29489,0.6);
#7723=VECTOR('',#29498,0.610606601717798);
#7724=VECTOR('',#29503,0.625);
#7725=VECTOR('',#29506,0.654393398282201);
#7726=VECTOR('',#29519,0.88);
#7727=VECTOR('',#29522,0.9);
#7728=VECTOR('',#29531,1.2);
#7729=VECTOR('',#29542,1.05);
#7730=VECTOR('',#29547,0.9);
#7731=VECTOR('',#29554,1.08);
#7732=VECTOR('',#29571,1.065);
#7733=VECTOR('',#29576,1.4956066017178);
#7734=VECTOR('',#29581,1.525);
#7735=VECTOR('',#29584,1.5393933982822);
#7736=VECTOR('',#29595,1.55);
#7737=VECTOR('',#29600,1.5393933982822);
#7738=VECTOR('',#29605,1.525);
#7739=VECTOR('',#29610,0.925);
#7740=VECTOR('',#29621,0.91);
#7741=VECTOR('',#29626,1.4956066017178);
#7742=VECTOR('',#29637,0.225);
#7743=VECTOR('',#29648,0.21);
#7744=VECTOR('',#29653,0.225);
#7745=VECTOR('',#29664,0.21);
#7746=VECTOR('',#29667,0.1325);
#7747=VECTOR('',#29672,0.12);
#7748=VECTOR('',#29677,0.1325);
#7749=VECTOR('',#29684,0.1325);
#7750=VECTOR('',#29689,0.12);
#7751=VECTOR('',#29694,0.1325);
#7752=VECTOR('',#29701,0.93);
#7753=VECTOR('',#29712,0.45);
#7754=VECTOR('',#29719,0.45);
#7755=VECTOR('',#29726,0.13);
#7756=VECTOR('',#29731,0.18);
#7757=VECTOR('',#29738,0.145);
#7758=VECTOR('',#29745,0.145);
#7759=VECTOR('',#29752,0.145);
#7760=VECTOR('',#29759,0.0950000000000001);
#7761=VECTOR('',#29766,0.095);
#7762=VECTOR('',#29773,0.305);
#7763=VECTOR('',#29780,0.815);
#7764=VECTOR('',#29791,0.8);
#7765=VECTOR('',#29798,0.815);
#7766=VECTOR('',#29807,3.985);
#7767=VECTOR('',#29814,4.);
#7768=VECTOR('',#29821,3.985);
#7769=VECTOR('',#29826,0.0425);
#7770=VECTOR('',#29831,0.085);
#7771=VECTOR('',#29836,0.0425);
#7772=VECTOR('',#29841,0.085);
#7773=VECTOR('',#29848,0.14);
#7774=VECTOR('',#29861,0.52);
#7775=VECTOR('',#29866,0.54);
#7776=VECTOR('',#29871,0.78);
#7777=VECTOR('',#29886,0.8);
#7778=VECTOR('',#29895,0.78);
#7779=VECTOR('',#29898,0.8);
#7780=VECTOR('',#29903,0.78);
#7781=VECTOR('',#29912,0.3);
#7782=VECTOR('',#29921,0.1);
#7783=VECTOR('',#29926,0.09);
#7784=VECTOR('',#29935,0.185);
#7785=VECTOR('',#29946,0.2);
#7786=VECTOR('',#29955,0.115);
#7787=VECTOR('',#29958,0.1);
#7788=VECTOR('',#29961,1.);
#7789=VECTOR('',#29962,1.);
#7790=VECTOR('',#29969,0.115);
#7791=VECTOR('',#29974,1.);
#7792=VECTOR('',#29983,0.39);
#7793=VECTOR('',#29990,0.105);
#7794=VECTOR('',#29997,0.1);
#7795=VECTOR('',#30002,0.085);
#7796=VECTOR('',#30017,0.1);
#7797=VECTOR('',#30028,0.1);
#7798=VECTOR('',#30033,0.085);
#7799=VECTOR('',#30038,0.1);
#7800=VECTOR('',#30041,0.1);
#7801=VECTOR('',#30046,0.085);
#7802=VECTOR('',#30051,0.1);
#7803=VECTOR('',#30058,0.69);
#7804=VECTOR('',#30065,0.7);
#7805=VECTOR('',#30072,0.69);
#7806=VECTOR('',#30079,0.2175);
#7807=VECTOR('',#30090,0.2025);
#7808=VECTOR('',#30113,0.2175);
#7809=VECTOR('',#30132,0.685);
#7810=VECTOR('',#30139,0.7);
#7811=VECTOR('',#30142,0.105);
#7812=VECTOR('',#30147,0.09);
#7813=VECTOR('',#30152,0.105);
#7814=VECTOR('',#30155,0.105);
#7815=VECTOR('',#30160,0.09);
#7816=VECTOR('',#30165,0.105);
#7817=VECTOR('',#30168,0.105);
#7818=VECTOR('',#30173,0.09);
#7819=VECTOR('',#30178,0.105);
#7820=VECTOR('',#30181,0.69);
#7821=VECTOR('',#30186,1.);
#7822=VECTOR('',#30187,1.);
#7823=VECTOR('',#30188,1.);
#7824=VECTOR('',#30189,1.);
#7825=VECTOR('',#30192,1.);
#7826=VECTOR('',#30193,1.);
#7827=VECTOR('',#30194,1.);
#7828=VECTOR('',#30195,1.);
#7829=VECTOR('',#30198,1.);
#7830=VECTOR('',#30199,1.);
#7831=VECTOR('',#30210,1.);
#7832=VECTOR('',#30213,1.);
#7833=VECTOR('',#30216,1.);
#7834=VECTOR('',#30219,1.);
#7835=VECTOR('',#30222,1.);
#7836=VECTOR('',#30225,1.);
#7837=VECTOR('',#30228,1.);
#7838=VECTOR('',#30231,1.);
#7839=VECTOR('',#30234,1.);
#7840=VECTOR('',#30237,1.);
#7841=VECTOR('',#30240,1.);
#7842=VECTOR('',#30243,1.);
#7843=VECTOR('',#30256,0.09);
#7844=VECTOR('',#30261,0.09);
#7845=VECTOR('',#30266,0.0900000000000001);
#7846=VECTOR('',#30269,1.);
#7847=VECTOR('',#30270,1.);
#7848=VECTOR('',#30271,1.);
#7849=VECTOR('',#30274,1.);
#7850=VECTOR('',#30279,1.);
#7851=VECTOR('',#30280,1.);
#7852=VECTOR('',#30287,1.);
#7853=VECTOR('',#30288,1.);
#7854=VECTOR('',#30289,1.);
#7855=VECTOR('',#30292,1.);
#7856=VECTOR('',#30297,1.);
#7857=VECTOR('',#30298,1.);
#7858=VECTOR('',#30305,1.);
#7859=VECTOR('',#30306,1.);
#7860=VECTOR('',#30307,1.);
#7861=VECTOR('',#30310,1.);
#7862=VECTOR('',#30315,1.);
#7863=VECTOR('',#30316,1.);
#7864=VECTOR('',#30323,1.);
#7865=VECTOR('',#30324,1.);
#7866=VECTOR('',#30325,1.);
#7867=VECTOR('',#30328,1.);
#7868=VECTOR('',#30333,1.);
#7869=VECTOR('',#30334,1.);
#7870=VECTOR('',#30341,1.);
#7871=VECTOR('',#30342,1.);
#7872=VECTOR('',#30343,1.);
#7873=VECTOR('',#30346,1.);
#7874=VECTOR('',#30351,1.);
#7875=VECTOR('',#30352,1.);
#7876=VECTOR('',#30359,1.);
#7877=VECTOR('',#30360,1.);
#7878=VECTOR('',#30361,1.);
#7879=VECTOR('',#30364,1.);
#7880=VECTOR('',#30369,1.);
#7881=VECTOR('',#30370,1.);
#7882=VECTOR('',#30379,0.2025);
#7883=VECTOR('',#30386,1.);
#7884=VECTOR('',#30387,1.);
#7885=VECTOR('',#30388,1.);
#7886=VECTOR('',#30389,1.);
#7887=VECTOR('',#30392,1.);
#7888=VECTOR('',#30393,1.);
#7889=VECTOR('',#30394,1.);
#7890=VECTOR('',#30397,1.);
#7891=VECTOR('',#30398,1.);
#7892=VECTOR('',#30399,1.);
#7893=VECTOR('',#30400,1.);
#7894=VECTOR('',#30401,1.);
#7895=VECTOR('',#30402,1.);
#7896=VECTOR('',#30403,1.);
#7897=VECTOR('',#30404,1.);
#7898=VECTOR('',#30405,1.);
#7899=VECTOR('',#30406,1.);
#7900=VECTOR('',#30407,1.);
#7901=VECTOR('',#30408,1.);
#7902=VECTOR('',#30409,1.);
#7903=VECTOR('',#30410,1.);
#7904=VECTOR('',#30413,1.);
#7905=VECTOR('',#30414,1.);
#7906=VECTOR('',#30415,1.);
#7907=VECTOR('',#30418,1.);
#7908=VECTOR('',#30419,1.);
#7909=VECTOR('',#30422,1.);
#7910=VECTOR('',#30423,1.);
#7911=VECTOR('',#30424,1.);
#7912=VECTOR('',#30425,1.);
#7913=VECTOR('',#30426,1.);
#7914=VECTOR('',#30427,1.);
#7915=VECTOR('',#30428,1.);
#7916=VECTOR('',#30429,1.);
#7917=VECTOR('',#30430,1.);
#7918=VECTOR('',#30431,1.);
#7919=VECTOR('',#30432,1.);
#7920=VECTOR('',#30433,1.);
#7921=VECTOR('',#30436,1.);
#7922=VECTOR('',#30439,1.);
#7923=VECTOR('',#30440,1.);
#7924=VECTOR('',#30441,1.);
#7925=VECTOR('',#30442,1.);
#7926=VECTOR('',#30443,1.);
#7927=VECTOR('',#30446,1.);
#7928=VECTOR('',#30449,1.);
#7929=VECTOR('',#30452,1.);
#7930=VECTOR('',#30455,1.);
#7931=VECTOR('',#30456,1.);
#7932=VECTOR('',#30457,1.);
#7933=VECTOR('',#30458,1.);
#7934=VECTOR('',#30459,1.);
#7935=VECTOR('',#30464,1.);
#7936=VECTOR('',#30465,1.);
#7937=VECTOR('',#30468,1.);
#7938=VECTOR('',#30469,1.);
#7939=VECTOR('',#30470,1.);
#7940=VECTOR('',#30471,1.);
#7941=VECTOR('',#30476,1.);
#7942=VECTOR('',#30479,1.);
#7943=VECTOR('',#30486,0.0900000000000001);
#7944=VECTOR('',#30491,0.09);
#7945=VECTOR('',#30494,1.);
#7946=VECTOR('',#30495,1.);
#7947=VECTOR('',#30496,1.);
#7948=VECTOR('',#30499,1.);
#7949=VECTOR('',#30500,1.);
#7950=VECTOR('',#30501,1.);
#7951=VECTOR('',#30504,1.);
#7952=VECTOR('',#30505,1.);
#7953=VECTOR('',#30512,1.);
#7954=VECTOR('',#30513,1.);
#7955=VECTOR('',#30514,1.);
#7956=VECTOR('',#30517,1.);
#7957=VECTOR('',#30518,1.);
#7958=VECTOR('',#30521,1.);
#7959=VECTOR('',#30522,1.);
#7960=VECTOR('',#30525,1.);
#7961=VECTOR('',#30530,1.);
#7962=VECTOR('',#30531,1.);
#7963=VECTOR('',#30532,1.);
#7964=VECTOR('',#30535,1.);
#7965=VECTOR('',#30536,1.);
#7966=VECTOR('',#30539,1.);
#7967=VECTOR('',#30540,1.);
#7968=VECTOR('',#30543,1.);
#7969=VECTOR('',#30554,1.);
#7970=VECTOR('',#30557,1.);
#7971=VECTOR('',#30560,1.);
#7972=VECTOR('',#30563,1.);
#7973=VECTOR('',#30564,1.);
#7974=VECTOR('',#30567,1.);
#7975=VECTOR('',#30570,1.);
#7976=VECTOR('',#30573,1.);
#7977=VECTOR('',#30574,1.);
#7978=VECTOR('',#30577,1.);
#7979=VECTOR('',#30578,1.);
#7980=VECTOR('',#30583,1.);
#7981=VECTOR('',#30588,0.085);
#7982=VECTOR('',#30595,0.085);
#7983=VECTOR('',#30600,1.);
#7984=VECTOR('',#30601,1.);
#7985=VECTOR('',#30602,1.);
#7986=VECTOR('',#30605,1.);
#7987=VECTOR('',#30610,1.);
#7988=VECTOR('',#30611,1.);
#7989=VECTOR('',#30620,1.);
#7990=VECTOR('',#30627,1.);
#7991=VECTOR('',#30630,1.);
#7992=VECTOR('',#30631,1.);
#7993=VECTOR('',#30634,1.);
#7994=VECTOR('',#30635,1.);
#7995=VECTOR('',#30638,1.);
#7996=VECTOR('',#30639,1.);
#7997=VECTOR('',#30640,1.);
#7998=VECTOR('',#30641,1.);
#7999=VECTOR('',#30644,1.);
#8000=VECTOR('',#30645,1.);
#8001=VECTOR('',#30646,1.);
#8002=VECTOR('',#30647,1.);
#8003=VECTOR('',#30650,1.);
#8004=VECTOR('',#30651,1.);
#8005=VECTOR('',#30652,1.);
#8006=VECTOR('',#30655,1.);
#8007=VECTOR('',#30656,1.);
#8008=VECTOR('',#30665,1.);
#8009=VECTOR('',#30666,1.);
#8010=VECTOR('',#30667,1.);
#8011=VECTOR('',#30668,1.);
#8012=VECTOR('',#30671,1.);
#8013=VECTOR('',#30672,1.);
#8014=VECTOR('',#30673,1.);
#8015=VECTOR('',#30676,1.);
#8016=VECTOR('',#30677,1.);
#8017=VECTOR('',#30678,1.);
#8018=VECTOR('',#30681,1.);
#8019=VECTOR('',#30682,1.);
#8020=VECTOR('',#30687,1.);
#8021=VECTOR('',#30688,1.);
#8022=VECTOR('',#30689,1.);
#8023=VECTOR('',#30690,1.);
#8024=VECTOR('',#30693,1.);
#8025=VECTOR('',#30694,1.);
#8026=VECTOR('',#30695,1.);
#8027=VECTOR('',#30698,1.);
#8028=VECTOR('',#30699,1.);
#8029=VECTOR('',#30700,1.);
#8030=VECTOR('',#30703,1.);
#8031=VECTOR('',#30704,1.);
#8032=VECTOR('',#30711,0.3);
#8033=VECTOR('',#30718,1.);
#8034=VECTOR('',#30719,1.);
#8035=VECTOR('',#30720,1.);
#8036=VECTOR('',#30721,1.);
#8037=VECTOR('',#30724,1.);
#8038=VECTOR('',#30725,1.);
#8039=VECTOR('',#30726,1.);
#8040=VECTOR('',#30729,1.);
#8041=VECTOR('',#30730,1.);
#8042=VECTOR('',#30731,1.);
#8043=VECTOR('',#30734,1.);
#8044=VECTOR('',#30735,1.);
#8045=VECTOR('',#30740,1.);
#8046=VECTOR('',#30741,1.);
#8047=VECTOR('',#30742,1.);
#8048=VECTOR('',#30743,1.);
#8049=VECTOR('',#30746,1.);
#8050=VECTOR('',#30747,1.);
#8051=VECTOR('',#30748,1.);
#8052=VECTOR('',#30751,1.);
#8053=VECTOR('',#30752,1.);
#8054=VECTOR('',#30753,1.);
#8055=VECTOR('',#30756,1.);
#8056=VECTOR('',#30757,1.);
#8057=VECTOR('',#30762,1.);
#8058=VECTOR('',#30763,1.);
#8059=VECTOR('',#30764,1.);
#8060=VECTOR('',#30765,1.);
#8061=VECTOR('',#30768,1.);
#8062=VECTOR('',#30769,1.);
#8063=VECTOR('',#30770,1.);
#8064=VECTOR('',#30773,1.);
#8065=VECTOR('',#30774,1.);
#8066=VECTOR('',#30775,1.);
#8067=VECTOR('',#30778,1.);
#8068=VECTOR('',#30779,1.);
#8069=VECTOR('',#30784,1.);
#8070=VECTOR('',#30785,1.);
#8071=VECTOR('',#30786,1.);
#8072=VECTOR('',#30787,1.);
#8073=VECTOR('',#30790,1.);
#8074=VECTOR('',#30791,1.);
#8075=VECTOR('',#30792,1.);
#8076=VECTOR('',#30795,1.);
#8077=VECTOR('',#30796,1.);
#8078=VECTOR('',#30797,1.);
#8079=VECTOR('',#30800,1.);
#8080=VECTOR('',#30801,1.);
#8081=VECTOR('',#30808,0.135);
#8082=VECTOR('',#30815,0.135);
#8083=VECTOR('',#30822,0.135);
#8084=VECTOR('',#30829,0.8);
#8085=VECTOR('',#30840,3.8);
#8086=VECTOR('',#30847,0.1);
#8087=VECTOR('',#30848,0.1);
#8088=VECTOR('',#30855,0.1);
#8089=VECTOR('',#30858,0.1);
#8090=VECTOR('',#30861,0.0739);
#8091=VECTOR('',#30866,0.0739);
#8092=VECTOR('',#30869,0.0739);
#8093=VECTOR('',#30872,0.0739);
#8094=VECTOR('',#30891,0.0207846096908265);
#8095=VECTOR('',#30896,1.);
#8096=VECTOR('',#30897,1.);
#8097=VECTOR('',#30898,1.);
#8098=VECTOR('',#30899,1.);
#8099=VECTOR('',#30902,1.);
#8100=VECTOR('',#30903,1.);
#8101=VECTOR('',#30904,1.);
#8102=VECTOR('',#30907,1.);
#8103=VECTOR('',#30908,1.);
#8104=VECTOR('',#30909,1.);
#8105=VECTOR('',#30912,1.);
#8106=VECTOR('',#30913,1.);
#8107=VECTOR('',#30914,1.);
#8108=VECTOR('',#30917,1.);
#8109=VECTOR('',#30918,1.);
#8110=VECTOR('',#30919,1.);
#8111=VECTOR('',#30922,1.);
#8112=VECTOR('',#30923,1.);
#8113=VECTOR('',#30932,0.085);
#8114=VECTOR('',#30937,0.09);
#8115=VECTOR('',#30944,0.125);
#8116=VECTOR('',#30947,0.125);
#8117=VECTOR('',#30954,0.125);
#8118=VECTOR('',#30957,0.125);
#8119=VECTOR('',#30960,0.125);
#8120=VECTOR('',#30963,0.125);
#8121=VECTOR('',#30966,0.125);
#8122=VECTOR('',#30969,0.125);
#8123=VECTOR('',#30972,0.125);
#8124=VECTOR('',#30975,0.095825);
#8125=VECTOR('',#30980,0.095825);
#8126=VECTOR('',#30983,0.095825);
#8127=VECTOR('',#30986,0.095825);
#8128=VECTOR('',#30989,0.095825);
#8129=VECTOR('',#30992,0.095825);
#8130=VECTOR('',#30995,0.095825);
#8131=VECTOR('',#30998,0.095825);
#8132=VECTOR('',#31011,0.065);
#8133=VECTOR('',#31016,0.13);
#8134=VECTOR('',#31021,0.18);
#8135=VECTOR('',#31050,1.);
#8136=VECTOR('',#31051,1.);
#8137=VECTOR('',#31052,1.);
#8138=VECTOR('',#31053,1.);
#8139=VECTOR('',#31056,1.);
#8140=VECTOR('',#31057,1.);
#8141=VECTOR('',#31058,1.);
#8142=VECTOR('',#31061,1.);
#8143=VECTOR('',#31062,1.);
#8144=VECTOR('',#31063,1.);
#8145=VECTOR('',#31066,1.);
#8146=VECTOR('',#31067,1.);
#8147=VECTOR('',#31068,1.);
#8148=VECTOR('',#31071,1.);
#8149=VECTOR('',#31072,1.);
#8150=VECTOR('',#31099,1.);
#8151=VECTOR('',#31100,1.);
#8152=VECTOR('',#31107,0.115);
#8153=VECTOR('',#31110,1.);
#8154=VECTOR('',#31117,0.1);
#8155=VECTOR('',#31120,0.1);
#8156=VECTOR('',#31127,0.1);
#8157=VECTOR('',#31130,0.1);
#8158=VECTOR('',#31133,0.1);
#8159=VECTOR('',#31136,0.1);
#8160=VECTOR('',#31139,0.1);
#8161=VECTOR('',#31142,0.1);
#8162=VECTOR('',#31145,0.1);
#8163=VECTOR('',#31148,0.1);
#8164=VECTOR('',#31151,0.1);
#8165=VECTOR('',#31154,0.1);
#8166=VECTOR('',#31157,0.1);
#8167=VECTOR('',#31160,0.1);
#8168=VECTOR('',#31163,0.1);
#8169=VECTOR('',#31166,0.1);
#8170=VECTOR('',#31169,0.1);
#8171=VECTOR('',#31172,0.1);
#8172=VECTOR('',#31175,0.1);
#8173=VECTOR('',#31178,0.1);
#8174=VECTOR('',#31181,0.1);
#8175=VECTOR('',#31184,0.1);
#8176=VECTOR('',#31187,0.1);
#8177=VECTOR('',#31190,0.1);
#8178=VECTOR('',#31193,0.1);
#8179=VECTOR('',#31196,0.1);
#8180=VECTOR('',#31199,0.1);
#8181=VECTOR('',#31202,0.1);
#8182=VECTOR('',#31205,0.1);
#8183=VECTOR('',#31208,0.0739);
#8184=VECTOR('',#31213,0.0739);
#8185=VECTOR('',#31216,0.0739);
#8186=VECTOR('',#31219,0.0739);
#8187=VECTOR('',#31222,0.0739);
#8188=VECTOR('',#31225,0.0739);
#8189=VECTOR('',#31228,0.0739);
#8190=VECTOR('',#31231,0.0739);
#8191=VECTOR('',#31234,0.0739);
#8192=VECTOR('',#31237,0.0739);
#8193=VECTOR('',#31240,0.0739);
#8194=VECTOR('',#31243,0.0739);
#8195=VECTOR('',#31246,0.0739);
#8196=VECTOR('',#31249,0.0739);
#8197=VECTOR('',#31252,0.0739);
#8198=VECTOR('',#31255,0.0739);
#8199=VECTOR('',#31258,0.0739);
#8200=VECTOR('',#31261,0.0739);
#8201=VECTOR('',#31264,0.0739);
#8202=VECTOR('',#31267,0.0739);
#8203=VECTOR('',#31270,0.0739);
#8204=VECTOR('',#31273,0.0739);
#8205=VECTOR('',#31276,0.0739);
#8206=VECTOR('',#31279,0.0739);
#8207=VECTOR('',#31282,0.0739);
#8208=VECTOR('',#31285,0.0739);
#8209=VECTOR('',#31288,0.0739);
#8210=VECTOR('',#31291,0.0739);
#8211=VECTOR('',#31294,0.0739);
#8212=VECTOR('',#31313,1.);
#8213=VECTOR('',#31314,1.);
#8214=VECTOR('',#31317,1.);
#8215=VECTOR('',#31318,1.);
#8216=VECTOR('',#31321,1.);
#8217=VECTOR('',#31326,1.);
#8218=VECTOR('',#31327,1.);
#8219=VECTOR('',#31330,1.);
#8220=VECTOR('',#31331,1.);
#8221=VECTOR('',#31334,1.);
#8222=VECTOR('',#31339,1.);
#8223=VECTOR('',#31340,1.);
#8224=VECTOR('',#31343,1.);
#8225=VECTOR('',#31344,1.);
#8226=VECTOR('',#31347,1.);
#8227=VECTOR('',#31352,1.);
#8228=VECTOR('',#31353,1.);
#8229=VECTOR('',#31356,1.);
#8230=VECTOR('',#31357,1.);
#8231=VECTOR('',#31360,1.);
#8232=VECTOR('',#31365,1.);
#8233=VECTOR('',#31366,1.);
#8234=VECTOR('',#31369,1.);
#8235=VECTOR('',#31370,1.);
#8236=VECTOR('',#31373,1.);
#8237=VECTOR('',#31378,1.);
#8238=VECTOR('',#31379,1.);
#8239=VECTOR('',#31382,1.);
#8240=VECTOR('',#31383,1.);
#8241=VECTOR('',#31386,1.);
#8242=VECTOR('',#31391,1.);
#8243=VECTOR('',#31392,1.);
#8244=VECTOR('',#31395,1.);
#8245=VECTOR('',#31396,1.);
#8246=VECTOR('',#31399,1.);
#8247=VECTOR('',#31404,1.);
#8248=VECTOR('',#31405,1.);
#8249=VECTOR('',#31408,1.);
#8250=VECTOR('',#31409,1.);
#8251=VECTOR('',#31412,1.);
#8252=VECTOR('',#31417,1.);
#8253=VECTOR('',#31418,1.);
#8254=VECTOR('',#31421,1.);
#8255=VECTOR('',#31422,1.);
#8256=VECTOR('',#31425,1.);
#8257=VECTOR('',#31430,1.);
#8258=VECTOR('',#31431,1.);
#8259=VECTOR('',#31434,1.);
#8260=VECTOR('',#31435,1.);
#8261=VECTOR('',#31438,1.);
#8262=VECTOR('',#31443,1.);
#8263=VECTOR('',#31444,1.);
#8264=VECTOR('',#31447,1.);
#8265=VECTOR('',#31448,1.);
#8266=VECTOR('',#31451,1.);
#8267=VECTOR('',#31456,1.);
#8268=VECTOR('',#31457,1.);
#8269=VECTOR('',#31460,1.);
#8270=VECTOR('',#31461,1.);
#8271=VECTOR('',#31464,1.);
#8272=VECTOR('',#31469,1.);
#8273=VECTOR('',#31470,1.);
#8274=VECTOR('',#31473,1.);
#8275=VECTOR('',#31474,1.);
#8276=VECTOR('',#31477,1.);
#8277=VECTOR('',#31482,1.);
#8278=VECTOR('',#31483,1.);
#8279=VECTOR('',#31486,1.);
#8280=VECTOR('',#31487,1.);
#8281=VECTOR('',#31490,1.);
#8282=VECTOR('',#31495,1.);
#8283=VECTOR('',#31496,1.);
#8284=VECTOR('',#31499,1.);
#8285=VECTOR('',#31500,1.);
#8286=VECTOR('',#31503,1.);
#8287=VECTOR('',#31508,1.);
#8288=VECTOR('',#31509,1.);
#8289=VECTOR('',#31512,1.);
#8290=VECTOR('',#31513,1.);
#8291=VECTOR('',#31516,1.);
#8292=VECTOR('',#31521,1.);
#8293=VECTOR('',#31522,1.);
#8294=VECTOR('',#31525,1.);
#8295=VECTOR('',#31526,1.);
#8296=VECTOR('',#31529,1.);
#8297=VECTOR('',#31534,1.);
#8298=VECTOR('',#31535,1.);
#8299=VECTOR('',#31540,1.);
#8300=VECTOR('',#31541,1.);
#8301=VECTOR('',#31544,1.);
#8302=VECTOR('',#31549,1.);
#8303=VECTOR('',#31550,1.);
#8304=VECTOR('',#31553,1.);
#8305=VECTOR('',#31554,1.);
#8306=VECTOR('',#31557,1.);
#8307=VECTOR('',#31562,1.);
#8308=VECTOR('',#31563,1.);
#8309=VECTOR('',#31566,1.);
#8310=VECTOR('',#31567,1.);
#8311=VECTOR('',#31570,1.);
#8312=VECTOR('',#31575,1.);
#8313=VECTOR('',#31576,1.);
#8314=VECTOR('',#31579,1.);
#8315=VECTOR('',#31580,1.);
#8316=VECTOR('',#31583,1.);
#8317=VECTOR('',#31588,1.);
#8318=VECTOR('',#31589,1.);
#8319=VECTOR('',#31592,1.);
#8320=VECTOR('',#31593,1.);
#8321=VECTOR('',#31596,1.);
#8322=VECTOR('',#31601,1.);
#8323=VECTOR('',#31602,1.);
#8324=VECTOR('',#31605,1.);
#8325=VECTOR('',#31606,1.);
#8326=VECTOR('',#31609,1.);
#8327=VECTOR('',#31614,1.);
#8328=VECTOR('',#31615,1.);
#8329=VECTOR('',#31618,1.);
#8330=VECTOR('',#31619,1.);
#8331=VECTOR('',#31622,1.);
#8332=VECTOR('',#31627,1.);
#8333=VECTOR('',#31628,1.);
#8334=VECTOR('',#31631,1.);
#8335=VECTOR('',#31632,1.);
#8336=VECTOR('',#31635,1.);
#8337=VECTOR('',#31640,1.);
#8338=VECTOR('',#31641,1.);
#8339=VECTOR('',#31644,1.);
#8340=VECTOR('',#31645,1.);
#8341=VECTOR('',#31648,1.);
#8342=VECTOR('',#31653,1.);
#8343=VECTOR('',#31654,1.);
#8344=VECTOR('',#31657,1.);
#8345=VECTOR('',#31658,1.);
#8346=VECTOR('',#31661,1.);
#8347=VECTOR('',#31666,1.);
#8348=VECTOR('',#31667,1.);
#8349=VECTOR('',#31670,1.);
#8350=VECTOR('',#31671,1.);
#8351=VECTOR('',#31674,1.);
#8352=VECTOR('',#31679,1.);
#8353=VECTOR('',#31680,1.);
#8354=VECTOR('',#31683,1.);
#8355=VECTOR('',#31684,1.);
#8356=VECTOR('',#31687,1.);
#8357=VECTOR('',#31692,1.);
#8358=VECTOR('',#31693,1.);
#8359=VECTOR('',#31696,1.);
#8360=VECTOR('',#31697,1.);
#8361=VECTOR('',#31700,1.);
#8362=VECTOR('',#31705,1.);
#8363=VECTOR('',#31706,1.);
#8364=VECTOR('',#31709,1.);
#8365=VECTOR('',#31710,1.);
#8366=VECTOR('',#31713,1.);
#8367=VECTOR('',#31718,1.);
#8368=VECTOR('',#31719,1.);
#8369=VECTOR('',#31722,1.);
#8370=VECTOR('',#31723,1.);
#8371=VECTOR('',#31726,1.);
#8372=VECTOR('',#31731,1.);
#8373=VECTOR('',#31732,1.);
#8374=VECTOR('',#31735,1.);
#8375=VECTOR('',#31736,1.);
#8376=VECTOR('',#31739,1.);
#8377=VECTOR('',#31744,1.);
#8378=VECTOR('',#31745,1.);
#8379=VECTOR('',#31748,1.);
#8380=VECTOR('',#31749,1.);
#8381=VECTOR('',#31752,1.);
#8382=VECTOR('',#31757,1.);
#8383=VECTOR('',#31758,1.);
#8384=VECTOR('',#31761,1.);
#8385=VECTOR('',#31762,1.);
#8386=VECTOR('',#31765,1.);
#8387=VECTOR('',#31802,0.19);
#8388=VECTOR('',#31841,1.);
#8389=VECTOR('',#31844,1.);
#8390=VECTOR('',#31849,1.);
#8391=VECTOR('',#31850,1.);
#8392=VECTOR('',#31853,1.);
#8393=VECTOR('',#31860,0.1825);
#8394=VECTOR('',#31863,0.0346410161513776);
#8395=VECTOR('',#31868,1.);
#8396=VECTOR('',#31869,1.);
#8397=VECTOR('',#31870,1.);
#8398=VECTOR('',#31871,1.);
#8399=VECTOR('',#31874,1.);
#8400=VECTOR('',#31875,1.);
#8401=VECTOR('',#31876,1.);
#8402=VECTOR('',#31879,1.);
#8403=VECTOR('',#31880,1.);
#8404=VECTOR('',#31881,1.);
#8405=VECTOR('',#31884,1.);
#8406=VECTOR('',#31885,1.);
#8407=VECTOR('',#31886,1.);
#8408=VECTOR('',#31889,1.);
#8409=VECTOR('',#31890,1.);
#8410=VECTOR('',#31891,1.);
#8411=VECTOR('',#31894,1.);
#8412=VECTOR('',#31895,1.);
#8413=VECTOR('',#31904,0.088);
#8414=VECTOR('',#31913,0.105);
#8415=VECTOR('',#31922,0.1);
#8416=VECTOR('',#31925,0.1);
#8417=VECTOR('',#31932,0.1);
#8418=VECTOR('',#31935,0.1);
#8419=VECTOR('',#31938,0.1);
#8420=VECTOR('',#31941,0.1);
#8421=VECTOR('',#31944,0.1);
#8422=VECTOR('',#31947,0.1);
#8423=VECTOR('',#31950,0.1);
#8424=VECTOR('',#31953,0.1);
#8425=VECTOR('',#31956,0.1);
#8426=VECTOR('',#31959,0.1);
#8427=VECTOR('',#31962,0.1);
#8428=VECTOR('',#31965,0.1);
#8429=VECTOR('',#31968,0.1);
#8430=VECTOR('',#31971,0.1);
#8431=VECTOR('',#31974,0.1);
#8432=VECTOR('',#31977,0.1);
#8433=VECTOR('',#31980,0.1);
#8434=VECTOR('',#31983,0.1);
#8435=VECTOR('',#31986,0.1);
#8436=VECTOR('',#31989,0.1);
#8437=VECTOR('',#31992,0.1);
#8438=VECTOR('',#31995,0.1);
#8439=VECTOR('',#31998,0.0739);
#8440=VECTOR('',#32003,0.0739);
#8441=VECTOR('',#32006,0.0739);
#8442=VECTOR('',#32009,0.0739);
#8443=VECTOR('',#32012,0.0739);
#8444=VECTOR('',#32015,0.0739);
#8445=VECTOR('',#32018,0.0739);
#8446=VECTOR('',#32021,0.0739);
#8447=VECTOR('',#32024,0.0739);
#8448=VECTOR('',#32027,0.0739);
#8449=VECTOR('',#32030,0.0739);
#8450=VECTOR('',#32033,0.0739);
#8451=VECTOR('',#32036,0.0739);
#8452=VECTOR('',#32039,0.0739);
#8453=VECTOR('',#32042,0.0739);
#8454=VECTOR('',#32045,0.0739);
#8455=VECTOR('',#32048,0.0739);
#8456=VECTOR('',#32051,0.0739);
#8457=VECTOR('',#32054,0.0739);
#8458=VECTOR('',#32057,0.0739);
#8459=VECTOR('',#32060,0.0739);
#8460=VECTOR('',#32063,0.0739);
#8461=VECTOR('',#32066,0.0739);
#8462=VECTOR('',#32069,0.0739);
#8463=VECTOR('',#32088,1.);
#8464=VECTOR('',#32089,1.);
#8465=VECTOR('',#32092,1.);
#8466=VECTOR('',#32093,1.);
#8467=VECTOR('',#32096,1.);
#8468=VECTOR('',#32101,1.);
#8469=VECTOR('',#32102,1.);
#8470=VECTOR('',#32105,1.);
#8471=VECTOR('',#32106,1.);
#8472=VECTOR('',#32109,1.);
#8473=VECTOR('',#32114,1.);
#8474=VECTOR('',#32115,1.);
#8475=VECTOR('',#32118,1.);
#8476=VECTOR('',#32119,1.);
#8477=VECTOR('',#32122,1.);
#8478=VECTOR('',#32127,1.);
#8479=VECTOR('',#32128,1.);
#8480=VECTOR('',#32131,1.);
#8481=VECTOR('',#32132,1.);
#8482=VECTOR('',#32135,1.);
#8483=VECTOR('',#32140,1.);
#8484=VECTOR('',#32141,1.);
#8485=VECTOR('',#32144,1.);
#8486=VECTOR('',#32145,1.);
#8487=VECTOR('',#32148,1.);
#8488=VECTOR('',#32153,1.);
#8489=VECTOR('',#32154,1.);
#8490=VECTOR('',#32157,1.);
#8491=VECTOR('',#32158,1.);
#8492=VECTOR('',#32161,1.);
#8493=VECTOR('',#32166,1.);
#8494=VECTOR('',#32167,1.);
#8495=VECTOR('',#32170,1.);
#8496=VECTOR('',#32171,1.);
#8497=VECTOR('',#32174,1.);
#8498=VECTOR('',#32179,1.);
#8499=VECTOR('',#32180,1.);
#8500=VECTOR('',#32183,1.);
#8501=VECTOR('',#32184,1.);
#8502=VECTOR('',#32187,1.);
#8503=VECTOR('',#32192,1.);
#8504=VECTOR('',#32193,1.);
#8505=VECTOR('',#32196,1.);
#8506=VECTOR('',#32197,1.);
#8507=VECTOR('',#32200,1.);
#8508=VECTOR('',#32205,1.);
#8509=VECTOR('',#32206,1.);
#8510=VECTOR('',#32209,1.);
#8511=VECTOR('',#32210,1.);
#8512=VECTOR('',#32213,1.);
#8513=VECTOR('',#32218,1.);
#8514=VECTOR('',#32219,1.);
#8515=VECTOR('',#32222,1.);
#8516=VECTOR('',#32223,1.);
#8517=VECTOR('',#32226,1.);
#8518=VECTOR('',#32231,1.);
#8519=VECTOR('',#32232,1.);
#8520=VECTOR('',#32235,1.);
#8521=VECTOR('',#32236,1.);
#8522=VECTOR('',#32239,1.);
#8523=VECTOR('',#32244,1.);
#8524=VECTOR('',#32245,1.);
#8525=VECTOR('',#32248,1.);
#8526=VECTOR('',#32249,1.);
#8527=VECTOR('',#32252,1.);
#8528=VECTOR('',#32257,1.);
#8529=VECTOR('',#32258,1.);
#8530=VECTOR('',#32261,1.);
#8531=VECTOR('',#32262,1.);
#8532=VECTOR('',#32265,1.);
#8533=VECTOR('',#32270,1.);
#8534=VECTOR('',#32271,1.);
#8535=VECTOR('',#32274,1.);
#8536=VECTOR('',#32275,1.);
#8537=VECTOR('',#32278,1.);
#8538=VECTOR('',#32283,1.);
#8539=VECTOR('',#32284,1.);
#8540=VECTOR('',#32287,1.);
#8541=VECTOR('',#32288,1.);
#8542=VECTOR('',#32291,1.);
#8543=VECTOR('',#32296,1.);
#8544=VECTOR('',#32297,1.);
#8545=VECTOR('',#32300,1.);
#8546=VECTOR('',#32301,1.);
#8547=VECTOR('',#32304,1.);
#8548=VECTOR('',#32309,1.);
#8549=VECTOR('',#32310,1.);
#8550=VECTOR('',#32315,1.);
#8551=VECTOR('',#32316,1.);
#8552=VECTOR('',#32319,1.);
#8553=VECTOR('',#32324,1.);
#8554=VECTOR('',#32325,1.);
#8555=VECTOR('',#32328,1.);
#8556=VECTOR('',#32329,1.);
#8557=VECTOR('',#32332,1.);
#8558=VECTOR('',#32337,1.);
#8559=VECTOR('',#32338,1.);
#8560=VECTOR('',#32341,1.);
#8561=VECTOR('',#32342,1.);
#8562=VECTOR('',#32345,1.);
#8563=VECTOR('',#32350,1.);
#8564=VECTOR('',#32351,1.);
#8565=VECTOR('',#32354,1.);
#8566=VECTOR('',#32355,1.);
#8567=VECTOR('',#32358,1.);
#8568=VECTOR('',#32363,1.);
#8569=VECTOR('',#32364,1.);
#8570=VECTOR('',#32367,1.);
#8571=VECTOR('',#32368,1.);
#8572=VECTOR('',#32371,1.);
#8573=VECTOR('',#32376,1.);
#8574=VECTOR('',#32377,1.);
#8575=VECTOR('',#32380,1.);
#8576=VECTOR('',#32381,1.);
#8577=VECTOR('',#32384,1.);
#8578=VECTOR('',#32389,1.);
#8579=VECTOR('',#32390,1.);
#8580=VECTOR('',#32393,1.);
#8581=VECTOR('',#32394,1.);
#8582=VECTOR('',#32397,1.);
#8583=VECTOR('',#32402,1.);
#8584=VECTOR('',#32403,1.);
#8585=VECTOR('',#32406,1.);
#8586=VECTOR('',#32407,1.);
#8587=VECTOR('',#32410,1.);
#8588=VECTOR('',#32415,1.);
#8589=VECTOR('',#32416,1.);
#8590=VECTOR('',#32419,1.);
#8591=VECTOR('',#32420,1.);
#8592=VECTOR('',#32423,1.);
#8593=VECTOR('',#32428,1.);
#8594=VECTOR('',#32429,1.);
#8595=VECTOR('',#32432,1.);
#8596=VECTOR('',#32433,1.);
#8597=VECTOR('',#32436,1.);
#8598=VECTOR('',#32441,1.);
#8599=VECTOR('',#32442,1.);
#8600=VECTOR('',#32445,1.);
#8601=VECTOR('',#32446,1.);
#8602=VECTOR('',#32449,1.);
#8603=VECTOR('',#32454,1.);
#8604=VECTOR('',#32455,1.);
#8605=VECTOR('',#32458,1.);
#8606=VECTOR('',#32459,1.);
#8607=VECTOR('',#32462,1.);
#8608=VECTOR('',#32467,1.);
#8609=VECTOR('',#32468,1.);
#8610=VECTOR('',#32471,1.);
#8611=VECTOR('',#32472,1.);
#8612=VECTOR('',#32475,1.);
#8613=VECTOR('',#32480,1.);
#8614=VECTOR('',#32481,1.);
#8615=VECTOR('',#32484,1.);
#8616=VECTOR('',#32485,1.);
#8617=VECTOR('',#32488,1.);
#8618=VECTOR('',#32493,1.);
#8619=VECTOR('',#32494,1.);
#8620=VECTOR('',#32497,1.);
#8621=VECTOR('',#32498,1.);
#8622=VECTOR('',#32501,1.);
#8623=VECTOR('',#32506,1.);
#8624=VECTOR('',#32507,1.);
#8625=VECTOR('',#32510,1.);
#8626=VECTOR('',#32511,1.);
#8627=VECTOR('',#32514,1.);
#8628=VECTOR('',#32519,1.);
#8629=VECTOR('',#32520,1.);
#8630=VECTOR('',#32523,1.);
#8631=VECTOR('',#32524,1.);
#8632=VECTOR('',#32527,1.);
#8633=VECTOR('',#32532,1.);
#8634=VECTOR('',#32533,1.);
#8635=VECTOR('',#32536,1.);
#8636=VECTOR('',#32537,1.);
#8637=VECTOR('',#32540,1.);
#8638=VECTOR('',#32577,0.19);
#8639=VECTOR('',#32616,1.);
#8640=VECTOR('',#32619,1.);
#8641=VECTOR('',#32624,1.);
#8642=VECTOR('',#32625,1.);
#8643=VECTOR('',#32628,1.);
#8644=VECTOR('',#32635,0.1825);
#8645=VECTOR('',#32638,0.0346410161513776);
#8646=VECTOR('',#32643,1.);
#8647=VECTOR('',#32644,1.);
#8648=VECTOR('',#32645,1.);
#8649=VECTOR('',#32646,1.);
#8650=VECTOR('',#32649,1.);
#8651=VECTOR('',#32650,1.);
#8652=VECTOR('',#32651,1.);
#8653=VECTOR('',#32654,1.);
#8654=VECTOR('',#32655,1.);
#8655=VECTOR('',#32656,1.);
#8656=VECTOR('',#32659,1.);
#8657=VECTOR('',#32660,1.);
#8658=VECTOR('',#32661,1.);
#8659=VECTOR('',#32664,1.);
#8660=VECTOR('',#32665,1.);
#8661=VECTOR('',#32666,1.);
#8662=VECTOR('',#32669,1.);
#8663=VECTOR('',#32670,1.);
#8664=VECTOR('',#32679,0.088);
#8665=VECTOR('',#32688,0.105);
#8666=VECTOR('',#32697,0.125);
#8667=VECTOR('',#32700,0.125);
#8668=VECTOR('',#32707,0.125);
#8669=VECTOR('',#32710,0.125);
#8670=VECTOR('',#32713,0.125);
#8671=VECTOR('',#32716,0.125);
#8672=VECTOR('',#32719,0.125);
#8673=VECTOR('',#32722,0.125);
#8674=VECTOR('',#32725,0.125);
#8675=VECTOR('',#32728,0.125);
#8676=VECTOR('',#32731,0.125);
#8677=VECTOR('',#32734,0.125);
#8678=VECTOR('',#32737,0.125);
#8679=VECTOR('',#32740,0.095825);
#8680=VECTOR('',#32745,0.095825);
#8681=VECTOR('',#32748,0.095825);
#8682=VECTOR('',#32751,0.095825);
#8683=VECTOR('',#32754,0.095825);
#8684=VECTOR('',#32757,0.095825);
#8685=VECTOR('',#32760,0.095825);
#8686=VECTOR('',#32763,0.095825);
#8687=VECTOR('',#32766,0.095825);
#8688=VECTOR('',#32769,0.095825);
#8689=VECTOR('',#32772,0.095825);
#8690=VECTOR('',#32775,0.095825);
#8691=VECTOR('',#32798,1.);
#8692=VECTOR('',#32799,1.);
#8693=VECTOR('',#32802,1.);
#8694=VECTOR('',#32803,1.);
#8695=VECTOR('',#32806,1.);
#8696=VECTOR('',#32811,1.);
#8697=VECTOR('',#32812,1.);
#8698=VECTOR('',#32815,1.);
#8699=VECTOR('',#32816,1.);
#8700=VECTOR('',#32819,1.);
#8701=VECTOR('',#32824,1.);
#8702=VECTOR('',#32825,1.);
#8703=VECTOR('',#32828,1.);
#8704=VECTOR('',#32829,1.);
#8705=VECTOR('',#32832,1.);
#8706=VECTOR('',#32837,1.);
#8707=VECTOR('',#32838,1.);
#8708=VECTOR('',#32841,1.);
#8709=VECTOR('',#32842,1.);
#8710=VECTOR('',#32845,1.);
#8711=VECTOR('',#32850,1.);
#8712=VECTOR('',#32851,1.);
#8713=VECTOR('',#32854,1.);
#8714=VECTOR('',#32855,1.);
#8715=VECTOR('',#32858,1.);
#8716=VECTOR('',#32863,1.);
#8717=VECTOR('',#32864,1.);
#8718=VECTOR('',#32867,1.);
#8719=VECTOR('',#32868,1.);
#8720=VECTOR('',#32871,1.);
#8721=VECTOR('',#32876,1.);
#8722=VECTOR('',#32877,1.);
#8723=VECTOR('',#32880,1.);
#8724=VECTOR('',#32881,1.);
#8725=VECTOR('',#32884,1.);
#8726=VECTOR('',#32889,1.);
#8727=VECTOR('',#32890,1.);
#8728=VECTOR('',#32893,1.);
#8729=VECTOR('',#32894,1.);
#8730=VECTOR('',#32897,1.);
#8731=VECTOR('',#32902,1.);
#8732=VECTOR('',#32903,1.);
#8733=VECTOR('',#32906,1.);
#8734=VECTOR('',#32907,1.);
#8735=VECTOR('',#32910,1.);
#8736=VECTOR('',#32915,1.);
#8737=VECTOR('',#32916,1.);
#8738=VECTOR('',#32919,1.);
#8739=VECTOR('',#32920,1.);
#8740=VECTOR('',#32923,1.);
#8741=VECTOR('',#32928,1.);
#8742=VECTOR('',#32929,1.);
#8743=VECTOR('',#32932,1.);
#8744=VECTOR('',#32933,1.);
#8745=VECTOR('',#32936,1.);
#8746=VECTOR('',#32941,1.);
#8747=VECTOR('',#32942,1.);
#8748=VECTOR('',#32945,1.);
#8749=VECTOR('',#32946,1.);
#8750=VECTOR('',#32949,1.);
#8751=VECTOR('',#32954,1.);
#8752=VECTOR('',#32955,1.);
#8753=VECTOR('',#32958,1.);
#8754=VECTOR('',#32959,1.);
#8755=VECTOR('',#32962,1.);
#8756=VECTOR('',#32967,1.);
#8757=VECTOR('',#32968,1.);
#8758=VECTOR('',#32971,1.);
#8759=VECTOR('',#32972,1.);
#8760=VECTOR('',#32975,1.);
#8761=VECTOR('',#32980,1.);
#8762=VECTOR('',#32981,1.);
#8763=VECTOR('',#32984,1.);
#8764=VECTOR('',#32985,1.);
#8765=VECTOR('',#32988,1.);
#8766=VECTOR('',#32993,1.);
#8767=VECTOR('',#32994,1.);
#8768=VECTOR('',#32997,1.);
#8769=VECTOR('',#32998,1.);
#8770=VECTOR('',#33001,1.);
#8771=VECTOR('',#33006,1.);
#8772=VECTOR('',#33007,1.);
#8773=VECTOR('',#33010,1.);
#8774=VECTOR('',#33011,1.);
#8775=VECTOR('',#33014,1.);
#8776=VECTOR('',#33019,1.);
#8777=VECTOR('',#33020,1.);
#8778=VECTOR('',#33025,1.);
#8779=VECTOR('',#33026,1.);
#8780=VECTOR('',#33029,1.);
#8781=VECTOR('',#33034,1.);
#8782=VECTOR('',#33035,1.);
#8783=VECTOR('',#33038,1.);
#8784=VECTOR('',#33039,1.);
#8785=VECTOR('',#33042,1.);
#8786=VECTOR('',#33047,1.);
#8787=VECTOR('',#33048,1.);
#8788=VECTOR('',#33051,1.);
#8789=VECTOR('',#33052,1.);
#8790=VECTOR('',#33055,1.);
#8791=VECTOR('',#33060,1.);
#8792=VECTOR('',#33061,1.);
#8793=VECTOR('',#33064,1.);
#8794=VECTOR('',#33065,1.);
#8795=VECTOR('',#33068,1.);
#8796=VECTOR('',#33073,1.);
#8797=VECTOR('',#33074,1.);
#8798=VECTOR('',#33077,1.);
#8799=VECTOR('',#33078,1.);
#8800=VECTOR('',#33081,1.);
#8801=VECTOR('',#33086,1.);
#8802=VECTOR('',#33087,1.);
#8803=VECTOR('',#33090,1.);
#8804=VECTOR('',#33091,1.);
#8805=VECTOR('',#33094,1.);
#8806=VECTOR('',#33099,1.);
#8807=VECTOR('',#33100,1.);
#8808=VECTOR('',#33103,1.);
#8809=VECTOR('',#33104,1.);
#8810=VECTOR('',#33107,1.);
#8811=VECTOR('',#33112,1.);
#8812=VECTOR('',#33113,1.);
#8813=VECTOR('',#33116,1.);
#8814=VECTOR('',#33117,1.);
#8815=VECTOR('',#33120,1.);
#8816=VECTOR('',#33125,1.);
#8817=VECTOR('',#33126,1.);
#8818=VECTOR('',#33129,1.);
#8819=VECTOR('',#33130,1.);
#8820=VECTOR('',#33133,1.);
#8821=VECTOR('',#33138,1.);
#8822=VECTOR('',#33139,1.);
#8823=VECTOR('',#33142,1.);
#8824=VECTOR('',#33143,1.);
#8825=VECTOR('',#33146,1.);
#8826=VECTOR('',#33151,1.);
#8827=VECTOR('',#33152,1.);
#8828=VECTOR('',#33155,1.);
#8829=VECTOR('',#33156,1.);
#8830=VECTOR('',#33159,1.);
#8831=VECTOR('',#33164,1.);
#8832=VECTOR('',#33165,1.);
#8833=VECTOR('',#33168,1.);
#8834=VECTOR('',#33169,1.);
#8835=VECTOR('',#33172,1.);
#8836=VECTOR('',#33177,1.);
#8837=VECTOR('',#33178,1.);
#8838=VECTOR('',#33181,1.);
#8839=VECTOR('',#33182,1.);
#8840=VECTOR('',#33185,1.);
#8841=VECTOR('',#33190,1.);
#8842=VECTOR('',#33191,1.);
#8843=VECTOR('',#33194,1.);
#8844=VECTOR('',#33195,1.);
#8845=VECTOR('',#33198,1.);
#8846=VECTOR('',#33203,1.);
#8847=VECTOR('',#33204,1.);
#8848=VECTOR('',#33207,1.);
#8849=VECTOR('',#33208,1.);
#8850=VECTOR('',#33211,1.);
#8851=VECTOR('',#33216,1.);
#8852=VECTOR('',#33217,1.);
#8853=VECTOR('',#33220,1.);
#8854=VECTOR('',#33221,1.);
#8855=VECTOR('',#33224,1.);
#8856=VECTOR('',#33229,1.);
#8857=VECTOR('',#33230,1.);
#8858=VECTOR('',#33233,1.);
#8859=VECTOR('',#33234,1.);
#8860=VECTOR('',#33237,1.);
#8861=VECTOR('',#33242,1.);
#8862=VECTOR('',#33243,1.);
#8863=VECTOR('',#33246,1.);
#8864=VECTOR('',#33247,1.);
#8865=VECTOR('',#33250,1.);
#8866=VECTOR('',#33287,0.225);
#8867=VECTOR('',#33326,1.);
#8868=VECTOR('',#33329,1.);
#8869=VECTOR('',#33334,1.);
#8870=VECTOR('',#33335,1.);
#8871=VECTOR('',#33338,1.);
#8872=VECTOR('',#33345,0.2175);
#8873=VECTOR('',#33348,0.0461880215351701);
#8874=VECTOR('',#33353,1.);
#8875=VECTOR('',#33354,1.);
#8876=VECTOR('',#33355,1.);
#8877=VECTOR('',#33356,1.);
#8878=VECTOR('',#33359,1.);
#8879=VECTOR('',#33360,1.);
#8880=VECTOR('',#33361,1.);
#8881=VECTOR('',#33364,1.);
#8882=VECTOR('',#33365,1.);
#8883=VECTOR('',#33366,1.);
#8884=VECTOR('',#33369,1.);
#8885=VECTOR('',#33370,1.);
#8886=VECTOR('',#33371,1.);
#8887=VECTOR('',#33374,1.);
#8888=VECTOR('',#33375,1.);
#8889=VECTOR('',#33376,1.);
#8890=VECTOR('',#33379,1.);
#8891=VECTOR('',#33380,1.);
#8892=VECTOR('',#33389,0.11);
#8893=VECTOR('',#33394,0.13);
#8894=VECTOR('',#33403,0.08);
#8895=VECTOR('',#33406,0.08);
#8896=VECTOR('',#33413,0.08);
#8897=VECTOR('',#33416,0.08);
#8898=VECTOR('',#33419,0.08);
#8899=VECTOR('',#33422,0.08);
#8900=VECTOR('',#33425,0.08);
#8901=VECTOR('',#33428,0.08);
#8902=VECTOR('',#33431,0.056925);
#8903=VECTOR('',#33436,0.056925);
#8904=VECTOR('',#33439,0.056925);
#8905=VECTOR('',#33442,0.056925);
#8906=VECTOR('',#33445,0.056925);
#8907=VECTOR('',#33448,0.056925);
#8908=VECTOR('',#33451,0.056925);
#8909=VECTOR('',#33454,0.056925);
#8910=VECTOR('',#33465,1.);
#8911=VECTOR('',#33466,1.);
#8912=VECTOR('',#33467,1.);
#8913=VECTOR('',#33468,1.);
#8914=VECTOR('',#33471,1.);
#8915=VECTOR('',#33472,1.);
#8916=VECTOR('',#33473,1.);
#8917=VECTOR('',#33474,1.);
#8918=VECTOR('',#33477,1.);
#8919=VECTOR('',#33478,1.);
#8920=VECTOR('',#33479,1.);
#8921=VECTOR('',#33480,1.);
#8922=VECTOR('',#33483,1.);
#8923=VECTOR('',#33484,1.);
#8924=VECTOR('',#33485,1.);
#8925=VECTOR('',#33488,1.);
#8926=VECTOR('',#33489,1.);
#8927=VECTOR('',#33492,1.);
#8928=VECTOR('',#33493,1.);
#8929=VECTOR('',#33494,1.);
#8930=VECTOR('',#33499,1.);
#8931=VECTOR('',#33500,1.);
#8932=VECTOR('',#33501,1.);
#8933=VECTOR('',#33502,1.);
#8934=VECTOR('',#33503,1.);
#8935=VECTOR('',#33504,1.);
#8936=VECTOR('',#33507,1.);
#8937=VECTOR('',#33508,1.);
#8938=VECTOR('',#33511,1.);
#8939=VECTOR('',#33512,1.);
#8940=VECTOR('',#33515,1.);
#8941=VECTOR('',#33516,1.);
#8942=VECTOR('',#33519,1.);
#8943=VECTOR('',#33520,1.);
#8944=VECTOR('',#33523,1.);
#8945=VECTOR('',#33526,1.);
#8946=VECTOR('',#33535,0.0704);
#8947=VECTOR('',#33548,0.16);
#8948=VECTOR('',#33551,0.14375);
#8949=VECTOR('',#33556,0.08);
#8950=VECTOR('',#33559,0.08);
#8951=VECTOR('',#33566,0.08);
#8952=VECTOR('',#33569,0.08);
#8953=VECTOR('',#33572,0.08);
#8954=VECTOR('',#33575,0.08);
#8955=VECTOR('',#33578,0.08);
#8956=VECTOR('',#33581,0.08);
#8957=VECTOR('',#33584,0.08);
#8958=VECTOR('',#33587,0.08);
#8959=VECTOR('',#33590,0.08);
#8960=VECTOR('',#33593,0.08);
#8961=VECTOR('',#33596,0.08);
#8962=VECTOR('',#33599,0.08);
#8963=VECTOR('',#33602,0.08);
#8964=VECTOR('',#33605,0.08);
#8965=VECTOR('',#33608,0.08);
#8966=VECTOR('',#33611,0.056925);
#8967=VECTOR('',#33616,0.056925);
#8968=VECTOR('',#33621,0.056925);
#8969=VECTOR('',#33624,0.056925);
#8970=VECTOR('',#33627,0.056925);
#8971=VECTOR('',#33630,0.056925);
#8972=VECTOR('',#33633,0.056925);
#8973=VECTOR('',#33636,0.056925);
#8974=VECTOR('',#33639,0.056925);
#8975=VECTOR('',#33642,0.056925);
#8976=VECTOR('',#33645,0.056925);
#8977=VECTOR('',#33648,0.056925);
#8978=VECTOR('',#33651,0.056925);
#8979=VECTOR('',#33654,0.056925);
#8980=VECTOR('',#33657,0.056925);
#8981=VECTOR('',#33660,0.056925);
#8982=VECTOR('',#33663,0.056925);
#8983=VECTOR('',#33678,1.);
#8984=VECTOR('',#33679,1.);
#8985=VECTOR('',#33680,1.);
#8986=VECTOR('',#33681,1.);
#8987=VECTOR('',#33684,1.);
#8988=VECTOR('',#33685,1.);
#8989=VECTOR('',#33686,1.);
#8990=VECTOR('',#33687,1.);
#8991=VECTOR('',#33690,1.);
#8992=VECTOR('',#33691,1.);
#8993=VECTOR('',#33692,1.);
#8994=VECTOR('',#33693,1.);
#8995=VECTOR('',#33696,1.);
#8996=VECTOR('',#33697,1.);
#8997=VECTOR('',#33698,1.);
#8998=VECTOR('',#33701,1.);
#8999=VECTOR('',#33702,1.);
#9000=VECTOR('',#33705,1.);
#9001=VECTOR('',#33706,1.);
#9002=VECTOR('',#33707,1.);
#9003=VECTOR('',#33712,1.);
#9004=VECTOR('',#33713,1.);
#9005=VECTOR('',#33714,1.);
#9006=VECTOR('',#33715,1.);
#9007=VECTOR('',#33716,1.);
#9008=VECTOR('',#33717,1.);
#9009=VECTOR('',#33720,1.);
#9010=VECTOR('',#33721,1.);
#9011=VECTOR('',#33724,1.);
#9012=VECTOR('',#33725,1.);
#9013=VECTOR('',#33728,1.);
#9014=VECTOR('',#33729,1.);
#9015=VECTOR('',#33732,1.);
#9016=VECTOR('',#33733,1.);
#9017=VECTOR('',#33736,1.);
#9018=VECTOR('',#33739,1.);
#9019=VECTOR('',#33748,0.0704);
#9020=VECTOR('',#33757,0.16);
#9021=VECTOR('',#33760,0.14375);
#9022=CIRCLE('',#24773,4.7287867965644);
#9023=CIRCLE('',#24774,4.75);
#9024=CIRCLE('',#24775,4.75);
#9025=CIRCLE('',#24777,4.6912132034356);
#9026=CIRCLE('',#24779,4.75);
#9027=CIRCLE('',#24781,4.6912132034356);
#9028=CIRCLE('',#24782,4.64);
#9029=CIRCLE('',#24784,4.7287867965644);
#9030=CIRCLE('',#24786,4.095);
#9031=CIRCLE('',#24787,0.128333333333333);
#9032=CIRCLE('',#24788,0.128333333333333);
#9033=CIRCLE('',#24789,0.128333333333333);
#9034=CIRCLE('',#24790,0.128333333333333);
#9035=CIRCLE('',#24791,0.128333333333334);
#9036=CIRCLE('',#24792,0.128333333333333);
#9037=CIRCLE('',#24794,4.64);
#9038=CIRCLE('',#24796,0.78);
#9039=CIRCLE('',#24797,0.24);
#9040=CIRCLE('',#24798,0.24);
#9041=CIRCLE('',#24799,0.24);
#9042=CIRCLE('',#24800,0.24);
#9043=CIRCLE('',#24801,0.24);
#9044=CIRCLE('',#24802,0.24);
#9045=CIRCLE('',#24804,0.728786796564404);
#9046=CIRCLE('',#24806,0.721213203435596);
#9047=CIRCLE('',#24808,0.7);
#9048=CIRCLE('',#24809,0.7);
#9049=CIRCLE('',#24811,0.7);
#9050=CIRCLE('',#24812,0.7);
#9051=CIRCLE('',#24814,0.721213203435596);
#9052=CIRCLE('',#24816,0.728786796564404);
#9053=CIRCLE('',#24818,0.78);
#9054=CIRCLE('',#24820,4.055);
#9055=CIRCLE('',#24821,0.18);
#9056=CIRCLE('',#24822,0.18);
#9057=CIRCLE('',#24823,0.18);
#9058=CIRCLE('',#24825,0.21);
#9059=CIRCLE('',#24826,0.21);
#9060=CIRCLE('',#24828,0.21);
#9061=CIRCLE('',#24830,0.21);
#9062=CIRCLE('',#24831,0.21);
#9063=CIRCLE('',#24833,0.21);
#9064=CIRCLE('',#24835,0.21);
#9065=CIRCLE('',#24836,0.21);
#9066=CIRCLE('',#24838,0.21);
#9067=CIRCLE('',#24840,0.21);
#9068=CIRCLE('',#24841,0.21);
#9069=CIRCLE('',#24843,0.21);
#9070=CIRCLE('',#24845,0.21);
#9071=CIRCLE('',#24846,0.21);
#9072=CIRCLE('',#24848,0.21);
#9073=CIRCLE('',#24850,0.21);
#9074=CIRCLE('',#24851,0.21);
#9075=CIRCLE('',#24853,0.21);
#9076=CIRCLE('',#24855,4.75);
#9077=CIRCLE('',#24856,4.75);
#9078=CIRCLE('',#24858,4.75);
#9079=CIRCLE('',#24860,4.72);
#9080=CIRCLE('',#24862,4.66);
#9081=CIRCLE('',#24864,4.72);
#9082=CIRCLE('',#24866,4.66);
#9083=CIRCLE('',#24869,0.13);
#9084=CIRCLE('',#24871,0.13);
#9085=CIRCLE('',#24874,0.13);
#9086=CIRCLE('',#24876,0.13);
#9087=CIRCLE('',#24879,0.13);
#9088=CIRCLE('',#24881,0.13);
#9089=CIRCLE('',#24884,0.12);
#9090=CIRCLE('',#24886,0.12);
#9091=CIRCLE('',#24888,0.145);
#9092=CIRCLE('',#24891,0.12);
#9093=CIRCLE('',#24893,0.12);
#9094=CIRCLE('',#24895,0.145);
#9095=CIRCLE('',#24898,0.12);
#9096=CIRCLE('',#24900,0.12);
#9097=CIRCLE('',#24902,0.145);
#9098=CIRCLE('',#24905,0.12);
#9099=CIRCLE('',#24907,0.12);
#9100=CIRCLE('',#24909,0.145);
#9101=CIRCLE('',#24912,0.12);
#9102=CIRCLE('',#24914,0.12);
#9103=CIRCLE('',#24916,0.145);
#9104=CIRCLE('',#24919,0.12);
#9105=CIRCLE('',#24921,0.12);
#9106=CIRCLE('',#24923,0.145);
#9107=CIRCLE('',#24926,4.095);
#9108=CIRCLE('',#24927,4.095);
#9109=CIRCLE('',#24931,0.105);
#9110=CIRCLE('',#24933,0.105);
#9111=CIRCLE('',#24935,0.155);
#9112=CIRCLE('',#24937,0.105);
#9113=CIRCLE('',#24939,0.105);
#9114=CIRCLE('',#24941,0.155);
#9115=CIRCLE('',#24943,0.105);
#9116=CIRCLE('',#24945,0.105);
#9117=CIRCLE('',#24947,0.154999999999999);
#9118=CIRCLE('',#24949,0.105);
#9119=CIRCLE('',#24951,0.105);
#9120=CIRCLE('',#24953,0.155);
#9121=CIRCLE('',#24955,0.105);
#9122=CIRCLE('',#24957,0.105);
#9123=CIRCLE('',#24959,0.155);
#9124=CIRCLE('',#24961,0.105);
#9125=CIRCLE('',#24963,0.105);
#9126=CIRCLE('',#24965,0.154999999999999);
#9127=CIRCLE('',#24967,0.105);
#9128=CIRCLE('',#24969,0.105);
#9129=CIRCLE('',#24971,0.154999999999999);
#9130=CIRCLE('',#24973,0.105);
#9131=CIRCLE('',#24975,0.105);
#9132=CIRCLE('',#24977,0.155);
#9133=CIRCLE('',#24979,0.105);
#9134=CIRCLE('',#24981,0.105);
#9135=CIRCLE('',#24983,0.155);
#9136=CIRCLE('',#24985,0.105);
#9137=CIRCLE('',#24987,0.105);
#9138=CIRCLE('',#24989,0.155);
#9139=CIRCLE('',#24991,0.105);
#9140=CIRCLE('',#24993,0.105);
#9141=CIRCLE('',#24995,0.155);
#9142=CIRCLE('',#24997,0.105);
#9143=CIRCLE('',#24999,0.105);
#9144=CIRCLE('',#25001,0.155);
#9145=CIRCLE('',#25003,0.105);
#9146=CIRCLE('',#25005,0.105);
#9147=CIRCLE('',#25007,0.155);
#9148=CIRCLE('',#25009,0.105);
#9149=CIRCLE('',#25011,0.105);
#9150=CIRCLE('',#25013,0.155);
#9151=CIRCLE('',#25015,0.105);
#9152=CIRCLE('',#25017,0.105);
#9153=CIRCLE('',#25019,0.155);
#9154=CIRCLE('',#25021,0.105);
#9155=CIRCLE('',#25023,0.105);
#9156=CIRCLE('',#25025,0.155);
#9157=CIRCLE('',#25027,0.105);
#9158=CIRCLE('',#25029,0.105);
#9159=CIRCLE('',#25031,0.155);
#9160=CIRCLE('',#25033,0.105);
#9161=CIRCLE('',#25035,0.105);
#9162=CIRCLE('',#25037,0.154999999999999);
#9163=CIRCLE('',#25039,4.13);
#9164=CIRCLE('',#25040,4.1);
#9165=CIRCLE('',#25041,4.1);
#9166=CIRCLE('',#25043,4.1);
#9167=CIRCLE('',#25044,4.1);
#9168=CIRCLE('',#25046,4.56);
#9169=CIRCLE('',#25048,4.13);
#9170=CIRCLE('',#25050,4.56);
#9171=CIRCLE('',#25052,4.6);
#9172=CIRCLE('',#25053,4.6);
#9173=CIRCLE('',#25055,4.6);
#9174=CIRCLE('',#25056,4.6);
#9175=CIRCLE('',#25060,0.105);
#9176=CIRCLE('',#25062,0.105);
#9177=CIRCLE('',#25064,0.155);
#9178=CIRCLE('',#25066,0.105);
#9179=CIRCLE('',#25068,0.105);
#9180=CIRCLE('',#25070,0.155);
#9181=CIRCLE('',#25072,0.13);
#9182=CIRCLE('',#25074,0.13);
#9183=CIRCLE('',#25076,0.180000000000001);
#9184=CIRCLE('',#25078,0.13);
#9185=CIRCLE('',#25080,0.13);
#9186=CIRCLE('',#25082,0.18);
#9187=CIRCLE('',#25084,0.13);
#9188=CIRCLE('',#25086,0.13);
#9189=CIRCLE('',#25088,0.18);
#9190=CIRCLE('',#25090,0.128333333333333);
#9191=CIRCLE('',#25091,0.12);
#9192=CIRCLE('',#25093,0.12);
#9193=CIRCLE('',#25095,0.145);
#9194=CIRCLE('',#25097,0.21);
#9195=CIRCLE('',#25099,0.21);
#9196=CIRCLE('',#25101,0.128333333333333);
#9197=CIRCLE('',#25102,0.12);
#9198=CIRCLE('',#25104,0.12);
#9199=CIRCLE('',#25106,0.145);
#9200=CIRCLE('',#25108,0.21);
#9201=CIRCLE('',#25110,0.21);
#9202=CIRCLE('',#25112,0.128333333333333);
#9203=CIRCLE('',#25113,0.12);
#9204=CIRCLE('',#25115,0.12);
#9205=CIRCLE('',#25117,0.145);
#9206=CIRCLE('',#25119,0.21);
#9207=CIRCLE('',#25121,0.21);
#9208=CIRCLE('',#25123,0.128333333333333);
#9209=CIRCLE('',#25124,0.12);
#9210=CIRCLE('',#25126,0.12);
#9211=CIRCLE('',#25128,0.145);
#9212=CIRCLE('',#25130,0.21);
#9213=CIRCLE('',#25132,0.21);
#9214=CIRCLE('',#25134,0.128333333333333);
#9215=CIRCLE('',#25135,0.12);
#9216=CIRCLE('',#25137,0.12);
#9217=CIRCLE('',#25139,0.145);
#9218=CIRCLE('',#25141,0.21);
#9219=CIRCLE('',#25143,0.21);
#9220=CIRCLE('',#25145,0.128333333333333);
#9221=CIRCLE('',#25146,0.120000000000001);
#9222=CIRCLE('',#25148,0.120000000000001);
#9223=CIRCLE('',#25150,0.145);
#9224=CIRCLE('',#25152,0.21);
#9225=CIRCLE('',#25154,0.21);
#9226=CIRCLE('',#25156,0.128333333333333);
#9227=CIRCLE('',#25157,0.12);
#9228=CIRCLE('',#25159,0.12);
#9229=CIRCLE('',#25161,0.145);
#9230=CIRCLE('',#25163,0.21);
#9231=CIRCLE('',#25165,0.21);
#9232=CIRCLE('',#25167,0.128333333333332);
#9233=CIRCLE('',#25168,0.12);
#9234=CIRCLE('',#25170,0.12);
#9235=CIRCLE('',#25172,0.145);
#9236=CIRCLE('',#25174,0.21);
#9237=CIRCLE('',#25176,0.21);
#9238=CIRCLE('',#25178,0.128333333333333);
#9239=CIRCLE('',#25179,0.12);
#9240=CIRCLE('',#25181,0.12);
#9241=CIRCLE('',#25183,0.145);
#9242=CIRCLE('',#25185,0.21);
#9243=CIRCLE('',#25187,0.21);
#9244=CIRCLE('',#25189,0.128333333333333);
#9245=CIRCLE('',#25190,0.12);
#9246=CIRCLE('',#25192,0.12);
#9247=CIRCLE('',#25194,0.145);
#9248=CIRCLE('',#25196,0.21);
#9249=CIRCLE('',#25198,0.21);
#9250=CIRCLE('',#25200,0.128333333333333);
#9251=CIRCLE('',#25201,0.12);
#9252=CIRCLE('',#25203,0.12);
#9253=CIRCLE('',#25205,0.145);
#9254=CIRCLE('',#25207,0.21);
#9255=CIRCLE('',#25209,0.21);
#9256=CIRCLE('',#25211,0.128333333333333);
#9257=CIRCLE('',#25212,0.12);
#9258=CIRCLE('',#25214,0.12);
#9259=CIRCLE('',#25216,0.145);
#9260=CIRCLE('',#25218,0.21);
#9261=CIRCLE('',#25220,0.21);
#9262=CIRCLE('',#25222,0.74);
#9263=CIRCLE('',#25223,0.7);
#9264=CIRCLE('',#25224,0.7);
#9265=CIRCLE('',#25226,0.7);
#9266=CIRCLE('',#25227,0.7);
#9267=CIRCLE('',#25229,3.8);
#9268=CIRCLE('',#25231,0.74);
#9269=CIRCLE('',#25233,0.9025);
#9270=CIRCLE('',#25235,4.6);
#9271=CIRCLE('',#25236,4.6);
#9272=CIRCLE('',#25237,4.57);
#9273=CIRCLE('',#25239,4.6);
#9274=CIRCLE('',#25240,4.6);
#9275=CIRCLE('',#25242,4.095);
#9276=CIRCLE('',#25244,4.57);
#9277=CIRCLE('',#25246,0.12);
#9278=CIRCLE('',#25247,4.);
#9279=CIRCLE('',#25248,0.12);
#9280=CIRCLE('',#25249,4.);
#9281=CIRCLE('',#25250,0.12);
#9282=CIRCLE('',#25251,0.12);
#9283=CIRCLE('',#25252,0.12);
#9284=CIRCLE('',#25253,0.12);
#9285=CIRCLE('',#25254,4.);
#9286=CIRCLE('',#25255,4.);
#9287=CIRCLE('',#25256,0.12);
#9288=CIRCLE('',#25257,0.12);
#9289=CIRCLE('',#25258,0.12);
#9290=CIRCLE('',#25259,4.);
#9291=CIRCLE('',#25260,0.12);
#9292=CIRCLE('',#25261,4.);
#9293=CIRCLE('',#25262,0.12);
#9294=CIRCLE('',#25263,0.12);
#9295=CIRCLE('',#25264,0.12);
#9296=CIRCLE('',#25265,0.12);
#9297=CIRCLE('',#25266,4.);
#9298=CIRCLE('',#25267,4.);
#9299=CIRCLE('',#25268,0.12);
#9300=CIRCLE('',#25269,0.12);
#9301=CIRCLE('',#25270,0.12);
#9302=CIRCLE('',#25271,4.);
#9303=CIRCLE('',#25272,0.12);
#9304=CIRCLE('',#25273,4.);
#9305=CIRCLE('',#25274,0.12);
#9306=CIRCLE('',#25275,0.12);
#9307=CIRCLE('',#25276,0.12);
#9308=CIRCLE('',#25277,0.12);
#9309=CIRCLE('',#25278,4.);
#9310=CIRCLE('',#25279,4.);
#9311=CIRCLE('',#25280,0.12);
#9312=CIRCLE('',#25281,0.12);
#9313=CIRCLE('',#25282,0.12);
#9314=CIRCLE('',#25283,0.12);
#9315=CIRCLE('',#25284,0.12);
#9316=CIRCLE('',#25285,0.12);
#9317=CIRCLE('',#25286,0.12);
#9318=CIRCLE('',#25287,0.12);
#9319=CIRCLE('',#25288,0.12);
#9320=CIRCLE('',#25289,0.12);
#9321=CIRCLE('',#25290,0.12);
#9322=CIRCLE('',#25291,0.12);
#9323=CIRCLE('',#25292,0.12);
#9324=CIRCLE('',#25293,0.12);
#9325=CIRCLE('',#25294,0.12);
#9326=CIRCLE('',#25295,0.12);
#9327=CIRCLE('',#25296,0.12);
#9328=CIRCLE('',#25297,0.12);
#9329=CIRCLE('',#25298,0.12);
#9330=CIRCLE('',#25299,0.12);
#9331=CIRCLE('',#25300,0.12);
#9332=CIRCLE('',#25301,0.12);
#9333=CIRCLE('',#25302,0.12);
#9334=CIRCLE('',#25303,0.12);
#9335=CIRCLE('',#25304,0.12);
#9336=CIRCLE('',#25305,0.12);
#9337=CIRCLE('',#25306,0.12);
#9338=CIRCLE('',#25307,0.12);
#9339=CIRCLE('',#25308,0.12);
#9340=CIRCLE('',#25309,0.12);
#9341=CIRCLE('',#25310,0.12);
#9342=CIRCLE('',#25311,0.12);
#9343=CIRCLE('',#25312,0.12);
#9344=CIRCLE('',#25313,0.12);
#9345=CIRCLE('',#25314,0.12);
#9346=CIRCLE('',#25315,0.12);
#9347=CIRCLE('',#25316,0.12);
#9348=CIRCLE('',#25317,0.12);
#9349=CIRCLE('',#25318,0.12);
#9350=CIRCLE('',#25319,0.12);
#9351=CIRCLE('',#25320,0.12);
#9352=CIRCLE('',#25321,0.12);
#9353=CIRCLE('',#25322,0.12);
#9354=CIRCLE('',#25323,0.12);
#9355=CIRCLE('',#25324,0.12);
#9356=CIRCLE('',#25325,0.12);
#9357=CIRCLE('',#25326,0.12);
#9358=CIRCLE('',#25327,0.12);
#9359=CIRCLE('',#25328,0.12);
#9360=CIRCLE('',#25329,0.12);
#9361=CIRCLE('',#25330,0.12);
#9362=CIRCLE('',#25331,0.12);
#9363=CIRCLE('',#25332,0.12);
#9364=CIRCLE('',#25333,0.12);
#9365=CIRCLE('',#25334,0.12);
#9366=CIRCLE('',#25335,0.12);
#9367=CIRCLE('',#25336,0.9025);
#9368=CIRCLE('',#25338,0.12);
#9369=CIRCLE('',#25340,0.12);
#9370=CIRCLE('',#25343,0.12);
#9371=CIRCLE('',#25345,4.);
#9372=CIRCLE('',#25347,0.12);
#9373=CIRCLE('',#25350,0.12);
#9374=CIRCLE('',#25352,0.12);
#9375=CIRCLE('',#25356,0.12);
#9376=CIRCLE('',#25359,0.12);
#9377=CIRCLE('',#25361,0.12);
#9378=CIRCLE('',#25365,0.12);
#9379=CIRCLE('',#25367,0.12);
#9380=CIRCLE('',#25370,0.12);
#9381=CIRCLE('',#25372,0.12);
#9382=CIRCLE('',#25376,0.12);
#9383=CIRCLE('',#25379,0.12);
#9384=CIRCLE('',#25381,0.12);
#9385=CIRCLE('',#25385,0.12);
#9386=CIRCLE('',#25388,0.12);
#9387=CIRCLE('',#25390,0.12);
#9388=CIRCLE('',#25391,4.);
#9389=CIRCLE('',#25395,0.12);
#9390=CIRCLE('',#25398,0.12);
#9391=CIRCLE('',#25400,0.12);
#9392=CIRCLE('',#25404,0.12);
#9393=CIRCLE('',#25407,0.12);
#9394=CIRCLE('',#25409,0.12);
#9395=CIRCLE('',#25413,0.12);
#9396=CIRCLE('',#25415,0.12);
#9397=CIRCLE('',#25416,4.);
#9398=CIRCLE('',#25421,0.12);
#9399=CIRCLE('',#25424,0.12);
#9400=CIRCLE('',#25426,0.12);
#9401=CIRCLE('',#25430,0.12);
#9402=CIRCLE('',#25433,0.12);
#9403=CIRCLE('',#25435,0.12);
#9404=CIRCLE('',#25439,0.12);
#9405=CIRCLE('',#25442,0.12);
#9406=CIRCLE('',#25444,0.12);
#9407=CIRCLE('',#25445,4.);
#9408=CIRCLE('',#25449,0.12);
#9409=CIRCLE('',#25452,0.12);
#9410=CIRCLE('',#25454,0.12);
#9411=CIRCLE('',#25458,0.12);
#9412=CIRCLE('',#25461,0.12);
#9413=CIRCLE('',#25463,0.12);
#9414=CIRCLE('',#25467,0.12);
#9415=CIRCLE('',#25470,0.12);
#9416=CIRCLE('',#25472,0.12);
#9417=CIRCLE('',#25476,0.12);
#9418=CIRCLE('',#25478,0.12);
#9419=CIRCLE('',#25481,0.12);
#9420=CIRCLE('',#25483,0.12);
#9421=CIRCLE('',#25487,0.12);
#9422=CIRCLE('',#25490,0.12);
#9423=CIRCLE('',#25492,0.12);
#9424=CIRCLE('',#25496,0.12);
#9425=CIRCLE('',#25498,0.12);
#9426=CIRCLE('',#25499,4.);
#9427=CIRCLE('',#25504,0.12);
#9428=CIRCLE('',#25507,0.12);
#9429=CIRCLE('',#25509,0.12);
#9430=CIRCLE('',#25513,0.12);
#9431=CIRCLE('',#25516,0.12);
#9432=CIRCLE('',#25518,0.12);
#9433=CIRCLE('',#25522,0.12);
#9434=CIRCLE('',#25524,0.12);
#9435=CIRCLE('',#25526,4.);
#9436=CIRCLE('',#25529,0.12);
#9437=CIRCLE('',#25532,0.12);
#9438=CIRCLE('',#25534,0.12);
#9439=CIRCLE('',#25538,0.12);
#9440=CIRCLE('',#25541,0.12);
#9441=CIRCLE('',#25543,0.12);
#9442=CIRCLE('',#25547,0.12);
#9443=CIRCLE('',#25550,0.12);
#9444=CIRCLE('',#25552,0.12);
#9445=CIRCLE('',#25556,0.12);
#9446=CIRCLE('',#25558,4.);
#9447=CIRCLE('',#25561,0.12);
#9448=CIRCLE('',#25564,0.12);
#9449=CIRCLE('',#25566,4.);
#9450=CIRCLE('',#25568,0.12);
#9451=CIRCLE('',#25570,4.);
#9452=CIRCLE('',#25573,0.12);
#9453=CIRCLE('',#25575,4.);
#9454=CIRCLE('',#25577,0.12);
#9455=CIRCLE('',#25579,4.);
#9456=CIRCLE('',#25582,0.12);
#9457=CIRCLE('',#25584,4.);
#9458=CIRCLE('',#25626,3.8);
#9459=CIRCLE('',#25628,4.095);
#9460=CIRCLE('',#25633,1.02);
#9461=CIRCLE('',#25634,1.05);
#9462=CIRCLE('',#25635,1.05);
#9463=CIRCLE('',#25637,1.05);
#9464=CIRCLE('',#25638,1.05);
#9465=CIRCLE('',#25640,0.9);
#9466=CIRCLE('',#25642,1.02);
#9467=CIRCLE('',#25644,0.9);
#9468=CIRCLE('',#25646,0.628786796564401);
#9469=CIRCLE('',#25647,0.679999999999998);
#9470=CIRCLE('',#25649,0.621213203435595);
#9471=CIRCLE('',#25651,1.1);
#9472=CIRCLE('',#25653,0.6);
#9473=CIRCLE('',#25654,0.6);
#9474=CIRCLE('',#25656,0.6);
#9475=CIRCLE('',#25657,0.6);
#9476=CIRCLE('',#25659,0.621213203435596);
#9477=CIRCLE('',#25661,0.628786796564403);
#9478=CIRCLE('',#25663,0.68);
#9479=CIRCLE('',#25665,0.86);
#9480=CIRCLE('',#25667,0.9);
#9481=CIRCLE('',#25668,0.9);
#9482=CIRCLE('',#25671,0.1);
#9483=CIRCLE('',#25672,1.2);
#9484=CIRCLE('',#25674,1.2);
#9485=CIRCLE('',#25676,0.1);
#9486=CIRCLE('',#25677,1.18);
#9487=CIRCLE('',#25679,0.9);
#9488=CIRCLE('',#25683,1.095);
#9489=CIRCLE('',#25684,1.065);
#9490=CIRCLE('',#25685,1.065);
#9491=CIRCLE('',#25687,1.47);
#9492=CIRCLE('',#25688,0.128333333333334);
#9493=CIRCLE('',#25689,0.128333333333334);
#9494=CIRCLE('',#25691,1.065);
#9495=CIRCLE('',#25693,1.5212132034356);
#9496=CIRCLE('',#25695,1.5287867965644);
#9497=CIRCLE('',#25697,1.55);
#9498=CIRCLE('',#25698,1.55);
#9499=CIRCLE('',#25700,1.55);
#9500=CIRCLE('',#25701,1.55);
#9501=CIRCLE('',#25703,1.5287867965644);
#9502=CIRCLE('',#25705,1.5212132034356);
#9503=CIRCLE('',#25707,0.94);
#9504=CIRCLE('',#25708,0.91);
#9505=CIRCLE('',#25709,0.91);
#9506=CIRCLE('',#25711,0.91);
#9507=CIRCLE('',#25712,0.91);
#9508=CIRCLE('',#25715,1.47);
#9509=CIRCLE('',#25716,1.47);
#9510=CIRCLE('',#25717,1.47);
#9511=CIRCLE('',#25719,0.24);
#9512=CIRCLE('',#25720,0.21);
#9513=CIRCLE('',#25721,0.21);
#9514=CIRCLE('',#25722,0.24);
#9515=CIRCLE('',#25724,0.21);
#9516=CIRCLE('',#25726,0.24);
#9517=CIRCLE('',#25727,0.21);
#9518=CIRCLE('',#25728,0.21);
#9519=CIRCLE('',#25729,0.24);
#9520=CIRCLE('',#25731,0.21);
#9521=CIRCLE('',#25733,0.12);
#9522=CIRCLE('',#25735,0.12);
#9523=CIRCLE('',#25737,0.145);
#9524=CIRCLE('',#25740,0.12);
#9525=CIRCLE('',#25742,0.12);
#9526=CIRCLE('',#25744,0.145);
#9527=CIRCLE('',#25747,0.95);
#9528=CIRCLE('',#25751,0.45);
#9529=CIRCLE('',#25752,0.45);
#9530=CIRCLE('',#25754,0.45);
#9531=CIRCLE('',#25755,0.45);
#9532=CIRCLE('',#25757,0.13);
#9533=CIRCLE('',#25758,0.13);
#9534=CIRCLE('',#25760,0.18);
#9535=CIRCLE('',#25762,0.145);
#9536=CIRCLE('',#25763,0.145);
#9537=CIRCLE('',#25765,0.145);
#9538=CIRCLE('',#25766,0.145);
#9539=CIRCLE('',#25768,0.145);
#9540=CIRCLE('',#25769,0.145);
#9541=CIRCLE('',#25771,0.0950000000000001);
#9542=CIRCLE('',#25772,0.0950000000000001);
#9543=CIRCLE('',#25774,0.095);
#9544=CIRCLE('',#25775,0.095);
#9545=CIRCLE('',#25777,0.305);
#9546=CIRCLE('',#25778,0.305);
#9547=CIRCLE('',#25780,0.83);
#9548=CIRCLE('',#25781,0.8);
#9549=CIRCLE('',#25782,0.8);
#9550=CIRCLE('',#25784,0.8);
#9551=CIRCLE('',#25785,0.8);
#9552=CIRCLE('',#25787,3.97);
#9553=CIRCLE('',#25789,0.83);
#9554=CIRCLE('',#25791,3.97);
#9555=CIRCLE('',#25793,4.);
#9556=CIRCLE('',#25794,4.);
#9557=CIRCLE('',#25796,4.);
#9558=CIRCLE('',#25797,4.);
#9559=CIRCLE('',#25801,0.085);
#9560=CIRCLE('',#25803,0.085);
#9561=CIRCLE('',#25805,0.085);
#9562=CIRCLE('',#25807,0.085);
#9563=CIRCLE('',#25809,0.14);
#9564=CIRCLE('',#25810,0.14);
#9565=CIRCLE('',#25813,0.5);
#9566=CIRCLE('',#25815,0.54);
#9567=CIRCLE('',#25817,0.54);
#9568=CIRCLE('',#25819,0.78);
#9569=CIRCLE('',#25820,0.78);
#9570=CIRCLE('',#25822,0.8);
#9571=CIRCLE('',#25824,0.8);
#9572=CIRCLE('',#25826,0.8);
#9573=CIRCLE('',#25828,0.76);
#9574=CIRCLE('',#25830,0.8);
#9575=CIRCLE('',#25833,0.76);
#9576=CIRCLE('',#25835,0.3);
#9577=CIRCLE('',#25837,0.3);
#9578=CIRCLE('',#25839,0.1);
#9579=CIRCLE('',#25841,0.1);
#9580=CIRCLE('',#25843,0.08);
#9581=CIRCLE('',#25847,0.17);
#9582=CIRCLE('',#25848,0.2);
#9583=CIRCLE('',#25849,0.2);
#9584=CIRCLE('',#25851,0.13);
#9585=CIRCLE('',#25853,0.2);
#9586=CIRCLE('',#25855,0.1);
#9587=CIRCLE('',#25856,0.1);
#9588=CIRCLE('',#25858,0.1);
#9589=CIRCLE('',#25859,0.1);
#9590=CIRCLE('',#25861,0.13);
#9591=CIRCLE('',#25863,0.38);
#9592=CIRCLE('',#25865,0.4);
#9593=CIRCLE('',#25866,0.4);
#9594=CIRCLE('',#25869,0.105);
#9595=CIRCLE('',#25870,0.105);
#9596=CIRCLE('',#25871,0.105);
#9597=CIRCLE('',#25873,0.115);
#9598=CIRCLE('',#25874,0.085);
#9599=CIRCLE('',#25876,0.085);
#9600=CIRCLE('',#25878,0.68);
#9601=CIRCLE('',#25879,0.115);
#9602=CIRCLE('',#25880,0.115);
#9603=CIRCLE('',#25882,0.115);
#9604=CIRCLE('',#25884,0.68);
#9605=CIRCLE('',#25885,0.115);
#9606=CIRCLE('',#25886,0.115);
#9607=CIRCLE('',#25888,0.085);
#9608=CIRCLE('',#25890,0.085);
#9609=CIRCLE('',#25893,0.085);
#9610=CIRCLE('',#25895,0.085);
#9611=CIRCLE('',#25900,0.7);
#9612=CIRCLE('',#25901,0.7);
#9613=CIRCLE('',#25903,0.7);
#9614=CIRCLE('',#25904,0.7);
#9615=CIRCLE('',#25908,0.2325);
#9616=CIRCLE('',#25909,0.2025);
#9617=CIRCLE('',#25910,0.2025);
#9618=CIRCLE('',#25912,0.2025);
#9619=CIRCLE('',#25913,0.2025);
#9620=CIRCLE('',#25915,0.12);
#9621=CIRCLE('',#25916,0.67);
#9622=CIRCLE('',#25917,0.12);
#9623=CIRCLE('',#25918,0.12);
#9624=CIRCLE('',#25919,0.67);
#9625=CIRCLE('',#25920,0.12);
#9626=CIRCLE('',#25921,0.12);
#9627=CIRCLE('',#25922,0.67);
#9628=CIRCLE('',#25923,0.12);
#9629=CIRCLE('',#25925,0.2325);
#9630=CIRCLE('',#25927,0.68);
#9631=CIRCLE('',#25928,0.12);
#9632=CIRCLE('',#25929,0.12);
#9633=CIRCLE('',#25930,0.12);
#9634=CIRCLE('',#25932,0.7);
#9635=CIRCLE('',#25933,0.7);
#9636=CIRCLE('',#25935,0.7);
#9637=CIRCLE('',#25936,0.7);
#9638=CIRCLE('',#25938,0.09);
#9639=CIRCLE('',#25940,0.09);
#9640=CIRCLE('',#25943,0.09);
#9641=CIRCLE('',#25945,0.09);
#9642=CIRCLE('',#25948,0.09);
#9643=CIRCLE('',#25950,0.09);
#9644=CIRCLE('',#25958,2.35);
#9645=CIRCLE('',#25959,0.09);
#9646=CIRCLE('',#25960,0.0900000000000001);
#9647=CIRCLE('',#25961,0.2025);
#9648=CIRCLE('',#25962,2.15);
#9649=CIRCLE('',#25963,1.1);
#9650=CIRCLE('',#25964,2.15);
#9651=CIRCLE('',#25965,1.1);
#9652=CIRCLE('',#25966,2.15);
#9653=CIRCLE('',#25967,1.1);
#9654=CIRCLE('',#25968,2.15);
#9655=CIRCLE('',#25969,1.1);
#9656=CIRCLE('',#25970,2.15);
#9657=CIRCLE('',#25971,1.1);
#9658=CIRCLE('',#25972,2.15);
#9659=CIRCLE('',#25973,1.1);
#9660=CIRCLE('',#25974,0.09);
#9661=CIRCLE('',#25976,2.35);
#9662=CIRCLE('',#25978,0.09);
#9663=CIRCLE('',#25980,0.09);
#9664=CIRCLE('',#25982,0.0900000000000001);
#9665=CIRCLE('',#25985,1.1);
#9666=CIRCLE('',#25988,2.15);
#9667=CIRCLE('',#25991,1.1);
#9668=CIRCLE('',#25994,2.15);
#9669=CIRCLE('',#25997,1.1);
#9670=CIRCLE('',#26000,2.15);
#9671=CIRCLE('',#26003,1.1);
#9672=CIRCLE('',#26006,2.15);
#9673=CIRCLE('',#26009,1.1);
#9674=CIRCLE('',#26012,2.15);
#9675=CIRCLE('',#26015,1.1);
#9676=CIRCLE('',#26018,2.15);
#9677=CIRCLE('',#26020,0.2025);
#9678=CIRCLE('',#26038,0.09);
#9679=CIRCLE('',#26039,0.0900000000000001);
#9680=CIRCLE('',#26043,0.0900000000000001);
#9681=CIRCLE('',#26045,0.09);
#9682=CIRCLE('',#26064,0.15);
#9683=CIRCLE('',#26065,0.15);
#9684=CIRCLE('',#26067,0.15);
#9685=CIRCLE('',#26068,0.145);
#9686=CIRCLE('',#26069,0.145);
#9687=CIRCLE('',#26070,0.145);
#9688=CIRCLE('',#26073,0.15);
#9689=CIRCLE('',#26075,0.085);
#9690=CIRCLE('',#26076,0.085);
#9691=CIRCLE('',#26078,0.085);
#9692=CIRCLE('',#26079,0.085);
#9693=CIRCLE('',#26082,0.145);
#9694=CIRCLE('',#26085,0.145);
#9695=CIRCLE('',#26086,0.145);
#9696=CIRCLE('',#26089,0.06);
#9697=CIRCLE('',#26090,0.06);
#9698=CIRCLE('',#26111,0.3);
#9699=CIRCLE('',#26112,0.3);
#9700=CIRCLE('',#26135,0.135);
#9701=CIRCLE('',#26136,0.135);
#9702=CIRCLE('',#26138,0.135);
#9703=CIRCLE('',#26139,0.135);
#9704=CIRCLE('',#26141,0.135);
#9705=CIRCLE('',#26142,0.135);
#9706=CIRCLE('',#26144,0.8);
#9707=CIRCLE('',#26145,0.8);
#9708=CIRCLE('',#26147,3.8);
#9709=CIRCLE('',#26149,3.8);
#9710=CIRCLE('',#26153,0.096675);
#9711=CIRCLE('',#26154,0.096675);
#9712=CIRCLE('',#26158,0.0739);
#9713=CIRCLE('',#26163,0.096675);
#9714=CIRCLE('',#26164,0.096675);
#9715=CIRCLE('',#26166,0.0739);
#9716=CIRCLE('',#26169,0.096675);
#9717=CIRCLE('',#26171,0.0400285208940887);
#9718=CIRCLE('',#26180,0.07);
#9719=CIRCLE('',#26183,0.08);
#9720=CIRCLE('',#26187,0.1215);
#9721=CIRCLE('',#26188,0.1215);
#9722=CIRCLE('',#26189,0.1215);
#9723=CIRCLE('',#26198,0.095825);
#9724=CIRCLE('',#26207,0.095825);
#9725=CIRCLE('',#26210,0.1215);
#9726=CIRCLE('',#26212,0.13);
#9727=CIRCLE('',#26214,0.13);
#9728=CIRCLE('',#26216,0.18);
#9729=CIRCLE('',#26218,0.255);
#9730=CIRCLE('',#26220,0.255);
#9731=CIRCLE('',#26222,0.255);
#9732=CIRCLE('',#26224,0.255);
#9733=CIRCLE('',#26226,0.255);
#9734=CIRCLE('',#26228,0.255);
#9735=CIRCLE('',#26235,0.255);
#9736=CIRCLE('',#26237,0.255);
#9737=CIRCLE('',#26239,0.255);
#9738=CIRCLE('',#26241,0.255);
#9739=CIRCLE('',#26243,0.255);
#9740=CIRCLE('',#26245,0.255);
#9741=CIRCLE('',#26248,0.105);
#9742=CIRCLE('',#26254,0.096675);
#9743=CIRCLE('',#26255,0.096675);
#9744=CIRCLE('',#26256,0.096675);
#9745=CIRCLE('',#26285,0.0739);
#9746=CIRCLE('',#26314,0.0739);
#9747=CIRCLE('',#26316,0.096675);
#9748=CIRCLE('',#26317,0.096675);
#9749=CIRCLE('',#26319,0.0739);
#9750=CIRCLE('',#26322,0.19);
#9751=CIRCLE('',#26326,0.19);
#9752=CIRCLE('',#26330,0.19);
#9753=CIRCLE('',#26334,0.19);
#9754=CIRCLE('',#26338,0.19);
#9755=CIRCLE('',#26342,0.19);
#9756=CIRCLE('',#26346,0.19);
#9757=CIRCLE('',#26350,0.19);
#9758=CIRCLE('',#26354,0.19);
#9759=CIRCLE('',#26358,0.19);
#9760=CIRCLE('',#26362,0.19);
#9761=CIRCLE('',#26366,0.19);
#9762=CIRCLE('',#26370,0.19);
#9763=CIRCLE('',#26374,0.19);
#9764=CIRCLE('',#26378,0.19);
#9765=CIRCLE('',#26382,0.19);
#9766=CIRCLE('',#26386,0.19);
#9767=CIRCLE('',#26390,0.19);
#9768=CIRCLE('',#26391,0.19);
#9769=CIRCLE('',#26395,0.19);
#9770=CIRCLE('',#26399,0.19);
#9771=CIRCLE('',#26403,0.19);
#9772=CIRCLE('',#26407,0.19);
#9773=CIRCLE('',#26411,0.19);
#9774=CIRCLE('',#26415,0.19);
#9775=CIRCLE('',#26419,0.19);
#9776=CIRCLE('',#26423,0.19);
#9777=CIRCLE('',#26427,0.19);
#9778=CIRCLE('',#26431,0.19);
#9779=CIRCLE('',#26435,0.19);
#9780=CIRCLE('',#26439,0.19);
#9781=CIRCLE('',#26443,0.19);
#9782=CIRCLE('',#26447,0.19);
#9783=CIRCLE('',#26451,0.19);
#9784=CIRCLE('',#26455,0.19);
#9785=CIRCLE('',#26459,0.19);
#9786=CIRCLE('',#26463,0.19);
#9787=CIRCLE('',#26464,0.19);
#9788=CIRCLE('',#26465,0.19);
#9789=CIRCLE('',#26466,0.19);
#9790=CIRCLE('',#26467,0.19);
#9791=CIRCLE('',#26468,0.19);
#9792=CIRCLE('',#26469,0.19);
#9793=CIRCLE('',#26470,0.19);
#9794=CIRCLE('',#26471,0.19);
#9795=CIRCLE('',#26472,0.19);
#9796=CIRCLE('',#26473,0.19);
#9797=CIRCLE('',#26474,0.19);
#9798=CIRCLE('',#26475,0.19);
#9799=CIRCLE('',#26476,0.19);
#9800=CIRCLE('',#26477,0.19);
#9801=CIRCLE('',#26478,0.19);
#9802=CIRCLE('',#26479,0.19);
#9803=CIRCLE('',#26480,0.19);
#9804=CIRCLE('',#26481,0.19);
#9805=CIRCLE('',#26482,0.19);
#9806=CIRCLE('',#26483,0.19);
#9807=CIRCLE('',#26484,0.19);
#9808=CIRCLE('',#26485,0.19);
#9809=CIRCLE('',#26486,0.19);
#9810=CIRCLE('',#26487,0.19);
#9811=CIRCLE('',#26488,0.19);
#9812=CIRCLE('',#26489,0.19);
#9813=CIRCLE('',#26490,0.19);
#9814=CIRCLE('',#26491,0.19);
#9815=CIRCLE('',#26492,0.19);
#9816=CIRCLE('',#26493,0.19);
#9817=CIRCLE('',#26494,0.19);
#9818=CIRCLE('',#26495,0.19);
#9819=CIRCLE('',#26496,0.19);
#9820=CIRCLE('',#26497,0.19);
#9821=CIRCLE('',#26498,0.19);
#9822=CIRCLE('',#26499,0.19);
#9823=CIRCLE('',#26500,0.19);
#9824=CIRCLE('',#26505,0.175);
#9825=CIRCLE('',#26507,0.0677181486487011);
#9826=CIRCLE('',#26516,0.076);
#9827=CIRCLE('',#26519,0.096675);
#9828=CIRCLE('',#26521,0.11);
#9829=CIRCLE('',#26526,0.096675);
#9830=CIRCLE('',#26527,0.096675);
#9831=CIRCLE('',#26528,0.096675);
#9832=CIRCLE('',#26552,0.0739);
#9833=CIRCLE('',#26576,0.0739);
#9834=CIRCLE('',#26578,0.096675);
#9835=CIRCLE('',#26579,0.096675);
#9836=CIRCLE('',#26581,0.0739);
#9837=CIRCLE('',#26584,0.19);
#9838=CIRCLE('',#26588,0.19);
#9839=CIRCLE('',#26592,0.19);
#9840=CIRCLE('',#26596,0.19);
#9841=CIRCLE('',#26600,0.19);
#9842=CIRCLE('',#26604,0.19);
#9843=CIRCLE('',#26608,0.19);
#9844=CIRCLE('',#26612,0.19);
#9845=CIRCLE('',#26616,0.19);
#9846=CIRCLE('',#26620,0.19);
#9847=CIRCLE('',#26624,0.19);
#9848=CIRCLE('',#26628,0.19);
#9849=CIRCLE('',#26632,0.19);
#9850=CIRCLE('',#26636,0.19);
#9851=CIRCLE('',#26640,0.19);
#9852=CIRCLE('',#26644,0.19);
#9853=CIRCLE('',#26648,0.19);
#9854=CIRCLE('',#26652,0.19);
#9855=CIRCLE('',#26653,0.19);
#9856=CIRCLE('',#26657,0.19);
#9857=CIRCLE('',#26661,0.19);
#9858=CIRCLE('',#26665,0.19);
#9859=CIRCLE('',#26669,0.19);
#9860=CIRCLE('',#26673,0.19);
#9861=CIRCLE('',#26677,0.19);
#9862=CIRCLE('',#26681,0.19);
#9863=CIRCLE('',#26685,0.19);
#9864=CIRCLE('',#26689,0.19);
#9865=CIRCLE('',#26693,0.19);
#9866=CIRCLE('',#26697,0.19);
#9867=CIRCLE('',#26701,0.19);
#9868=CIRCLE('',#26705,0.19);
#9869=CIRCLE('',#26709,0.19);
#9870=CIRCLE('',#26713,0.19);
#9871=CIRCLE('',#26717,0.19);
#9872=CIRCLE('',#26721,0.19);
#9873=CIRCLE('',#26725,0.19);
#9874=CIRCLE('',#26726,0.19);
#9875=CIRCLE('',#26727,0.19);
#9876=CIRCLE('',#26728,0.19);
#9877=CIRCLE('',#26729,0.19);
#9878=CIRCLE('',#26730,0.19);
#9879=CIRCLE('',#26731,0.19);
#9880=CIRCLE('',#26732,0.19);
#9881=CIRCLE('',#26733,0.19);
#9882=CIRCLE('',#26734,0.19);
#9883=CIRCLE('',#26735,0.19);
#9884=CIRCLE('',#26736,0.19);
#9885=CIRCLE('',#26737,0.19);
#9886=CIRCLE('',#26738,0.19);
#9887=CIRCLE('',#26739,0.19);
#9888=CIRCLE('',#26740,0.19);
#9889=CIRCLE('',#26741,0.19);
#9890=CIRCLE('',#26742,0.19);
#9891=CIRCLE('',#26743,0.19);
#9892=CIRCLE('',#26744,0.19);
#9893=CIRCLE('',#26745,0.19);
#9894=CIRCLE('',#26746,0.19);
#9895=CIRCLE('',#26747,0.19);
#9896=CIRCLE('',#26748,0.19);
#9897=CIRCLE('',#26749,0.19);
#9898=CIRCLE('',#26750,0.19);
#9899=CIRCLE('',#26751,0.19);
#9900=CIRCLE('',#26752,0.19);
#9901=CIRCLE('',#26753,0.19);
#9902=CIRCLE('',#26754,0.19);
#9903=CIRCLE('',#26755,0.19);
#9904=CIRCLE('',#26756,0.19);
#9905=CIRCLE('',#26757,0.19);
#9906=CIRCLE('',#26758,0.19);
#9907=CIRCLE('',#26759,0.19);
#9908=CIRCLE('',#26760,0.19);
#9909=CIRCLE('',#26761,0.19);
#9910=CIRCLE('',#26762,0.19);
#9911=CIRCLE('',#26767,0.175);
#9912=CIRCLE('',#26769,0.0677181486487011);
#9913=CIRCLE('',#26778,0.076);
#9914=CIRCLE('',#26781,0.096675);
#9915=CIRCLE('',#26783,0.11);
#9916=CIRCLE('',#26788,0.1215);
#9917=CIRCLE('',#26789,0.1215);
#9918=CIRCLE('',#26790,0.1215);
#9919=CIRCLE('',#26803,0.095825);
#9920=CIRCLE('',#26815,0.095825);
#9921=CIRCLE('',#26817,0.1215);
#9922=CIRCLE('',#26818,0.1215);
#9923=CIRCLE('',#26820,0.095825);
#9924=CIRCLE('',#26823,0.1215);
#9925=CIRCLE('',#26825,0.225);
#9926=CIRCLE('',#26829,0.225);
#9927=CIRCLE('',#26833,0.225);
#9928=CIRCLE('',#26837,0.225);
#9929=CIRCLE('',#26841,0.225);
#9930=CIRCLE('',#26845,0.225);
#9931=CIRCLE('',#26849,0.225);
#9932=CIRCLE('',#26853,0.225);
#9933=CIRCLE('',#26857,0.225);
#9934=CIRCLE('',#26861,0.225);
#9935=CIRCLE('',#26865,0.225);
#9936=CIRCLE('',#26869,0.225);
#9937=CIRCLE('',#26873,0.225);
#9938=CIRCLE('',#26877,0.225);
#9939=CIRCLE('',#26881,0.225);
#9940=CIRCLE('',#26885,0.225);
#9941=CIRCLE('',#26889,0.225);
#9942=CIRCLE('',#26893,0.225);
#9943=CIRCLE('',#26894,0.225);
#9944=CIRCLE('',#26898,0.225);
#9945=CIRCLE('',#26902,0.225);
#9946=CIRCLE('',#26906,0.225);
#9947=CIRCLE('',#26910,0.225);
#9948=CIRCLE('',#26914,0.225);
#9949=CIRCLE('',#26918,0.225);
#9950=CIRCLE('',#26922,0.225);
#9951=CIRCLE('',#26926,0.225);
#9952=CIRCLE('',#26930,0.225);
#9953=CIRCLE('',#26934,0.225);
#9954=CIRCLE('',#26938,0.225);
#9955=CIRCLE('',#26942,0.225);
#9956=CIRCLE('',#26946,0.225);
#9957=CIRCLE('',#26950,0.225);
#9958=CIRCLE('',#26954,0.225);
#9959=CIRCLE('',#26958,0.225);
#9960=CIRCLE('',#26962,0.225);
#9961=CIRCLE('',#26966,0.225);
#9962=CIRCLE('',#26967,0.225);
#9963=CIRCLE('',#26968,0.225);
#9964=CIRCLE('',#26969,0.225);
#9965=CIRCLE('',#26970,0.225);
#9966=CIRCLE('',#26971,0.225);
#9967=CIRCLE('',#26972,0.225);
#9968=CIRCLE('',#26973,0.225);
#9969=CIRCLE('',#26974,0.225);
#9970=CIRCLE('',#26975,0.225);
#9971=CIRCLE('',#26976,0.225);
#9972=CIRCLE('',#26977,0.225);
#9973=CIRCLE('',#26978,0.225);
#9974=CIRCLE('',#26979,0.225);
#9975=CIRCLE('',#26980,0.225);
#9976=CIRCLE('',#26981,0.225);
#9977=CIRCLE('',#26982,0.225);
#9978=CIRCLE('',#26983,0.225);
#9979=CIRCLE('',#26984,0.225);
#9980=CIRCLE('',#26985,0.225);
#9981=CIRCLE('',#26986,0.225);
#9982=CIRCLE('',#26987,0.225);
#9983=CIRCLE('',#26988,0.225);
#9984=CIRCLE('',#26989,0.225);
#9985=CIRCLE('',#26990,0.225);
#9986=CIRCLE('',#26991,0.225);
#9987=CIRCLE('',#26992,0.225);
#9988=CIRCLE('',#26993,0.225);
#9989=CIRCLE('',#26994,0.225);
#9990=CIRCLE('',#26995,0.225);
#9991=CIRCLE('',#26996,0.225);
#9992=CIRCLE('',#26997,0.225);
#9993=CIRCLE('',#26998,0.225);
#9994=CIRCLE('',#26999,0.225);
#9995=CIRCLE('',#27000,0.225);
#9996=CIRCLE('',#27001,0.225);
#9997=CIRCLE('',#27002,0.225);
#9998=CIRCLE('',#27003,0.225);
#9999=CIRCLE('',#27008,0.21);
#10000=CIRCLE('',#27010,0.0908032840555568);
#10001=CIRCLE('',#27019,0.095);
#10002=CIRCLE('',#27022,0.135);
#10003=CIRCLE('',#27027,0.076925);
#10004=CIRCLE('',#27028,0.076925);
#10005=CIRCLE('',#27029,0.076925);
#10006=CIRCLE('',#27037,0.056925);
#10007=CIRCLE('',#27045,0.056925);
#10008=CIRCLE('',#27047,0.056925);
#10009=CIRCLE('',#27056,0.1275);
#10010=CIRCLE('',#27065,0.0608);
#10011=CIRCLE('',#27068,0.076925);
#10012=CIRCLE('',#27070,0.16);
#10013=CIRCLE('',#27072,0.16);
#10014=CIRCLE('',#27076,0.076925);
#10015=CIRCLE('',#27077,0.076925);
#10016=CIRCLE('',#27078,0.076925);
#10017=CIRCLE('',#27095,0.056925);
#10018=CIRCLE('',#27097,0.056925);
#10019=CIRCLE('',#27113,0.056925);
#10020=CIRCLE('',#27115,0.056925);
#10021=CIRCLE('',#27118,0.076925);
#10022=CIRCLE('',#27126,0.1275);
#10023=CIRCLE('',#27135,0.0608);
#10024=CIRCLE('',#27138,0.16);
#10025=CIRCLE('',#27140,0.16);
#10026=VERTEX_POINT('',#33872);
#10027=VERTEX_POINT('',#33874);
#10028=VERTEX_POINT('',#33876);
#10029=VERTEX_POINT('',#33880);
#10030=VERTEX_POINT('',#33884);
#10031=VERTEX_POINT('',#33888);
#10032=VERTEX_POINT('',#33890);
#10033=VERTEX_POINT('',#33894);
#10034=VERTEX_POINT('',#33898);
#10035=VERTEX_POINT('',#33900);
#10036=VERTEX_POINT('',#33902);
#10037=VERTEX_POINT('',#33904);
#10038=VERTEX_POINT('',#33906);
#10039=VERTEX_POINT('',#33908);
#10040=VERTEX_POINT('',#33910);
#10041=VERTEX_POINT('',#33913);
#10042=VERTEX_POINT('',#33917);
#10043=VERTEX_POINT('',#33919);
#10044=VERTEX_POINT('',#33921);
#10045=VERTEX_POINT('',#33923);
#10046=VERTEX_POINT('',#33925);
#10047=VERTEX_POINT('',#33927);
#10048=VERTEX_POINT('',#33929);
#10049=VERTEX_POINT('',#33932);
#10050=VERTEX_POINT('',#33936);
#10051=VERTEX_POINT('',#33940);
#10052=VERTEX_POINT('',#33942);
#10053=VERTEX_POINT('',#33946);
#10054=VERTEX_POINT('',#33947);
#10055=VERTEX_POINT('',#33952);
#10056=VERTEX_POINT('',#33956);
#10057=VERTEX_POINT('',#33960);
#10058=VERTEX_POINT('',#33964);
#10059=VERTEX_POINT('',#33966);
#10060=VERTEX_POINT('',#33968);
#10061=VERTEX_POINT('',#33970);
#10062=VERTEX_POINT('',#33973);
#10063=VERTEX_POINT('',#33975);
#10064=VERTEX_POINT('',#33979);
#10065=VERTEX_POINT('',#33983);
#10066=VERTEX_POINT('',#33985);
#10067=VERTEX_POINT('',#33989);
#10068=VERTEX_POINT('',#33993);
#10069=VERTEX_POINT('',#33995);
#10070=VERTEX_POINT('',#33999);
#10071=VERTEX_POINT('',#34003);
#10072=VERTEX_POINT('',#34005);
#10073=VERTEX_POINT('',#34009);
#10074=VERTEX_POINT('',#34013);
#10075=VERTEX_POINT('',#34015);
#10076=VERTEX_POINT('',#34019);
#10077=VERTEX_POINT('',#34023);
#10078=VERTEX_POINT('',#34025);
#10079=VERTEX_POINT('',#34029);
#10080=VERTEX_POINT('',#34033);
#10081=VERTEX_POINT('',#34035);
#10082=VERTEX_POINT('',#34039);
#10083=VERTEX_POINT('',#34043);
#10084=VERTEX_POINT('',#34047);
#10085=VERTEX_POINT('',#34050);
#10086=VERTEX_POINT('',#34054);
#10087=VERTEX_POINT('',#34059);
#10088=VERTEX_POINT('',#34060);
#10089=VERTEX_POINT('',#34064);
#10090=VERTEX_POINT('',#34070);
#10091=VERTEX_POINT('',#34071);
#10092=VERTEX_POINT('',#34075);
#10093=VERTEX_POINT('',#34081);
#10094=VERTEX_POINT('',#34082);
#10095=VERTEX_POINT('',#34086);
#10096=VERTEX_POINT('',#34092);
#10097=VERTEX_POINT('',#34096);
#10098=VERTEX_POINT('',#34100);
#10099=VERTEX_POINT('',#34105);
#10100=VERTEX_POINT('',#34109);
#10101=VERTEX_POINT('',#34113);
#10102=VERTEX_POINT('',#34118);
#10103=VERTEX_POINT('',#34122);
#10104=VERTEX_POINT('',#34126);
#10105=VERTEX_POINT('',#34131);
#10106=VERTEX_POINT('',#34135);
#10107=VERTEX_POINT('',#34139);
#10108=VERTEX_POINT('',#34144);
#10109=VERTEX_POINT('',#34148);
#10110=VERTEX_POINT('',#34152);
#10111=VERTEX_POINT('',#34157);
#10112=VERTEX_POINT('',#34161);
#10113=VERTEX_POINT('',#34165);
#10114=VERTEX_POINT('',#34170);
#10115=VERTEX_POINT('',#34172);
#10116=VERTEX_POINT('',#34179);
#10117=VERTEX_POINT('',#34180);
#10118=VERTEX_POINT('',#34184);
#10119=VERTEX_POINT('',#34188);
#10120=VERTEX_POINT('',#34192);
#10121=VERTEX_POINT('',#34193);
#10122=VERTEX_POINT('',#34197);
#10123=VERTEX_POINT('',#34201);
#10124=VERTEX_POINT('',#34205);
#10125=VERTEX_POINT('',#34206);
#10126=VERTEX_POINT('',#34210);
#10127=VERTEX_POINT('',#34214);
#10128=VERTEX_POINT('',#34218);
#10129=VERTEX_POINT('',#34219);
#10130=VERTEX_POINT('',#34223);
#10131=VERTEX_POINT('',#34227);
#10132=VERTEX_POINT('',#34231);
#10133=VERTEX_POINT('',#34232);
#10134=VERTEX_POINT('',#34236);
#10135=VERTEX_POINT('',#34240);
#10136=VERTEX_POINT('',#34244);
#10137=VERTEX_POINT('',#34245);
#10138=VERTEX_POINT('',#34249);
#10139=VERTEX_POINT('',#34253);
#10140=VERTEX_POINT('',#34257);
#10141=VERTEX_POINT('',#34258);
#10142=VERTEX_POINT('',#34262);
#10143=VERTEX_POINT('',#34266);
#10144=VERTEX_POINT('',#34270);
#10145=VERTEX_POINT('',#34271);
#10146=VERTEX_POINT('',#34275);
#10147=VERTEX_POINT('',#34279);
#10148=VERTEX_POINT('',#34283);
#10149=VERTEX_POINT('',#34284);
#10150=VERTEX_POINT('',#34288);
#10151=VERTEX_POINT('',#34292);
#10152=VERTEX_POINT('',#34296);
#10153=VERTEX_POINT('',#34297);
#10154=VERTEX_POINT('',#34301);
#10155=VERTEX_POINT('',#34305);
#10156=VERTEX_POINT('',#34309);
#10157=VERTEX_POINT('',#34310);
#10158=VERTEX_POINT('',#34314);
#10159=VERTEX_POINT('',#34318);
#10160=VERTEX_POINT('',#34322);
#10161=VERTEX_POINT('',#34323);
#10162=VERTEX_POINT('',#34327);
#10163=VERTEX_POINT('',#34331);
#10164=VERTEX_POINT('',#34335);
#10165=VERTEX_POINT('',#34336);
#10166=VERTEX_POINT('',#34340);
#10167=VERTEX_POINT('',#34344);
#10168=VERTEX_POINT('',#34348);
#10169=VERTEX_POINT('',#34349);
#10170=VERTEX_POINT('',#34353);
#10171=VERTEX_POINT('',#34357);
#10172=VERTEX_POINT('',#34361);
#10173=VERTEX_POINT('',#34362);
#10174=VERTEX_POINT('',#34366);
#10175=VERTEX_POINT('',#34370);
#10176=VERTEX_POINT('',#34374);
#10177=VERTEX_POINT('',#34375);
#10178=VERTEX_POINT('',#34379);
#10179=VERTEX_POINT('',#34383);
#10180=VERTEX_POINT('',#34387);
#10181=VERTEX_POINT('',#34388);
#10182=VERTEX_POINT('',#34392);
#10183=VERTEX_POINT('',#34396);
#10184=VERTEX_POINT('',#34400);
#10185=VERTEX_POINT('',#34401);
#10186=VERTEX_POINT('',#34405);
#10187=VERTEX_POINT('',#34409);
#10188=VERTEX_POINT('',#34413);
#10189=VERTEX_POINT('',#34415);
#10190=VERTEX_POINT('',#34417);
#10191=VERTEX_POINT('',#34421);
#10192=VERTEX_POINT('',#34422);
#10193=VERTEX_POINT('',#34427);
#10194=VERTEX_POINT('',#34430);
#10195=VERTEX_POINT('',#34434);
#10196=VERTEX_POINT('',#34437);
#10197=VERTEX_POINT('',#34439);
#10198=VERTEX_POINT('',#34443);
#10199=VERTEX_POINT('',#34445);
#10200=VERTEX_POINT('',#34452);
#10201=VERTEX_POINT('',#34453);
#10202=VERTEX_POINT('',#34457);
#10203=VERTEX_POINT('',#34461);
#10204=VERTEX_POINT('',#34465);
#10205=VERTEX_POINT('',#34466);
#10206=VERTEX_POINT('',#34470);
#10207=VERTEX_POINT('',#34474);
#10208=VERTEX_POINT('',#34478);
#10209=VERTEX_POINT('',#34479);
#10210=VERTEX_POINT('',#34483);
#10211=VERTEX_POINT('',#34487);
#10212=VERTEX_POINT('',#34491);
#10213=VERTEX_POINT('',#34492);
#10214=VERTEX_POINT('',#34496);
#10215=VERTEX_POINT('',#34500);
#10216=VERTEX_POINT('',#34504);
#10217=VERTEX_POINT('',#34505);
#10218=VERTEX_POINT('',#34509);
#10219=VERTEX_POINT('',#34513);
#10220=VERTEX_POINT('',#34517);
#10221=VERTEX_POINT('',#34519);
#10222=VERTEX_POINT('',#34523);
#10223=VERTEX_POINT('',#34527);
#10224=VERTEX_POINT('',#34531);
#10225=VERTEX_POINT('',#34534);
#10226=VERTEX_POINT('',#34538);
#10227=VERTEX_POINT('',#34540);
#10228=VERTEX_POINT('',#34544);
#10229=VERTEX_POINT('',#34548);
#10230=VERTEX_POINT('',#34552);
#10231=VERTEX_POINT('',#34555);
#10232=VERTEX_POINT('',#34559);
#10233=VERTEX_POINT('',#34561);
#10234=VERTEX_POINT('',#34565);
#10235=VERTEX_POINT('',#34569);
#10236=VERTEX_POINT('',#34573);
#10237=VERTEX_POINT('',#34576);
#10238=VERTEX_POINT('',#34580);
#10239=VERTEX_POINT('',#34582);
#10240=VERTEX_POINT('',#34586);
#10241=VERTEX_POINT('',#34590);
#10242=VERTEX_POINT('',#34594);
#10243=VERTEX_POINT('',#34597);
#10244=VERTEX_POINT('',#34601);
#10245=VERTEX_POINT('',#34603);
#10246=VERTEX_POINT('',#34607);
#10247=VERTEX_POINT('',#34611);
#10248=VERTEX_POINT('',#34615);
#10249=VERTEX_POINT('',#34618);
#10250=VERTEX_POINT('',#34622);
#10251=VERTEX_POINT('',#34624);
#10252=VERTEX_POINT('',#34628);
#10253=VERTEX_POINT('',#34632);
#10254=VERTEX_POINT('',#34636);
#10255=VERTEX_POINT('',#34639);
#10256=VERTEX_POINT('',#34643);
#10257=VERTEX_POINT('',#34645);
#10258=VERTEX_POINT('',#34649);
#10259=VERTEX_POINT('',#34653);
#10260=VERTEX_POINT('',#34657);
#10261=VERTEX_POINT('',#34660);
#10262=VERTEX_POINT('',#34664);
#10263=VERTEX_POINT('',#34666);
#10264=VERTEX_POINT('',#34670);
#10265=VERTEX_POINT('',#34674);
#10266=VERTEX_POINT('',#34678);
#10267=VERTEX_POINT('',#34681);
#10268=VERTEX_POINT('',#34685);
#10269=VERTEX_POINT('',#34687);
#10270=VERTEX_POINT('',#34691);
#10271=VERTEX_POINT('',#34695);
#10272=VERTEX_POINT('',#34699);
#10273=VERTEX_POINT('',#34702);
#10274=VERTEX_POINT('',#34706);
#10275=VERTEX_POINT('',#34708);
#10276=VERTEX_POINT('',#34712);
#10277=VERTEX_POINT('',#34716);
#10278=VERTEX_POINT('',#34720);
#10279=VERTEX_POINT('',#34723);
#10280=VERTEX_POINT('',#34727);
#10281=VERTEX_POINT('',#34729);
#10282=VERTEX_POINT('',#34733);
#10283=VERTEX_POINT('',#34737);
#10284=VERTEX_POINT('',#34741);
#10285=VERTEX_POINT('',#34744);
#10286=VERTEX_POINT('',#34748);
#10287=VERTEX_POINT('',#34750);
#10288=VERTEX_POINT('',#34754);
#10289=VERTEX_POINT('',#34758);
#10290=VERTEX_POINT('',#34762);
#10291=VERTEX_POINT('',#34765);
#10292=VERTEX_POINT('',#34769);
#10293=VERTEX_POINT('',#34771);
#10294=VERTEX_POINT('',#34773);
#10295=VERTEX_POINT('',#34777);
#10296=VERTEX_POINT('',#34778);
#10297=VERTEX_POINT('',#34783);
#10298=VERTEX_POINT('',#34786);
#10299=VERTEX_POINT('',#34790);
#10300=VERTEX_POINT('',#34793);
#10301=VERTEX_POINT('',#34794);
#10302=VERTEX_POINT('',#34797);
#10303=VERTEX_POINT('',#34801);
#10304=VERTEX_POINT('',#34802);
#10305=VERTEX_POINT('',#34807);
#10306=VERTEX_POINT('',#34810);
#10307=VERTEX_POINT('',#34814);
#10308=VERTEX_POINT('',#34815);
#10309=VERTEX_POINT('',#34817);
#10310=VERTEX_POINT('',#34819);
#10311=VERTEX_POINT('',#34821);
#10312=VERTEX_POINT('',#34824);
#10313=VERTEX_POINT('',#34825);
#10314=VERTEX_POINT('',#34827);
#10315=VERTEX_POINT('',#34829);
#10316=VERTEX_POINT('',#34831);
#10317=VERTEX_POINT('',#34834);
#10318=VERTEX_POINT('',#34835);
#10319=VERTEX_POINT('',#34837);
#10320=VERTEX_POINT('',#34839);
#10321=VERTEX_POINT('',#34841);
#10322=VERTEX_POINT('',#34844);
#10323=VERTEX_POINT('',#34845);
#10324=VERTEX_POINT('',#34847);
#10325=VERTEX_POINT('',#34849);
#10326=VERTEX_POINT('',#34851);
#10327=VERTEX_POINT('',#34854);
#10328=VERTEX_POINT('',#34855);
#10329=VERTEX_POINT('',#34857);
#10330=VERTEX_POINT('',#34859);
#10331=VERTEX_POINT('',#34861);
#10332=VERTEX_POINT('',#34864);
#10333=VERTEX_POINT('',#34865);
#10334=VERTEX_POINT('',#34867);
#10335=VERTEX_POINT('',#34869);
#10336=VERTEX_POINT('',#34871);
#10337=VERTEX_POINT('',#34874);
#10338=VERTEX_POINT('',#34875);
#10339=VERTEX_POINT('',#34877);
#10340=VERTEX_POINT('',#34879);
#10341=VERTEX_POINT('',#34881);
#10342=VERTEX_POINT('',#34884);
#10343=VERTEX_POINT('',#34885);
#10344=VERTEX_POINT('',#34887);
#10345=VERTEX_POINT('',#34889);
#10346=VERTEX_POINT('',#34891);
#10347=VERTEX_POINT('',#34894);
#10348=VERTEX_POINT('',#34895);
#10349=VERTEX_POINT('',#34897);
#10350=VERTEX_POINT('',#34899);
#10351=VERTEX_POINT('',#34901);
#10352=VERTEX_POINT('',#34904);
#10353=VERTEX_POINT('',#34905);
#10354=VERTEX_POINT('',#34907);
#10355=VERTEX_POINT('',#34909);
#10356=VERTEX_POINT('',#34911);
#10357=VERTEX_POINT('',#34914);
#10358=VERTEX_POINT('',#34915);
#10359=VERTEX_POINT('',#34917);
#10360=VERTEX_POINT('',#34919);
#10361=VERTEX_POINT('',#34921);
#10362=VERTEX_POINT('',#34924);
#10363=VERTEX_POINT('',#34925);
#10364=VERTEX_POINT('',#34927);
#10365=VERTEX_POINT('',#34929);
#10366=VERTEX_POINT('',#34931);
#10367=VERTEX_POINT('',#34934);
#10368=VERTEX_POINT('',#34935);
#10369=VERTEX_POINT('',#34937);
#10370=VERTEX_POINT('',#34939);
#10371=VERTEX_POINT('',#34941);
#10372=VERTEX_POINT('',#34943);
#10373=VERTEX_POINT('',#34946);
#10374=VERTEX_POINT('',#34947);
#10375=VERTEX_POINT('',#34949);
#10376=VERTEX_POINT('',#34951);
#10377=VERTEX_POINT('',#34953);
#10378=VERTEX_POINT('',#34955);
#10379=VERTEX_POINT('',#34958);
#10380=VERTEX_POINT('',#34959);
#10381=VERTEX_POINT('',#34961);
#10382=VERTEX_POINT('',#34963);
#10383=VERTEX_POINT('',#34965);
#10384=VERTEX_POINT('',#34967);
#10385=VERTEX_POINT('',#34970);
#10386=VERTEX_POINT('',#34971);
#10387=VERTEX_POINT('',#34973);
#10388=VERTEX_POINT('',#34975);
#10389=VERTEX_POINT('',#34977);
#10390=VERTEX_POINT('',#34979);
#10391=VERTEX_POINT('',#34982);
#10392=VERTEX_POINT('',#34983);
#10393=VERTEX_POINT('',#34985);
#10394=VERTEX_POINT('',#34987);
#10395=VERTEX_POINT('',#34989);
#10396=VERTEX_POINT('',#34991);
#10397=VERTEX_POINT('',#34994);
#10398=VERTEX_POINT('',#34995);
#10399=VERTEX_POINT('',#34997);
#10400=VERTEX_POINT('',#34999);
#10401=VERTEX_POINT('',#35001);
#10402=VERTEX_POINT('',#35003);
#10403=VERTEX_POINT('',#35006);
#10404=VERTEX_POINT('',#35007);
#10405=VERTEX_POINT('',#35009);
#10406=VERTEX_POINT('',#35011);
#10407=VERTEX_POINT('',#35013);
#10408=VERTEX_POINT('',#35015);
#10409=VERTEX_POINT('',#35018);
#10410=VERTEX_POINT('',#35019);
#10411=VERTEX_POINT('',#35021);
#10412=VERTEX_POINT('',#35023);
#10413=VERTEX_POINT('',#35025);
#10414=VERTEX_POINT('',#35027);
#10415=VERTEX_POINT('',#35030);
#10416=VERTEX_POINT('',#35031);
#10417=VERTEX_POINT('',#35033);
#10418=VERTEX_POINT('',#35035);
#10419=VERTEX_POINT('',#35037);
#10420=VERTEX_POINT('',#35039);
#10421=VERTEX_POINT('',#35042);
#10422=VERTEX_POINT('',#35043);
#10423=VERTEX_POINT('',#35045);
#10424=VERTEX_POINT('',#35047);
#10425=VERTEX_POINT('',#35049);
#10426=VERTEX_POINT('',#35051);
#10427=VERTEX_POINT('',#35054);
#10428=VERTEX_POINT('',#35055);
#10429=VERTEX_POINT('',#35057);
#10430=VERTEX_POINT('',#35059);
#10431=VERTEX_POINT('',#35061);
#10432=VERTEX_POINT('',#35063);
#10433=VERTEX_POINT('',#35066);
#10434=VERTEX_POINT('',#35067);
#10435=VERTEX_POINT('',#35069);
#10436=VERTEX_POINT('',#35071);
#10437=VERTEX_POINT('',#35073);
#10438=VERTEX_POINT('',#35075);
#10439=VERTEX_POINT('',#35078);
#10440=VERTEX_POINT('',#35079);
#10441=VERTEX_POINT('',#35081);
#10442=VERTEX_POINT('',#35083);
#10443=VERTEX_POINT('',#35085);
#10444=VERTEX_POINT('',#35087);
#10445=VERTEX_POINT('',#35090);
#10446=VERTEX_POINT('',#35091);
#10447=VERTEX_POINT('',#35093);
#10448=VERTEX_POINT('',#35095);
#10449=VERTEX_POINT('',#35097);
#10450=VERTEX_POINT('',#35099);
#10451=VERTEX_POINT('',#35102);
#10452=VERTEX_POINT('',#35103);
#10453=VERTEX_POINT('',#35105);
#10454=VERTEX_POINT('',#35107);
#10455=VERTEX_POINT('',#35109);
#10456=VERTEX_POINT('',#35111);
#10457=VERTEX_POINT('',#35114);
#10458=VERTEX_POINT('',#35115);
#10459=VERTEX_POINT('',#35117);
#10460=VERTEX_POINT('',#35119);
#10461=VERTEX_POINT('',#35121);
#10462=VERTEX_POINT('',#35123);
#10463=VERTEX_POINT('',#35126);
#10464=VERTEX_POINT('',#35127);
#10465=VERTEX_POINT('',#35129);
#10466=VERTEX_POINT('',#35131);
#10467=VERTEX_POINT('',#35133);
#10468=VERTEX_POINT('',#35135);
#10469=VERTEX_POINT('',#35138);
#10470=VERTEX_POINT('',#35139);
#10471=VERTEX_POINT('',#35141);
#10472=VERTEX_POINT('',#35143);
#10473=VERTEX_POINT('',#35145);
#10474=VERTEX_POINT('',#35147);
#10475=VERTEX_POINT('',#35150);
#10476=VERTEX_POINT('',#35153);
#10477=VERTEX_POINT('',#35155);
#10478=VERTEX_POINT('',#35159);
#10479=VERTEX_POINT('',#35160);
#10480=VERTEX_POINT('',#35165);
#10481=VERTEX_POINT('',#35169);
#10482=VERTEX_POINT('',#35170);
#10483=VERTEX_POINT('',#35178);
#10484=VERTEX_POINT('',#35179);
#10485=VERTEX_POINT('',#35184);
#10486=VERTEX_POINT('',#35188);
#10487=VERTEX_POINT('',#35189);
#10488=VERTEX_POINT('',#35195);
#10489=VERTEX_POINT('',#35202);
#10490=VERTEX_POINT('',#35203);
#10491=VERTEX_POINT('',#35208);
#10492=VERTEX_POINT('',#35212);
#10493=VERTEX_POINT('',#35213);
#10494=VERTEX_POINT('',#35219);
#10495=VERTEX_POINT('',#35226);
#10496=VERTEX_POINT('',#35228);
#10497=VERTEX_POINT('',#35232);
#10498=VERTEX_POINT('',#35233);
#10499=VERTEX_POINT('',#35238);
#10500=VERTEX_POINT('',#35242);
#10501=VERTEX_POINT('',#35243);
#10502=VERTEX_POINT('',#35249);
#10503=VERTEX_POINT('',#35256);
#10504=VERTEX_POINT('',#35257);
#10505=VERTEX_POINT('',#35262);
#10506=VERTEX_POINT('',#35266);
#10507=VERTEX_POINT('',#35267);
#10508=VERTEX_POINT('',#35273);
#10509=VERTEX_POINT('',#35280);
#10510=VERTEX_POINT('',#35281);
#10511=VERTEX_POINT('',#35286);
#10512=VERTEX_POINT('',#35290);
#10513=VERTEX_POINT('',#35291);
#10514=VERTEX_POINT('',#35296);
#10515=VERTEX_POINT('',#35298);
#10516=VERTEX_POINT('',#35300);
#10517=VERTEX_POINT('',#35308);
#10518=VERTEX_POINT('',#35309);
#10519=VERTEX_POINT('',#35314);
#10520=VERTEX_POINT('',#35318);
#10521=VERTEX_POINT('',#35319);
#10522=VERTEX_POINT('',#35325);
#10523=VERTEX_POINT('',#35332);
#10524=VERTEX_POINT('',#35333);
#10525=VERTEX_POINT('',#35338);
#10526=VERTEX_POINT('',#35342);
#10527=VERTEX_POINT('',#35343);
#10528=VERTEX_POINT('',#35349);
#10529=VERTEX_POINT('',#35356);
#10530=VERTEX_POINT('',#35358);
#10531=VERTEX_POINT('',#35362);
#10532=VERTEX_POINT('',#35364);
#10533=VERTEX_POINT('',#35366);
#10534=VERTEX_POINT('',#35376);
#10535=VERTEX_POINT('',#35377);
#10536=VERTEX_POINT('',#35382);
#10537=VERTEX_POINT('',#35386);
#10538=VERTEX_POINT('',#35387);
#10539=VERTEX_POINT('',#35393);
#10540=VERTEX_POINT('',#35400);
#10541=VERTEX_POINT('',#35401);
#10542=VERTEX_POINT('',#35406);
#10543=VERTEX_POINT('',#35410);
#10544=VERTEX_POINT('',#35411);
#10545=VERTEX_POINT('',#35417);
#10546=VERTEX_POINT('',#35424);
#10547=VERTEX_POINT('',#35425);
#10548=VERTEX_POINT('',#35430);
#10549=VERTEX_POINT('',#35434);
#10550=VERTEX_POINT('',#35435);
#10551=VERTEX_POINT('',#35440);
#10552=VERTEX_POINT('',#35442);
#10553=VERTEX_POINT('',#35444);
#10554=VERTEX_POINT('',#35452);
#10555=VERTEX_POINT('',#35453);
#10556=VERTEX_POINT('',#35458);
#10557=VERTEX_POINT('',#35462);
#10558=VERTEX_POINT('',#35463);
#10559=VERTEX_POINT('',#35469);
#10560=VERTEX_POINT('',#35476);
#10561=VERTEX_POINT('',#35477);
#10562=VERTEX_POINT('',#35482);
#10563=VERTEX_POINT('',#35486);
#10564=VERTEX_POINT('',#35487);
#10565=VERTEX_POINT('',#35493);
#10566=VERTEX_POINT('',#35500);
#10567=VERTEX_POINT('',#35501);
#10568=VERTEX_POINT('',#35506);
#10569=VERTEX_POINT('',#35510);
#10570=VERTEX_POINT('',#35511);
#10571=VERTEX_POINT('',#35517);
#10572=VERTEX_POINT('',#35524);
#10573=VERTEX_POINT('',#35526);
#10574=VERTEX_POINT('',#35530);
#10575=VERTEX_POINT('',#35531);
#10576=VERTEX_POINT('',#35536);
#10577=VERTEX_POINT('',#35540);
#10578=VERTEX_POINT('',#35541);
#10579=VERTEX_POINT('',#35547);
#10580=VERTEX_POINT('',#35554);
#10581=VERTEX_POINT('',#35555);
#10582=VERTEX_POINT('',#35560);
#10583=VERTEX_POINT('',#35564);
#10584=VERTEX_POINT('',#35565);
#10585=VERTEX_POINT('',#35571);
#10586=VERTEX_POINT('',#35578);
#10587=VERTEX_POINT('',#35580);
#10588=VERTEX_POINT('',#35584);
#10589=VERTEX_POINT('',#35586);
#10590=VERTEX_POINT('',#35588);
#10591=VERTEX_POINT('',#35598);
#10592=VERTEX_POINT('',#35599);
#10593=VERTEX_POINT('',#35604);
#10594=VERTEX_POINT('',#35608);
#10595=VERTEX_POINT('',#35609);
#10596=VERTEX_POINT('',#35615);
#10597=VERTEX_POINT('',#35622);
#10598=VERTEX_POINT('',#35623);
#10599=VERTEX_POINT('',#35628);
#10600=VERTEX_POINT('',#35632);
#10601=VERTEX_POINT('',#35633);
#10602=VERTEX_POINT('',#35639);
#10603=VERTEX_POINT('',#35646);
#10604=VERTEX_POINT('',#35648);
#10605=VERTEX_POINT('',#35652);
#10606=VERTEX_POINT('',#35653);
#10607=VERTEX_POINT('',#35659);
#10608=VERTEX_POINT('',#35665);
#10609=VERTEX_POINT('',#35666);
#10610=VERTEX_POINT('',#35671);
#10611=VERTEX_POINT('',#35675);
#10612=VERTEX_POINT('',#35676);
#10613=VERTEX_POINT('',#35682);
#10614=VERTEX_POINT('',#35689);
#10615=VERTEX_POINT('',#35690);
#10616=VERTEX_POINT('',#35695);
#10617=VERTEX_POINT('',#35699);
#10618=VERTEX_POINT('',#35700);
#10619=VERTEX_POINT('',#35706);
#10620=VERTEX_POINT('',#35713);
#10621=VERTEX_POINT('',#35714);
#10622=VERTEX_POINT('',#35719);
#10623=VERTEX_POINT('',#35723);
#10624=VERTEX_POINT('',#35724);
#10625=VERTEX_POINT('',#35730);
#10626=VERTEX_POINT('',#35737);
#10627=VERTEX_POINT('',#35738);
#10628=VERTEX_POINT('',#35744);
#10629=VERTEX_POINT('',#35750);
#10630=VERTEX_POINT('',#35751);
#10631=VERTEX_POINT('',#35756);
#10632=VERTEX_POINT('',#35760);
#10633=VERTEX_POINT('',#35761);
#10634=VERTEX_POINT('',#35769);
#10635=VERTEX_POINT('',#35770);
#10636=VERTEX_POINT('',#35776);
#10637=VERTEX_POINT('',#35782);
#10638=VERTEX_POINT('',#35783);
#10639=VERTEX_POINT('',#35791);
#10640=VERTEX_POINT('',#35792);
#10641=VERTEX_POINT('',#35798);
#10642=VERTEX_POINT('',#35804);
#10643=VERTEX_POINT('',#35805);
#10644=VERTEX_POINT('',#35855);
#10645=VERTEX_POINT('',#35859);
#10646=VERTEX_POINT('',#35867);
#10647=VERTEX_POINT('',#35869);
#10648=VERTEX_POINT('',#35871);
#10649=VERTEX_POINT('',#35875);
#10650=VERTEX_POINT('',#35877);
#10651=VERTEX_POINT('',#35881);
#10652=VERTEX_POINT('',#35884);
#10653=VERTEX_POINT('',#35888);
#10654=VERTEX_POINT('',#35891);
#10655=VERTEX_POINT('',#35893);
#10656=VERTEX_POINT('',#35897);
#10657=VERTEX_POINT('',#35901);
#10658=VERTEX_POINT('',#35904);
#10659=VERTEX_POINT('',#35906);
#10660=VERTEX_POINT('',#35910);
#10661=VERTEX_POINT('',#35912);
#10662=VERTEX_POINT('',#35916);
#10663=VERTEX_POINT('',#35920);
#10664=VERTEX_POINT('',#35924);
#10665=VERTEX_POINT('',#35928);
#10666=VERTEX_POINT('',#35931);
#10667=VERTEX_POINT('',#35932);
#10668=VERTEX_POINT('',#35939);
#10669=VERTEX_POINT('',#35943);
#10670=VERTEX_POINT('',#35947);
#10671=VERTEX_POINT('',#35951);
#10672=VERTEX_POINT('',#35958);
#10673=VERTEX_POINT('',#35960);
#10674=VERTEX_POINT('',#35962);
#10675=VERTEX_POINT('',#35966);
#10676=VERTEX_POINT('',#35968);
#10677=VERTEX_POINT('',#35970);
#10678=VERTEX_POINT('',#35973);
#10679=VERTEX_POINT('',#35977);
#10680=VERTEX_POINT('',#35981);
#10681=VERTEX_POINT('',#35985);
#10682=VERTEX_POINT('',#35987);
#10683=VERTEX_POINT('',#35991);
#10684=VERTEX_POINT('',#35992);
#10685=VERTEX_POINT('',#35997);
#10686=VERTEX_POINT('',#36001);
#10687=VERTEX_POINT('',#36005);
#10688=VERTEX_POINT('',#36007);
#10689=VERTEX_POINT('',#36009);
#10690=VERTEX_POINT('',#36013);
#10691=VERTEX_POINT('',#36014);
#10692=VERTEX_POINT('',#36020);
#10693=VERTEX_POINT('',#36022);
#10694=VERTEX_POINT('',#36024);
#10695=VERTEX_POINT('',#36035);
#10696=VERTEX_POINT('',#36037);
#10697=VERTEX_POINT('',#36050);
#10698=VERTEX_POINT('',#36052);
#10699=VERTEX_POINT('',#36054);
#10700=VERTEX_POINT('',#36059);
#10701=VERTEX_POINT('',#36063);
#10702=VERTEX_POINT('',#36065);
#10703=VERTEX_POINT('',#36067);
#10704=VERTEX_POINT('',#36072);
#10705=VERTEX_POINT('',#36076);
#10706=VERTEX_POINT('',#36080);
#10707=VERTEX_POINT('',#36084);
#10708=VERTEX_POINT('',#36089);
#10709=VERTEX_POINT('',#36093);
#10710=VERTEX_POINT('',#36097);
#10711=VERTEX_POINT('',#36102);
#10712=VERTEX_POINT('',#36108);
#10713=VERTEX_POINT('',#36110);
#10714=VERTEX_POINT('',#36114);
#10715=VERTEX_POINT('',#36116);
#10716=VERTEX_POINT('',#36120);
#10717=VERTEX_POINT('',#36122);
#10718=VERTEX_POINT('',#36126);
#10719=VERTEX_POINT('',#36130);
#10720=VERTEX_POINT('',#36132);
#10721=VERTEX_POINT('',#36136);
#10722=VERTEX_POINT('',#36138);
#10723=VERTEX_POINT('',#36142);
#10724=VERTEX_POINT('',#36144);
#10725=VERTEX_POINT('',#36148);
#10726=VERTEX_POINT('',#36150);
#10727=VERTEX_POINT('',#36154);
#10728=VERTEX_POINT('',#36156);
#10729=VERTEX_POINT('',#36160);
#10730=VERTEX_POINT('',#36162);
#10731=VERTEX_POINT('',#36166);
#10732=VERTEX_POINT('',#36168);
#10733=VERTEX_POINT('',#36170);
#10734=VERTEX_POINT('',#36174);
#10735=VERTEX_POINT('',#36175);
#10736=VERTEX_POINT('',#36180);
#10737=VERTEX_POINT('',#36183);
#10738=VERTEX_POINT('',#36187);
#10739=VERTEX_POINT('',#36190);
#10740=VERTEX_POINT('',#36192);
#10741=VERTEX_POINT('',#36196);
#10742=VERTEX_POINT('',#36198);
#10743=VERTEX_POINT('',#36205);
#10744=VERTEX_POINT('',#36206);
#10745=VERTEX_POINT('',#36210);
#10746=VERTEX_POINT('',#36214);
#10747=VERTEX_POINT('',#36215);
#10748=VERTEX_POINT('',#36219);
#10749=VERTEX_POINT('',#36223);
#10750=VERTEX_POINT('',#36225);
#10751=VERTEX_POINT('',#36230);
#10752=VERTEX_POINT('',#36233);
#10753=VERTEX_POINT('',#36237);
#10754=VERTEX_POINT('',#36241);
#10755=VERTEX_POINT('',#36243);
#10756=VERTEX_POINT('',#36247);
#10757=VERTEX_POINT('',#36250);
#10758=VERTEX_POINT('',#36253);
#10759=VERTEX_POINT('',#36257);
#10760=VERTEX_POINT('',#36260);
#10761=VERTEX_POINT('',#36266);
#10762=VERTEX_POINT('',#36270);
#10763=VERTEX_POINT('',#36273);
#10764=VERTEX_POINT('',#36277);
#10765=VERTEX_POINT('',#36280);
#10766=VERTEX_POINT('',#36284);
#10767=VERTEX_POINT('',#36290);
#10768=VERTEX_POINT('',#36292);
#10769=VERTEX_POINT('',#36294);
#10770=VERTEX_POINT('',#36298);
#10771=VERTEX_POINT('',#36301);
#10772=VERTEX_POINT('',#36305);
#10773=VERTEX_POINT('',#36306);
#10774=VERTEX_POINT('',#36311);
#10775=VERTEX_POINT('',#36313);
#10776=VERTEX_POINT('',#36315);
#10777=VERTEX_POINT('',#36320);
#10778=VERTEX_POINT('',#36322);
#10779=VERTEX_POINT('',#36366);
#10780=VERTEX_POINT('',#36368);
#10781=VERTEX_POINT('',#36375);
#10782=VERTEX_POINT('',#36377);
#10783=VERTEX_POINT('',#36473);
#10784=VERTEX_POINT('',#36480);
#10785=VERTEX_POINT('',#36505);
#10786=VERTEX_POINT('',#36643);
#10787=VERTEX_POINT('',#36644);
#10788=VERTEX_POINT('',#36667);
#10789=VERTEX_POINT('',#36693);
#10790=VERTEX_POINT('',#36702);
#10791=VERTEX_POINT('',#36704);
#10792=VERTEX_POINT('',#36741);
#10793=VERTEX_POINT('',#36752);
#10794=VERTEX_POINT('',#36809);
#10795=VERTEX_POINT('',#36810);
#10796=VERTEX_POINT('',#36829);
#10797=VERTEX_POINT('',#36914);
#10798=VERTEX_POINT('',#36916);
#10799=VERTEX_POINT('',#36920);
#10800=VERTEX_POINT('',#36924);
#10801=VERTEX_POINT('',#36926);
#10802=VERTEX_POINT('',#36928);
#10803=VERTEX_POINT('',#36931);
#10804=VERTEX_POINT('',#36935);
#10805=VERTEX_POINT('',#36937);
#10806=VERTEX_POINT('',#36939);
#10807=VERTEX_POINT('',#36942);
#10808=VERTEX_POINT('',#36946);
#10809=VERTEX_POINT('',#36952);
#10810=VERTEX_POINT('',#36956);
#10811=VERTEX_POINT('',#36964);
#10812=VERTEX_POINT('',#36966);
#10813=VERTEX_POINT('',#36970);
#10814=VERTEX_POINT('',#36972);
#10815=VERTEX_POINT('',#36979);
#10816=VERTEX_POINT('',#36981);
#10817=VERTEX_POINT('',#36983);
#10818=VERTEX_POINT('',#36987);
#10819=VERTEX_POINT('',#36988);
#10820=VERTEX_POINT('',#36993);
#10821=VERTEX_POINT('',#36994);
#10822=VERTEX_POINT('',#36996);
#10823=VERTEX_POINT('',#36998);
#10824=VERTEX_POINT('',#37001);
#10825=VERTEX_POINT('',#37003);
#10826=VERTEX_POINT('',#37009);
#10827=VERTEX_POINT('',#37013);
#10828=VERTEX_POINT('',#37015);
#10829=VERTEX_POINT('',#37017);
#10830=VERTEX_POINT('',#37019);
#10831=VERTEX_POINT('',#37022);
#10832=VERTEX_POINT('',#37023);
#10833=VERTEX_POINT('',#37028);
#10834=VERTEX_POINT('',#37029);
#10835=VERTEX_POINT('',#37034);
#10836=VERTEX_POINT('',#37038);
#10837=VERTEX_POINT('',#37044);
#10838=VERTEX_POINT('',#37048);
#10839=VERTEX_POINT('',#37054);
#10840=VERTEX_POINT('',#37058);
#10841=VERTEX_POINT('',#37067);
#10842=VERTEX_POINT('',#37068);
#10843=VERTEX_POINT('',#37070);
#10844=VERTEX_POINT('',#37072);
#10845=VERTEX_POINT('',#37076);
#10846=VERTEX_POINT('',#37077);
#10847=VERTEX_POINT('',#37079);
#10848=VERTEX_POINT('',#37081);
#10849=VERTEX_POINT('',#37089);
#10850=VERTEX_POINT('',#37091);
#10851=VERTEX_POINT('',#37093);
#10852=VERTEX_POINT('',#37095);
#10853=VERTEX_POINT('',#37096);
#10854=VERTEX_POINT('',#37098);
#10855=VERTEX_POINT('',#37100);
#10856=VERTEX_POINT('',#37103);
#10857=VERTEX_POINT('',#37104);
#10858=VERTEX_POINT('',#37106);
#10859=VERTEX_POINT('',#37108);
#10860=VERTEX_POINT('',#37111);
#10861=VERTEX_POINT('',#37112);
#10862=VERTEX_POINT('',#37114);
#10863=VERTEX_POINT('',#37116);
#10864=VERTEX_POINT('',#37119);
#10865=VERTEX_POINT('',#37120);
#10866=VERTEX_POINT('',#37122);
#10867=VERTEX_POINT('',#37124);
#10868=VERTEX_POINT('',#37127);
#10869=VERTEX_POINT('',#37128);
#10870=VERTEX_POINT('',#37130);
#10871=VERTEX_POINT('',#37132);
#10872=VERTEX_POINT('',#37135);
#10873=VERTEX_POINT('',#37136);
#10874=VERTEX_POINT('',#37138);
#10875=VERTEX_POINT('',#37140);
#10876=VERTEX_POINT('',#37143);
#10877=VERTEX_POINT('',#37148);
#10878=VERTEX_POINT('',#37152);
#10879=VERTEX_POINT('',#37156);
#10880=VERTEX_POINT('',#37160);
#10881=VERTEX_POINT('',#37162);
#10882=VERTEX_POINT('',#37166);
#10883=VERTEX_POINT('',#37170);
#10884=VERTEX_POINT('',#37176);
#10885=VERTEX_POINT('',#37178);
#10886=VERTEX_POINT('',#37182);
#10887=VERTEX_POINT('',#37186);
#10888=VERTEX_POINT('',#37192);
#10889=VERTEX_POINT('',#37194);
#10890=VERTEX_POINT('',#37198);
#10891=VERTEX_POINT('',#37202);
#10892=VERTEX_POINT('',#37208);
#10893=VERTEX_POINT('',#37210);
#10894=VERTEX_POINT('',#37214);
#10895=VERTEX_POINT('',#37218);
#10896=VERTEX_POINT('',#37224);
#10897=VERTEX_POINT('',#37226);
#10898=VERTEX_POINT('',#37230);
#10899=VERTEX_POINT('',#37234);
#10900=VERTEX_POINT('',#37240);
#10901=VERTEX_POINT('',#37242);
#10902=VERTEX_POINT('',#37246);
#10903=VERTEX_POINT('',#37250);
#10904=VERTEX_POINT('',#37256);
#10905=VERTEX_POINT('',#37262);
#10906=VERTEX_POINT('',#37263);
#10907=VERTEX_POINT('',#37265);
#10908=VERTEX_POINT('',#37267);
#10909=VERTEX_POINT('',#37271);
#10910=VERTEX_POINT('',#37273);
#10911=VERTEX_POINT('',#37277);
#10912=VERTEX_POINT('',#37279);
#10913=VERTEX_POINT('',#37281);
#10914=VERTEX_POINT('',#37283);
#10915=VERTEX_POINT('',#37285);
#10916=VERTEX_POINT('',#37287);
#10917=VERTEX_POINT('',#37289);
#10918=VERTEX_POINT('',#37291);
#10919=VERTEX_POINT('',#37293);
#10920=VERTEX_POINT('',#37295);
#10921=VERTEX_POINT('',#37297);
#10922=VERTEX_POINT('',#37299);
#10923=VERTEX_POINT('',#37301);
#10924=VERTEX_POINT('',#37305);
#10925=VERTEX_POINT('',#37307);
#10926=VERTEX_POINT('',#37311);
#10927=VERTEX_POINT('',#37315);
#10928=VERTEX_POINT('',#37317);
#10929=VERTEX_POINT('',#37319);
#10930=VERTEX_POINT('',#37321);
#10931=VERTEX_POINT('',#37323);
#10932=VERTEX_POINT('',#37325);
#10933=VERTEX_POINT('',#37328);
#10934=VERTEX_POINT('',#37330);
#10935=VERTEX_POINT('',#37332);
#10936=VERTEX_POINT('',#37334);
#10937=VERTEX_POINT('',#37341);
#10938=VERTEX_POINT('',#37342);
#10939=VERTEX_POINT('',#37344);
#10940=VERTEX_POINT('',#37346);
#10941=VERTEX_POINT('',#37357);
#10942=VERTEX_POINT('',#37358);
#10943=VERTEX_POINT('',#37360);
#10944=VERTEX_POINT('',#37362);
#10945=VERTEX_POINT('',#37370);
#10946=VERTEX_POINT('',#37371);
#10947=VERTEX_POINT('',#37373);
#10948=VERTEX_POINT('',#37375);
#10949=VERTEX_POINT('',#37378);
#10950=VERTEX_POINT('',#37380);
#10951=VERTEX_POINT('',#37387);
#10952=VERTEX_POINT('',#37391);
#10953=VERTEX_POINT('',#37395);
#10954=VERTEX_POINT('',#37397);
#10955=VERTEX_POINT('',#37401);
#10956=VERTEX_POINT('',#37403);
#10957=VERTEX_POINT('',#37412);
#10958=VERTEX_POINT('',#37413);
#10959=VERTEX_POINT('',#37418);
#10960=VERTEX_POINT('',#37422);
#10961=VERTEX_POINT('',#37429);
#10962=VERTEX_POINT('',#37431);
#10963=VERTEX_POINT('',#37435);
#10964=VERTEX_POINT('',#37439);
#10965=VERTEX_POINT('',#37448);
#10966=VERTEX_POINT('',#37449);
#10967=VERTEX_POINT('',#37451);
#10968=VERTEX_POINT('',#37453);
#10969=VERTEX_POINT('',#37457);
#10970=VERTEX_POINT('',#37459);
#10971=VERTEX_POINT('',#37461);
#10972=VERTEX_POINT('',#37463);
#10973=VERTEX_POINT('',#37465);
#10974=VERTEX_POINT('',#37467);
#10975=VERTEX_POINT('',#37469);
#10976=VERTEX_POINT('',#37471);
#10977=VERTEX_POINT('',#37473);
#10978=VERTEX_POINT('',#37475);
#10979=VERTEX_POINT('',#37479);
#10980=VERTEX_POINT('',#37483);
#10981=VERTEX_POINT('',#37487);
#10982=VERTEX_POINT('',#37489);
#10983=VERTEX_POINT('',#37493);
#10984=VERTEX_POINT('',#37495);
#10985=VERTEX_POINT('',#37499);
#10986=VERTEX_POINT('',#37501);
#10987=VERTEX_POINT('',#37505);
#10988=VERTEX_POINT('',#37509);
#10989=VERTEX_POINT('',#37518);
#10990=VERTEX_POINT('',#37520);
#10991=VERTEX_POINT('',#37524);
#10992=VERTEX_POINT('',#37528);
#10993=VERTEX_POINT('',#37532);
#10994=VERTEX_POINT('',#37533);
#10995=VERTEX_POINT('',#37535);
#10996=VERTEX_POINT('',#37537);
#10997=VERTEX_POINT('',#37542);
#10998=VERTEX_POINT('',#37544);
#10999=VERTEX_POINT('',#37548);
#11000=VERTEX_POINT('',#37550);
#11001=VERTEX_POINT('',#37560);
#11002=VERTEX_POINT('',#37561);
#11003=VERTEX_POINT('',#37563);
#11004=VERTEX_POINT('',#37565);
#11005=VERTEX_POINT('',#37569);
#11006=VERTEX_POINT('',#37571);
#11007=VERTEX_POINT('',#37575);
#11008=VERTEX_POINT('',#37577);
#11009=VERTEX_POINT('',#37585);
#11010=VERTEX_POINT('',#37586);
#11011=VERTEX_POINT('',#37588);
#11012=VERTEX_POINT('',#37590);
#11013=VERTEX_POINT('',#37594);
#11014=VERTEX_POINT('',#37596);
#11015=VERTEX_POINT('',#37600);
#11016=VERTEX_POINT('',#37602);
#11017=VERTEX_POINT('',#37610);
#11018=VERTEX_POINT('',#37612);
#11019=VERTEX_POINT('',#37617);
#11020=VERTEX_POINT('',#37618);
#11021=VERTEX_POINT('',#37620);
#11022=VERTEX_POINT('',#37622);
#11023=VERTEX_POINT('',#37626);
#11024=VERTEX_POINT('',#37628);
#11025=VERTEX_POINT('',#37632);
#11026=VERTEX_POINT('',#37634);
#11027=VERTEX_POINT('',#37642);
#11028=VERTEX_POINT('',#37643);
#11029=VERTEX_POINT('',#37645);
#11030=VERTEX_POINT('',#37647);
#11031=VERTEX_POINT('',#37651);
#11032=VERTEX_POINT('',#37653);
#11033=VERTEX_POINT('',#37657);
#11034=VERTEX_POINT('',#37659);
#11035=VERTEX_POINT('',#37667);
#11036=VERTEX_POINT('',#37668);
#11037=VERTEX_POINT('',#37670);
#11038=VERTEX_POINT('',#37672);
#11039=VERTEX_POINT('',#37676);
#11040=VERTEX_POINT('',#37678);
#11041=VERTEX_POINT('',#37682);
#11042=VERTEX_POINT('',#37684);
#11043=VERTEX_POINT('',#37692);
#11044=VERTEX_POINT('',#37693);
#11045=VERTEX_POINT('',#37695);
#11046=VERTEX_POINT('',#37697);
#11047=VERTEX_POINT('',#37701);
#11048=VERTEX_POINT('',#37703);
#11049=VERTEX_POINT('',#37707);
#11050=VERTEX_POINT('',#37709);
#11051=VERTEX_POINT('',#37717);
#11052=VERTEX_POINT('',#37719);
#11053=VERTEX_POINT('',#37723);
#11054=VERTEX_POINT('',#37725);
#11055=VERTEX_POINT('',#37729);
#11056=VERTEX_POINT('',#37731);
#11057=VERTEX_POINT('',#37735);
#11058=VERTEX_POINT('',#37737);
#11059=VERTEX_POINT('',#37741);
#11060=VERTEX_POINT('',#37744);
#11061=VERTEX_POINT('',#37750);
#11062=VERTEX_POINT('',#37751);
#11063=VERTEX_POINT('',#37753);
#11064=VERTEX_POINT('',#37776);
#11065=VERTEX_POINT('',#37779);
#11066=VERTEX_POINT('',#37784);
#11067=VERTEX_POINT('',#37806);
#11068=VERTEX_POINT('',#37807);
#11069=VERTEX_POINT('',#37860);
#11070=VERTEX_POINT('',#37861);
#11071=VERTEX_POINT('',#37908);
#11072=VERTEX_POINT('',#37909);
#11073=VERTEX_POINT('',#37911);
#11074=VERTEX_POINT('',#37918);
#11075=VERTEX_POINT('',#37926);
#11076=VERTEX_POINT('',#37927);
#11077=VERTEX_POINT('',#37950);
#11078=VERTEX_POINT('',#37951);
#11079=VERTEX_POINT('',#37975);
#11080=VERTEX_POINT('',#37976);
#11081=VERTEX_POINT('',#38000);
#11082=VERTEX_POINT('',#38047);
#11083=VERTEX_POINT('',#38049);
#11084=VERTEX_POINT('',#38232);
#11085=VERTEX_POINT('',#38287);
#11086=VERTEX_POINT('',#38477);
#11087=VERTEX_POINT('',#38478);
#11088=VERTEX_POINT('',#38482);
#11089=VERTEX_POINT('',#38483);
#11090=VERTEX_POINT('',#38485);
#11091=VERTEX_POINT('',#38487);
#11092=VERTEX_POINT('',#38491);
#11093=VERTEX_POINT('',#38493);
#11094=VERTEX_POINT('',#38497);
#11095=VERTEX_POINT('',#38499);
#11096=VERTEX_POINT('',#38503);
#11097=VERTEX_POINT('',#38505);
#11098=VERTEX_POINT('',#38509);
#11099=VERTEX_POINT('',#38511);
#11100=VERTEX_POINT('',#38519);
#11101=VERTEX_POINT('',#38524);
#11102=VERTEX_POINT('',#38530);
#11103=VERTEX_POINT('',#38531);
#11104=VERTEX_POINT('',#38533);
#11105=VERTEX_POINT('',#38553);
#11106=VERTEX_POINT('',#38555);
#11107=VERTEX_POINT('',#38558);
#11108=VERTEX_POINT('',#38577);
#11109=VERTEX_POINT('',#38578);
#11110=VERTEX_POINT('',#38625);
#11111=VERTEX_POINT('',#38626);
#11112=VERTEX_POINT('',#38673);
#11113=VERTEX_POINT('',#38674);
#11114=VERTEX_POINT('',#38727);
#11115=VERTEX_POINT('',#38728);
#11116=VERTEX_POINT('',#38775);
#11117=VERTEX_POINT('',#38776);
#11118=VERTEX_POINT('',#38823);
#11119=VERTEX_POINT('',#38824);
#11120=VERTEX_POINT('',#38874);
#11121=VERTEX_POINT('',#38875);
#11122=VERTEX_POINT('',#38922);
#11123=VERTEX_POINT('',#38923);
#11124=VERTEX_POINT('',#38925);
#11125=VERTEX_POINT('',#38935);
#11126=VERTEX_POINT('',#38946);
#11127=VERTEX_POINT('',#38947);
#11128=VERTEX_POINT('',#38971);
#11129=VERTEX_POINT('',#38972);
#11130=VERTEX_POINT('',#38996);
#11131=VERTEX_POINT('',#38997);
#11132=VERTEX_POINT('',#39020);
#11133=VERTEX_POINT('',#39021);
#11134=VERTEX_POINT('',#39045);
#11135=VERTEX_POINT('',#39046);
#11136=VERTEX_POINT('',#39070);
#11137=VERTEX_POINT('',#39071);
#11138=VERTEX_POINT('',#39094);
#11139=VERTEX_POINT('',#39095);
#11140=VERTEX_POINT('',#39342);
#11141=VERTEX_POINT('',#39402);
#11142=VERTEX_POINT('',#39459);
#11143=VERTEX_POINT('',#39739);
#11144=VERTEX_POINT('',#39799);
#11145=VERTEX_POINT('',#39800);
#11146=VERTEX_POINT('',#39804);
#11147=VERTEX_POINT('',#39808);
#11148=VERTEX_POINT('',#39812);
#11149=VERTEX_POINT('',#39813);
#11150=VERTEX_POINT('',#39817);
#11151=VERTEX_POINT('',#39823);
#11152=VERTEX_POINT('',#39824);
#11153=VERTEX_POINT('',#39828);
#11154=VERTEX_POINT('',#39834);
#11155=VERTEX_POINT('',#39835);
#11156=VERTEX_POINT('',#39839);
#11157=VERTEX_POINT('',#39845);
#11158=VERTEX_POINT('',#39846);
#11159=VERTEX_POINT('',#39850);
#11160=VERTEX_POINT('',#39856);
#11161=VERTEX_POINT('',#39857);
#11162=VERTEX_POINT('',#39861);
#11163=VERTEX_POINT('',#39867);
#11164=VERTEX_POINT('',#39868);
#11165=VERTEX_POINT('',#39872);
#11166=VERTEX_POINT('',#39878);
#11167=VERTEX_POINT('',#39880);
#11168=VERTEX_POINT('',#39884);
#11169=VERTEX_POINT('',#39886);
#11170=VERTEX_POINT('',#39893);
#11171=VERTEX_POINT('',#39897);
#11172=VERTEX_POINT('',#39899);
#11173=VERTEX_POINT('',#39906);
#11174=VERTEX_POINT('',#39910);
#11175=VERTEX_POINT('',#39912);
#11176=VERTEX_POINT('',#39923);
#11177=VERTEX_POINT('',#39927);
#11178=VERTEX_POINT('',#39929);
#11179=VERTEX_POINT('',#39935);
#11180=VERTEX_POINT('',#39936);
#11181=VERTEX_POINT('',#39940);
#11182=VERTEX_POINT('',#39946);
#11183=VERTEX_POINT('',#39958);
#11184=VERTEX_POINT('',#39967);
#11185=VERTEX_POINT('',#39976);
#11186=VERTEX_POINT('',#39977);
#11187=VERTEX_POINT('',#39979);
#11188=VERTEX_POINT('',#39993);
#11189=VERTEX_POINT('',#39995);
#11190=VERTEX_POINT('',#39998);
#11191=VERTEX_POINT('',#40011);
#11192=VERTEX_POINT('',#40012);
#11193=VERTEX_POINT('',#40059);
#11194=VERTEX_POINT('',#40060);
#11195=VERTEX_POINT('',#40110);
#11196=VERTEX_POINT('',#40111);
#11197=VERTEX_POINT('',#40158);
#11198=VERTEX_POINT('',#40159);
#11199=VERTEX_POINT('',#40206);
#11200=VERTEX_POINT('',#40207);
#11201=VERTEX_POINT('',#40260);
#11202=VERTEX_POINT('',#40261);
#11203=VERTEX_POINT('',#40308);
#11204=VERTEX_POINT('',#40309);
#11205=VERTEX_POINT('',#40356);
#11206=VERTEX_POINT('',#40357);
#11207=VERTEX_POINT('',#40410);
#11208=VERTEX_POINT('',#40411);
#11209=VERTEX_POINT('',#40458);
#11210=VERTEX_POINT('',#40459);
#11211=VERTEX_POINT('',#40506);
#11212=VERTEX_POINT('',#40507);
#11213=VERTEX_POINT('',#40554);
#11214=VERTEX_POINT('',#40555);
#11215=VERTEX_POINT('',#40605);
#11216=VERTEX_POINT('',#40606);
#11217=VERTEX_POINT('',#40653);
#11218=VERTEX_POINT('',#40654);
#11219=VERTEX_POINT('',#40701);
#11220=VERTEX_POINT('',#40702);
#11221=VERTEX_POINT('',#40755);
#11222=VERTEX_POINT('',#40756);
#11223=VERTEX_POINT('',#40803);
#11224=VERTEX_POINT('',#40804);
#11225=VERTEX_POINT('',#40851);
#11226=VERTEX_POINT('',#40852);
#11227=VERTEX_POINT('',#40905);
#11228=VERTEX_POINT('',#40906);
#11229=VERTEX_POINT('',#40953);
#11230=VERTEX_POINT('',#40954);
#11231=VERTEX_POINT('',#41001);
#11232=VERTEX_POINT('',#41002);
#11233=VERTEX_POINT('',#41049);
#11234=VERTEX_POINT('',#41050);
#11235=VERTEX_POINT('',#41100);
#11236=VERTEX_POINT('',#41101);
#11237=VERTEX_POINT('',#41148);
#11238=VERTEX_POINT('',#41149);
#11239=VERTEX_POINT('',#41196);
#11240=VERTEX_POINT('',#41197);
#11241=VERTEX_POINT('',#41250);
#11242=VERTEX_POINT('',#41251);
#11243=VERTEX_POINT('',#41298);
#11244=VERTEX_POINT('',#41299);
#11245=VERTEX_POINT('',#41346);
#11246=VERTEX_POINT('',#41347);
#11247=VERTEX_POINT('',#41349);
#11248=VERTEX_POINT('',#41357);
#11249=VERTEX_POINT('',#41365);
#11250=VERTEX_POINT('',#41366);
#11251=VERTEX_POINT('',#41390);
#11252=VERTEX_POINT('',#41391);
#11253=VERTEX_POINT('',#41414);
#11254=VERTEX_POINT('',#41415);
#11255=VERTEX_POINT('',#41439);
#11256=VERTEX_POINT('',#41440);
#11257=VERTEX_POINT('',#41464);
#11258=VERTEX_POINT('',#41465);
#11259=VERTEX_POINT('',#41488);
#11260=VERTEX_POINT('',#41489);
#11261=VERTEX_POINT('',#41513);
#11262=VERTEX_POINT('',#41514);
#11263=VERTEX_POINT('',#41537);
#11264=VERTEX_POINT('',#41538);
#11265=VERTEX_POINT('',#41562);
#11266=VERTEX_POINT('',#41563);
#11267=VERTEX_POINT('',#41586);
#11268=VERTEX_POINT('',#41587);
#11269=VERTEX_POINT('',#41611);
#11270=VERTEX_POINT('',#41612);
#11271=VERTEX_POINT('',#41636);
#11272=VERTEX_POINT('',#41637);
#11273=VERTEX_POINT('',#41660);
#11274=VERTEX_POINT('',#41661);
#11275=VERTEX_POINT('',#41685);
#11276=VERTEX_POINT('',#41686);
#11277=VERTEX_POINT('',#41710);
#11278=VERTEX_POINT('',#41711);
#11279=VERTEX_POINT('',#41734);
#11280=VERTEX_POINT('',#41735);
#11281=VERTEX_POINT('',#41759);
#11282=VERTEX_POINT('',#41760);
#11283=VERTEX_POINT('',#41784);
#11284=VERTEX_POINT('',#41785);
#11285=VERTEX_POINT('',#41808);
#11286=VERTEX_POINT('',#41809);
#11287=VERTEX_POINT('',#41832);
#11288=VERTEX_POINT('',#41833);
#11289=VERTEX_POINT('',#41857);
#11290=VERTEX_POINT('',#41858);
#11291=VERTEX_POINT('',#41882);
#11292=VERTEX_POINT('',#41883);
#11293=VERTEX_POINT('',#41906);
#11294=VERTEX_POINT('',#41907);
#11295=VERTEX_POINT('',#41931);
#11296=VERTEX_POINT('',#41932);
#11297=VERTEX_POINT('',#41956);
#11298=VERTEX_POINT('',#41957);
#11299=VERTEX_POINT('',#41980);
#11300=VERTEX_POINT('',#41981);
#11301=VERTEX_POINT('',#42005);
#11302=VERTEX_POINT('',#42006);
#11303=VERTEX_POINT('',#42030);
#11304=VERTEX_POINT('',#42031);
#11305=VERTEX_POINT('',#42033);
#11306=VERTEX_POINT('',#42055);
#11307=VERTEX_POINT('',#42102);
#11308=VERTEX_POINT('',#42104);
#11309=VERTEX_POINT('',#42913);
#11310=VERTEX_POINT('',#43772);
#11311=VERTEX_POINT('',#43773);
#11312=VERTEX_POINT('',#43775);
#11313=VERTEX_POINT('',#43779);
#11314=VERTEX_POINT('',#43781);
#11315=VERTEX_POINT('',#43787);
#11316=VERTEX_POINT('',#43793);
#11317=VERTEX_POINT('',#43794);
#11318=VERTEX_POINT('',#43796);
#11319=VERTEX_POINT('',#43800);
#11320=VERTEX_POINT('',#43802);
#11321=VERTEX_POINT('',#43808);
#11322=VERTEX_POINT('',#43814);
#11323=VERTEX_POINT('',#43815);
#11324=VERTEX_POINT('',#43817);
#11325=VERTEX_POINT('',#43821);
#11326=VERTEX_POINT('',#43823);
#11327=VERTEX_POINT('',#43829);
#11328=VERTEX_POINT('',#43835);
#11329=VERTEX_POINT('',#43836);
#11330=VERTEX_POINT('',#43838);
#11331=VERTEX_POINT('',#43842);
#11332=VERTEX_POINT('',#43844);
#11333=VERTEX_POINT('',#43850);
#11334=VERTEX_POINT('',#43856);
#11335=VERTEX_POINT('',#43857);
#11336=VERTEX_POINT('',#43859);
#11337=VERTEX_POINT('',#43863);
#11338=VERTEX_POINT('',#43865);
#11339=VERTEX_POINT('',#43871);
#11340=VERTEX_POINT('',#43877);
#11341=VERTEX_POINT('',#43878);
#11342=VERTEX_POINT('',#43880);
#11343=VERTEX_POINT('',#43884);
#11344=VERTEX_POINT('',#43886);
#11345=VERTEX_POINT('',#43892);
#11346=VERTEX_POINT('',#43898);
#11347=VERTEX_POINT('',#43899);
#11348=VERTEX_POINT('',#43901);
#11349=VERTEX_POINT('',#43905);
#11350=VERTEX_POINT('',#43907);
#11351=VERTEX_POINT('',#43913);
#11352=VERTEX_POINT('',#43919);
#11353=VERTEX_POINT('',#43920);
#11354=VERTEX_POINT('',#43922);
#11355=VERTEX_POINT('',#43926);
#11356=VERTEX_POINT('',#43928);
#11357=VERTEX_POINT('',#43934);
#11358=VERTEX_POINT('',#43940);
#11359=VERTEX_POINT('',#43941);
#11360=VERTEX_POINT('',#43943);
#11361=VERTEX_POINT('',#43947);
#11362=VERTEX_POINT('',#43949);
#11363=VERTEX_POINT('',#43955);
#11364=VERTEX_POINT('',#43961);
#11365=VERTEX_POINT('',#43962);
#11366=VERTEX_POINT('',#43964);
#11367=VERTEX_POINT('',#43968);
#11368=VERTEX_POINT('',#43970);
#11369=VERTEX_POINT('',#43976);
#11370=VERTEX_POINT('',#43982);
#11371=VERTEX_POINT('',#43983);
#11372=VERTEX_POINT('',#43985);
#11373=VERTEX_POINT('',#43989);
#11374=VERTEX_POINT('',#43991);
#11375=VERTEX_POINT('',#43997);
#11376=VERTEX_POINT('',#44003);
#11377=VERTEX_POINT('',#44004);
#11378=VERTEX_POINT('',#44006);
#11379=VERTEX_POINT('',#44010);
#11380=VERTEX_POINT('',#44012);
#11381=VERTEX_POINT('',#44018);
#11382=VERTEX_POINT('',#44024);
#11383=VERTEX_POINT('',#44025);
#11384=VERTEX_POINT('',#44027);
#11385=VERTEX_POINT('',#44031);
#11386=VERTEX_POINT('',#44033);
#11387=VERTEX_POINT('',#44039);
#11388=VERTEX_POINT('',#44045);
#11389=VERTEX_POINT('',#44046);
#11390=VERTEX_POINT('',#44048);
#11391=VERTEX_POINT('',#44052);
#11392=VERTEX_POINT('',#44054);
#11393=VERTEX_POINT('',#44060);
#11394=VERTEX_POINT('',#44066);
#11395=VERTEX_POINT('',#44067);
#11396=VERTEX_POINT('',#44069);
#11397=VERTEX_POINT('',#44073);
#11398=VERTEX_POINT('',#44075);
#11399=VERTEX_POINT('',#44081);
#11400=VERTEX_POINT('',#44087);
#11401=VERTEX_POINT('',#44088);
#11402=VERTEX_POINT('',#44090);
#11403=VERTEX_POINT('',#44094);
#11404=VERTEX_POINT('',#44096);
#11405=VERTEX_POINT('',#44102);
#11406=VERTEX_POINT('',#44108);
#11407=VERTEX_POINT('',#44109);
#11408=VERTEX_POINT('',#44111);
#11409=VERTEX_POINT('',#44115);
#11410=VERTEX_POINT('',#44117);
#11411=VERTEX_POINT('',#44123);
#11412=VERTEX_POINT('',#44129);
#11413=VERTEX_POINT('',#44130);
#11414=VERTEX_POINT('',#44132);
#11415=VERTEX_POINT('',#44134);
#11416=VERTEX_POINT('',#44138);
#11417=VERTEX_POINT('',#44140);
#11418=VERTEX_POINT('',#44146);
#11419=VERTEX_POINT('',#44152);
#11420=VERTEX_POINT('',#44153);
#11421=VERTEX_POINT('',#44155);
#11422=VERTEX_POINT('',#44159);
#11423=VERTEX_POINT('',#44161);
#11424=VERTEX_POINT('',#44167);
#11425=VERTEX_POINT('',#44173);
#11426=VERTEX_POINT('',#44174);
#11427=VERTEX_POINT('',#44176);
#11428=VERTEX_POINT('',#44180);
#11429=VERTEX_POINT('',#44182);
#11430=VERTEX_POINT('',#44188);
#11431=VERTEX_POINT('',#44194);
#11432=VERTEX_POINT('',#44195);
#11433=VERTEX_POINT('',#44197);
#11434=VERTEX_POINT('',#44201);
#11435=VERTEX_POINT('',#44203);
#11436=VERTEX_POINT('',#44209);
#11437=VERTEX_POINT('',#44215);
#11438=VERTEX_POINT('',#44216);
#11439=VERTEX_POINT('',#44218);
#11440=VERTEX_POINT('',#44222);
#11441=VERTEX_POINT('',#44224);
#11442=VERTEX_POINT('',#44230);
#11443=VERTEX_POINT('',#44236);
#11444=VERTEX_POINT('',#44237);
#11445=VERTEX_POINT('',#44239);
#11446=VERTEX_POINT('',#44243);
#11447=VERTEX_POINT('',#44245);
#11448=VERTEX_POINT('',#44251);
#11449=VERTEX_POINT('',#44257);
#11450=VERTEX_POINT('',#44258);
#11451=VERTEX_POINT('',#44260);
#11452=VERTEX_POINT('',#44264);
#11453=VERTEX_POINT('',#44266);
#11454=VERTEX_POINT('',#44272);
#11455=VERTEX_POINT('',#44278);
#11456=VERTEX_POINT('',#44279);
#11457=VERTEX_POINT('',#44281);
#11458=VERTEX_POINT('',#44285);
#11459=VERTEX_POINT('',#44287);
#11460=VERTEX_POINT('',#44293);
#11461=VERTEX_POINT('',#44299);
#11462=VERTEX_POINT('',#44300);
#11463=VERTEX_POINT('',#44302);
#11464=VERTEX_POINT('',#44306);
#11465=VERTEX_POINT('',#44308);
#11466=VERTEX_POINT('',#44314);
#11467=VERTEX_POINT('',#44320);
#11468=VERTEX_POINT('',#44321);
#11469=VERTEX_POINT('',#44323);
#11470=VERTEX_POINT('',#44327);
#11471=VERTEX_POINT('',#44329);
#11472=VERTEX_POINT('',#44335);
#11473=VERTEX_POINT('',#44341);
#11474=VERTEX_POINT('',#44342);
#11475=VERTEX_POINT('',#44344);
#11476=VERTEX_POINT('',#44348);
#11477=VERTEX_POINT('',#44350);
#11478=VERTEX_POINT('',#44356);
#11479=VERTEX_POINT('',#44362);
#11480=VERTEX_POINT('',#44363);
#11481=VERTEX_POINT('',#44365);
#11482=VERTEX_POINT('',#44369);
#11483=VERTEX_POINT('',#44371);
#11484=VERTEX_POINT('',#44377);
#11485=VERTEX_POINT('',#44383);
#11486=VERTEX_POINT('',#44384);
#11487=VERTEX_POINT('',#44386);
#11488=VERTEX_POINT('',#44390);
#11489=VERTEX_POINT('',#44392);
#11490=VERTEX_POINT('',#44398);
#11491=VERTEX_POINT('',#44404);
#11492=VERTEX_POINT('',#44405);
#11493=VERTEX_POINT('',#44407);
#11494=VERTEX_POINT('',#44411);
#11495=VERTEX_POINT('',#44413);
#11496=VERTEX_POINT('',#44419);
#11497=VERTEX_POINT('',#44425);
#11498=VERTEX_POINT('',#44426);
#11499=VERTEX_POINT('',#44428);
#11500=VERTEX_POINT('',#44432);
#11501=VERTEX_POINT('',#44434);
#11502=VERTEX_POINT('',#44440);
#11503=VERTEX_POINT('',#44446);
#11504=VERTEX_POINT('',#44447);
#11505=VERTEX_POINT('',#44449);
#11506=VERTEX_POINT('',#44453);
#11507=VERTEX_POINT('',#44455);
#11508=VERTEX_POINT('',#44461);
#11509=VERTEX_POINT('',#44467);
#11510=VERTEX_POINT('',#44468);
#11511=VERTEX_POINT('',#44470);
#11512=VERTEX_POINT('',#44474);
#11513=VERTEX_POINT('',#44476);
#11514=VERTEX_POINT('',#44482);
#11515=VERTEX_POINT('',#44488);
#11516=VERTEX_POINT('',#44489);
#11517=VERTEX_POINT('',#44491);
#11518=VERTEX_POINT('',#44495);
#11519=VERTEX_POINT('',#44497);
#11520=VERTEX_POINT('',#44503);
#11521=VERTEX_POINT('',#44526);
#11522=VERTEX_POINT('',#44546);
#11523=VERTEX_POINT('',#44548);
#11524=VERTEX_POINT('',#44550);
#11525=VERTEX_POINT('',#44552);
#11526=VERTEX_POINT('',#44556);
#11527=VERTEX_POINT('',#44558);
#11528=VERTEX_POINT('',#44570);
#11529=VERTEX_POINT('',#44574);
#11530=VERTEX_POINT('',#44575);
#11531=VERTEX_POINT('',#44579);
#11532=VERTEX_POINT('',#44580);
#11533=VERTEX_POINT('',#44582);
#11534=VERTEX_POINT('',#44584);
#11535=VERTEX_POINT('',#44588);
#11536=VERTEX_POINT('',#44590);
#11537=VERTEX_POINT('',#44594);
#11538=VERTEX_POINT('',#44596);
#11539=VERTEX_POINT('',#44600);
#11540=VERTEX_POINT('',#44602);
#11541=VERTEX_POINT('',#44606);
#11542=VERTEX_POINT('',#44608);
#11543=VERTEX_POINT('',#44616);
#11544=VERTEX_POINT('',#44623);
#11545=VERTEX_POINT('',#44630);
#11546=VERTEX_POINT('',#44631);
#11547=VERTEX_POINT('',#44633);
#11548=VERTEX_POINT('',#44647);
#11549=VERTEX_POINT('',#44649);
#11550=VERTEX_POINT('',#44652);
#11551=VERTEX_POINT('',#44665);
#11552=VERTEX_POINT('',#44666);
#11553=VERTEX_POINT('',#44719);
#11554=VERTEX_POINT('',#44720);
#11555=VERTEX_POINT('',#44767);
#11556=VERTEX_POINT('',#44768);
#11557=VERTEX_POINT('',#44815);
#11558=VERTEX_POINT('',#44816);
#11559=VERTEX_POINT('',#44863);
#11560=VERTEX_POINT('',#44864);
#11561=VERTEX_POINT('',#44917);
#11562=VERTEX_POINT('',#44918);
#11563=VERTEX_POINT('',#44965);
#11564=VERTEX_POINT('',#44966);
#11565=VERTEX_POINT('',#45013);
#11566=VERTEX_POINT('',#45014);
#11567=VERTEX_POINT('',#45067);
#11568=VERTEX_POINT('',#45068);
#11569=VERTEX_POINT('',#45115);
#11570=VERTEX_POINT('',#45116);
#11571=VERTEX_POINT('',#45163);
#11572=VERTEX_POINT('',#45164);
#11573=VERTEX_POINT('',#45217);
#11574=VERTEX_POINT('',#45218);
#11575=VERTEX_POINT('',#45265);
#11576=VERTEX_POINT('',#45266);
#11577=VERTEX_POINT('',#45313);
#11578=VERTEX_POINT('',#45314);
#11579=VERTEX_POINT('',#45367);
#11580=VERTEX_POINT('',#45368);
#11581=VERTEX_POINT('',#45415);
#11582=VERTEX_POINT('',#45416);
#11583=VERTEX_POINT('',#45463);
#11584=VERTEX_POINT('',#45464);
#11585=VERTEX_POINT('',#45517);
#11586=VERTEX_POINT('',#45518);
#11587=VERTEX_POINT('',#45565);
#11588=VERTEX_POINT('',#45566);
#11589=VERTEX_POINT('',#45613);
#11590=VERTEX_POINT('',#45614);
#11591=VERTEX_POINT('',#45667);
#11592=VERTEX_POINT('',#45668);
#11593=VERTEX_POINT('',#45715);
#11594=VERTEX_POINT('',#45716);
#11595=VERTEX_POINT('',#45763);
#11596=VERTEX_POINT('',#45764);
#11597=VERTEX_POINT('',#45766);
#11598=VERTEX_POINT('',#45774);
#11599=VERTEX_POINT('',#45782);
#11600=VERTEX_POINT('',#45783);
#11601=VERTEX_POINT('',#45807);
#11602=VERTEX_POINT('',#45808);
#11603=VERTEX_POINT('',#45831);
#11604=VERTEX_POINT('',#45832);
#11605=VERTEX_POINT('',#45856);
#11606=VERTEX_POINT('',#45857);
#11607=VERTEX_POINT('',#45881);
#11608=VERTEX_POINT('',#45882);
#11609=VERTEX_POINT('',#45905);
#11610=VERTEX_POINT('',#45906);
#11611=VERTEX_POINT('',#45930);
#11612=VERTEX_POINT('',#45931);
#11613=VERTEX_POINT('',#45955);
#11614=VERTEX_POINT('',#45956);
#11615=VERTEX_POINT('',#45979);
#11616=VERTEX_POINT('',#45980);
#11617=VERTEX_POINT('',#46004);
#11618=VERTEX_POINT('',#46005);
#11619=VERTEX_POINT('',#46029);
#11620=VERTEX_POINT('',#46030);
#11621=VERTEX_POINT('',#46053);
#11622=VERTEX_POINT('',#46054);
#11623=VERTEX_POINT('',#46078);
#11624=VERTEX_POINT('',#46079);
#11625=VERTEX_POINT('',#46103);
#11626=VERTEX_POINT('',#46104);
#11627=VERTEX_POINT('',#46127);
#11628=VERTEX_POINT('',#46128);
#11629=VERTEX_POINT('',#46152);
#11630=VERTEX_POINT('',#46153);
#11631=VERTEX_POINT('',#46177);
#11632=VERTEX_POINT('',#46178);
#11633=VERTEX_POINT('',#46201);
#11634=VERTEX_POINT('',#46202);
#11635=VERTEX_POINT('',#46226);
#11636=VERTEX_POINT('',#46227);
#11637=VERTEX_POINT('',#46251);
#11638=VERTEX_POINT('',#46252);
#11639=VERTEX_POINT('',#46275);
#11640=VERTEX_POINT('',#46276);
#11641=VERTEX_POINT('',#46299);
#11642=VERTEX_POINT('',#46300);
#11643=VERTEX_POINT('',#46324);
#11644=VERTEX_POINT('',#46325);
#11645=VERTEX_POINT('',#46327);
#11646=VERTEX_POINT('',#46350);
#11647=VERTEX_POINT('',#46397);
#11648=VERTEX_POINT('',#46399);
#11649=VERTEX_POINT('',#47081);
#11650=VERTEX_POINT('',#47813);
#11651=VERTEX_POINT('',#47814);
#11652=VERTEX_POINT('',#47816);
#11653=VERTEX_POINT('',#47820);
#11654=VERTEX_POINT('',#47822);
#11655=VERTEX_POINT('',#47828);
#11656=VERTEX_POINT('',#47834);
#11657=VERTEX_POINT('',#47835);
#11658=VERTEX_POINT('',#47837);
#11659=VERTEX_POINT('',#47841);
#11660=VERTEX_POINT('',#47843);
#11661=VERTEX_POINT('',#47849);
#11662=VERTEX_POINT('',#47855);
#11663=VERTEX_POINT('',#47856);
#11664=VERTEX_POINT('',#47858);
#11665=VERTEX_POINT('',#47862);
#11666=VERTEX_POINT('',#47864);
#11667=VERTEX_POINT('',#47870);
#11668=VERTEX_POINT('',#47876);
#11669=VERTEX_POINT('',#47877);
#11670=VERTEX_POINT('',#47879);
#11671=VERTEX_POINT('',#47883);
#11672=VERTEX_POINT('',#47885);
#11673=VERTEX_POINT('',#47891);
#11674=VERTEX_POINT('',#47897);
#11675=VERTEX_POINT('',#47898);
#11676=VERTEX_POINT('',#47900);
#11677=VERTEX_POINT('',#47904);
#11678=VERTEX_POINT('',#47906);
#11679=VERTEX_POINT('',#47912);
#11680=VERTEX_POINT('',#47918);
#11681=VERTEX_POINT('',#47919);
#11682=VERTEX_POINT('',#47921);
#11683=VERTEX_POINT('',#47925);
#11684=VERTEX_POINT('',#47927);
#11685=VERTEX_POINT('',#47933);
#11686=VERTEX_POINT('',#47939);
#11687=VERTEX_POINT('',#47940);
#11688=VERTEX_POINT('',#47942);
#11689=VERTEX_POINT('',#47946);
#11690=VERTEX_POINT('',#47948);
#11691=VERTEX_POINT('',#47954);
#11692=VERTEX_POINT('',#47960);
#11693=VERTEX_POINT('',#47961);
#11694=VERTEX_POINT('',#47963);
#11695=VERTEX_POINT('',#47967);
#11696=VERTEX_POINT('',#47969);
#11697=VERTEX_POINT('',#47975);
#11698=VERTEX_POINT('',#47981);
#11699=VERTEX_POINT('',#47982);
#11700=VERTEX_POINT('',#47984);
#11701=VERTEX_POINT('',#47988);
#11702=VERTEX_POINT('',#47990);
#11703=VERTEX_POINT('',#47996);
#11704=VERTEX_POINT('',#48002);
#11705=VERTEX_POINT('',#48003);
#11706=VERTEX_POINT('',#48005);
#11707=VERTEX_POINT('',#48009);
#11708=VERTEX_POINT('',#48011);
#11709=VERTEX_POINT('',#48017);
#11710=VERTEX_POINT('',#48023);
#11711=VERTEX_POINT('',#48024);
#11712=VERTEX_POINT('',#48026);
#11713=VERTEX_POINT('',#48030);
#11714=VERTEX_POINT('',#48032);
#11715=VERTEX_POINT('',#48038);
#11716=VERTEX_POINT('',#48044);
#11717=VERTEX_POINT('',#48045);
#11718=VERTEX_POINT('',#48047);
#11719=VERTEX_POINT('',#48051);
#11720=VERTEX_POINT('',#48053);
#11721=VERTEX_POINT('',#48059);
#11722=VERTEX_POINT('',#48065);
#11723=VERTEX_POINT('',#48066);
#11724=VERTEX_POINT('',#48068);
#11725=VERTEX_POINT('',#48072);
#11726=VERTEX_POINT('',#48074);
#11727=VERTEX_POINT('',#48080);
#11728=VERTEX_POINT('',#48086);
#11729=VERTEX_POINT('',#48087);
#11730=VERTEX_POINT('',#48089);
#11731=VERTEX_POINT('',#48093);
#11732=VERTEX_POINT('',#48095);
#11733=VERTEX_POINT('',#48101);
#11734=VERTEX_POINT('',#48107);
#11735=VERTEX_POINT('',#48108);
#11736=VERTEX_POINT('',#48110);
#11737=VERTEX_POINT('',#48114);
#11738=VERTEX_POINT('',#48116);
#11739=VERTEX_POINT('',#48122);
#11740=VERTEX_POINT('',#48128);
#11741=VERTEX_POINT('',#48129);
#11742=VERTEX_POINT('',#48131);
#11743=VERTEX_POINT('',#48135);
#11744=VERTEX_POINT('',#48137);
#11745=VERTEX_POINT('',#48143);
#11746=VERTEX_POINT('',#48149);
#11747=VERTEX_POINT('',#48150);
#11748=VERTEX_POINT('',#48152);
#11749=VERTEX_POINT('',#48156);
#11750=VERTEX_POINT('',#48158);
#11751=VERTEX_POINT('',#48164);
#11752=VERTEX_POINT('',#48170);
#11753=VERTEX_POINT('',#48171);
#11754=VERTEX_POINT('',#48173);
#11755=VERTEX_POINT('',#48175);
#11756=VERTEX_POINT('',#48179);
#11757=VERTEX_POINT('',#48181);
#11758=VERTEX_POINT('',#48187);
#11759=VERTEX_POINT('',#48193);
#11760=VERTEX_POINT('',#48194);
#11761=VERTEX_POINT('',#48196);
#11762=VERTEX_POINT('',#48200);
#11763=VERTEX_POINT('',#48202);
#11764=VERTEX_POINT('',#48208);
#11765=VERTEX_POINT('',#48214);
#11766=VERTEX_POINT('',#48215);
#11767=VERTEX_POINT('',#48217);
#11768=VERTEX_POINT('',#48221);
#11769=VERTEX_POINT('',#48223);
#11770=VERTEX_POINT('',#48229);
#11771=VERTEX_POINT('',#48235);
#11772=VERTEX_POINT('',#48236);
#11773=VERTEX_POINT('',#48238);
#11774=VERTEX_POINT('',#48242);
#11775=VERTEX_POINT('',#48244);
#11776=VERTEX_POINT('',#48250);
#11777=VERTEX_POINT('',#48256);
#11778=VERTEX_POINT('',#48257);
#11779=VERTEX_POINT('',#48259);
#11780=VERTEX_POINT('',#48263);
#11781=VERTEX_POINT('',#48265);
#11782=VERTEX_POINT('',#48271);
#11783=VERTEX_POINT('',#48277);
#11784=VERTEX_POINT('',#48278);
#11785=VERTEX_POINT('',#48280);
#11786=VERTEX_POINT('',#48284);
#11787=VERTEX_POINT('',#48286);
#11788=VERTEX_POINT('',#48292);
#11789=VERTEX_POINT('',#48298);
#11790=VERTEX_POINT('',#48299);
#11791=VERTEX_POINT('',#48301);
#11792=VERTEX_POINT('',#48305);
#11793=VERTEX_POINT('',#48307);
#11794=VERTEX_POINT('',#48313);
#11795=VERTEX_POINT('',#48319);
#11796=VERTEX_POINT('',#48320);
#11797=VERTEX_POINT('',#48322);
#11798=VERTEX_POINT('',#48326);
#11799=VERTEX_POINT('',#48328);
#11800=VERTEX_POINT('',#48334);
#11801=VERTEX_POINT('',#48340);
#11802=VERTEX_POINT('',#48341);
#11803=VERTEX_POINT('',#48343);
#11804=VERTEX_POINT('',#48347);
#11805=VERTEX_POINT('',#48349);
#11806=VERTEX_POINT('',#48355);
#11807=VERTEX_POINT('',#48361);
#11808=VERTEX_POINT('',#48362);
#11809=VERTEX_POINT('',#48364);
#11810=VERTEX_POINT('',#48368);
#11811=VERTEX_POINT('',#48370);
#11812=VERTEX_POINT('',#48376);
#11813=VERTEX_POINT('',#48382);
#11814=VERTEX_POINT('',#48383);
#11815=VERTEX_POINT('',#48385);
#11816=VERTEX_POINT('',#48389);
#11817=VERTEX_POINT('',#48391);
#11818=VERTEX_POINT('',#48397);
#11819=VERTEX_POINT('',#48403);
#11820=VERTEX_POINT('',#48404);
#11821=VERTEX_POINT('',#48406);
#11822=VERTEX_POINT('',#48410);
#11823=VERTEX_POINT('',#48412);
#11824=VERTEX_POINT('',#48418);
#11825=VERTEX_POINT('',#48424);
#11826=VERTEX_POINT('',#48425);
#11827=VERTEX_POINT('',#48427);
#11828=VERTEX_POINT('',#48431);
#11829=VERTEX_POINT('',#48433);
#11830=VERTEX_POINT('',#48439);
#11831=VERTEX_POINT('',#48445);
#11832=VERTEX_POINT('',#48446);
#11833=VERTEX_POINT('',#48448);
#11834=VERTEX_POINT('',#48452);
#11835=VERTEX_POINT('',#48454);
#11836=VERTEX_POINT('',#48460);
#11837=VERTEX_POINT('',#48466);
#11838=VERTEX_POINT('',#48467);
#11839=VERTEX_POINT('',#48469);
#11840=VERTEX_POINT('',#48473);
#11841=VERTEX_POINT('',#48475);
#11842=VERTEX_POINT('',#48481);
#11843=VERTEX_POINT('',#48487);
#11844=VERTEX_POINT('',#48488);
#11845=VERTEX_POINT('',#48490);
#11846=VERTEX_POINT('',#48494);
#11847=VERTEX_POINT('',#48496);
#11848=VERTEX_POINT('',#48502);
#11849=VERTEX_POINT('',#48508);
#11850=VERTEX_POINT('',#48509);
#11851=VERTEX_POINT('',#48511);
#11852=VERTEX_POINT('',#48515);
#11853=VERTEX_POINT('',#48517);
#11854=VERTEX_POINT('',#48523);
#11855=VERTEX_POINT('',#48529);
#11856=VERTEX_POINT('',#48530);
#11857=VERTEX_POINT('',#48532);
#11858=VERTEX_POINT('',#48536);
#11859=VERTEX_POINT('',#48538);
#11860=VERTEX_POINT('',#48544);
#11861=VERTEX_POINT('',#48567);
#11862=VERTEX_POINT('',#48587);
#11863=VERTEX_POINT('',#48589);
#11864=VERTEX_POINT('',#48591);
#11865=VERTEX_POINT('',#48593);
#11866=VERTEX_POINT('',#48597);
#11867=VERTEX_POINT('',#48599);
#11868=VERTEX_POINT('',#48611);
#11869=VERTEX_POINT('',#48615);
#11870=VERTEX_POINT('',#48616);
#11871=VERTEX_POINT('',#48620);
#11872=VERTEX_POINT('',#48621);
#11873=VERTEX_POINT('',#48623);
#11874=VERTEX_POINT('',#48625);
#11875=VERTEX_POINT('',#48629);
#11876=VERTEX_POINT('',#48631);
#11877=VERTEX_POINT('',#48635);
#11878=VERTEX_POINT('',#48637);
#11879=VERTEX_POINT('',#48641);
#11880=VERTEX_POINT('',#48643);
#11881=VERTEX_POINT('',#48647);
#11882=VERTEX_POINT('',#48649);
#11883=VERTEX_POINT('',#48657);
#11884=VERTEX_POINT('',#48664);
#11885=VERTEX_POINT('',#48671);
#11886=VERTEX_POINT('',#48672);
#11887=VERTEX_POINT('',#48674);
#11888=VERTEX_POINT('',#48691);
#11889=VERTEX_POINT('',#48693);
#11890=VERTEX_POINT('',#48696);
#11891=VERTEX_POINT('',#48712);
#11892=VERTEX_POINT('',#48713);
#11893=VERTEX_POINT('',#48760);
#11894=VERTEX_POINT('',#48761);
#11895=VERTEX_POINT('',#48808);
#11896=VERTEX_POINT('',#48809);
#11897=VERTEX_POINT('',#48862);
#11898=VERTEX_POINT('',#48863);
#11899=VERTEX_POINT('',#48910);
#11900=VERTEX_POINT('',#48911);
#11901=VERTEX_POINT('',#48964);
#11902=VERTEX_POINT('',#48965);
#11903=VERTEX_POINT('',#49012);
#11904=VERTEX_POINT('',#49013);
#11905=VERTEX_POINT('',#49060);
#11906=VERTEX_POINT('',#49061);
#11907=VERTEX_POINT('',#49114);
#11908=VERTEX_POINT('',#49115);
#11909=VERTEX_POINT('',#49162);
#11910=VERTEX_POINT('',#49163);
#11911=VERTEX_POINT('',#49210);
#11912=VERTEX_POINT('',#49211);
#11913=VERTEX_POINT('',#49264);
#11914=VERTEX_POINT('',#49265);
#11915=VERTEX_POINT('',#49267);
#11916=VERTEX_POINT('',#49277);
#11917=VERTEX_POINT('',#49287);
#11918=VERTEX_POINT('',#49288);
#11919=VERTEX_POINT('',#49312);
#11920=VERTEX_POINT('',#49313);
#11921=VERTEX_POINT('',#49336);
#11922=VERTEX_POINT('',#49337);
#11923=VERTEX_POINT('',#49361);
#11924=VERTEX_POINT('',#49362);
#11925=VERTEX_POINT('',#49386);
#11926=VERTEX_POINT('',#49387);
#11927=VERTEX_POINT('',#49410);
#11928=VERTEX_POINT('',#49411);
#11929=VERTEX_POINT('',#49435);
#11930=VERTEX_POINT('',#49436);
#11931=VERTEX_POINT('',#49460);
#11932=VERTEX_POINT('',#49461);
#11933=VERTEX_POINT('',#49485);
#11934=VERTEX_POINT('',#49486);
#11935=VERTEX_POINT('',#49510);
#11936=VERTEX_POINT('',#49511);
#11937=VERTEX_POINT('',#49534);
#11938=VERTEX_POINT('',#49535);
#11939=VERTEX_POINT('',#49537);
#11940=VERTEX_POINT('',#49560);
#11941=VERTEX_POINT('',#49610);
#11942=VERTEX_POINT('',#49612);
#11943=VERTEX_POINT('',#49990);
#11944=VERTEX_POINT('',#50424);
#11945=VERTEX_POINT('',#50425);
#11946=VERTEX_POINT('',#50427);
#11947=VERTEX_POINT('',#50431);
#11948=VERTEX_POINT('',#50433);
#11949=VERTEX_POINT('',#50439);
#11950=VERTEX_POINT('',#50445);
#11951=VERTEX_POINT('',#50446);
#11952=VERTEX_POINT('',#50448);
#11953=VERTEX_POINT('',#50452);
#11954=VERTEX_POINT('',#50454);
#11955=VERTEX_POINT('',#50460);
#11956=VERTEX_POINT('',#50466);
#11957=VERTEX_POINT('',#50467);
#11958=VERTEX_POINT('',#50469);
#11959=VERTEX_POINT('',#50473);
#11960=VERTEX_POINT('',#50475);
#11961=VERTEX_POINT('',#50481);
#11962=VERTEX_POINT('',#50487);
#11963=VERTEX_POINT('',#50488);
#11964=VERTEX_POINT('',#50490);
#11965=VERTEX_POINT('',#50494);
#11966=VERTEX_POINT('',#50496);
#11967=VERTEX_POINT('',#50502);
#11968=VERTEX_POINT('',#50508);
#11969=VERTEX_POINT('',#50509);
#11970=VERTEX_POINT('',#50511);
#11971=VERTEX_POINT('',#50515);
#11972=VERTEX_POINT('',#50517);
#11973=VERTEX_POINT('',#50523);
#11974=VERTEX_POINT('',#50529);
#11975=VERTEX_POINT('',#50530);
#11976=VERTEX_POINT('',#50532);
#11977=VERTEX_POINT('',#50536);
#11978=VERTEX_POINT('',#50538);
#11979=VERTEX_POINT('',#50544);
#11980=VERTEX_POINT('',#50550);
#11981=VERTEX_POINT('',#50551);
#11982=VERTEX_POINT('',#50553);
#11983=VERTEX_POINT('',#50557);
#11984=VERTEX_POINT('',#50559);
#11985=VERTEX_POINT('',#50565);
#11986=VERTEX_POINT('',#50571);
#11987=VERTEX_POINT('',#50572);
#11988=VERTEX_POINT('',#50574);
#11989=VERTEX_POINT('',#50578);
#11990=VERTEX_POINT('',#50580);
#11991=VERTEX_POINT('',#50586);
#11992=VERTEX_POINT('',#50592);
#11993=VERTEX_POINT('',#50593);
#11994=VERTEX_POINT('',#50595);
#11995=VERTEX_POINT('',#50599);
#11996=VERTEX_POINT('',#50601);
#11997=VERTEX_POINT('',#50607);
#11998=VERTEX_POINT('',#50613);
#11999=VERTEX_POINT('',#50614);
#12000=VERTEX_POINT('',#50616);
#12001=VERTEX_POINT('',#50620);
#12002=VERTEX_POINT('',#50622);
#12003=VERTEX_POINT('',#50628);
#12004=VERTEX_POINT('',#50634);
#12005=VERTEX_POINT('',#50635);
#12006=VERTEX_POINT('',#50637);
#12007=VERTEX_POINT('',#50641);
#12008=VERTEX_POINT('',#50643);
#12009=VERTEX_POINT('',#50649);
#12010=VERTEX_POINT('',#50655);
#12011=VERTEX_POINT('',#50656);
#12012=VERTEX_POINT('',#50658);
#12013=VERTEX_POINT('',#50662);
#12014=VERTEX_POINT('',#50664);
#12015=VERTEX_POINT('',#50670);
#12016=VERTEX_POINT('',#50676);
#12017=VERTEX_POINT('',#50677);
#12018=VERTEX_POINT('',#50679);
#12019=VERTEX_POINT('',#50683);
#12020=VERTEX_POINT('',#50685);
#12021=VERTEX_POINT('',#50691);
#12022=VERTEX_POINT('',#50697);
#12023=VERTEX_POINT('',#50698);
#12024=VERTEX_POINT('',#50700);
#12025=VERTEX_POINT('',#50704);
#12026=VERTEX_POINT('',#50706);
#12027=VERTEX_POINT('',#50712);
#12028=VERTEX_POINT('',#50718);
#12029=VERTEX_POINT('',#50719);
#12030=VERTEX_POINT('',#50721);
#12031=VERTEX_POINT('',#50725);
#12032=VERTEX_POINT('',#50727);
#12033=VERTEX_POINT('',#50733);
#12034=VERTEX_POINT('',#50739);
#12035=VERTEX_POINT('',#50740);
#12036=VERTEX_POINT('',#50742);
#12037=VERTEX_POINT('',#50746);
#12038=VERTEX_POINT('',#50748);
#12039=VERTEX_POINT('',#50754);
#12040=VERTEX_POINT('',#50760);
#12041=VERTEX_POINT('',#50761);
#12042=VERTEX_POINT('',#50763);
#12043=VERTEX_POINT('',#50767);
#12044=VERTEX_POINT('',#50769);
#12045=VERTEX_POINT('',#50775);
#12046=VERTEX_POINT('',#50781);
#12047=VERTEX_POINT('',#50782);
#12048=VERTEX_POINT('',#50784);
#12049=VERTEX_POINT('',#50786);
#12050=VERTEX_POINT('',#50790);
#12051=VERTEX_POINT('',#50792);
#12052=VERTEX_POINT('',#50798);
#12053=VERTEX_POINT('',#50804);
#12054=VERTEX_POINT('',#50805);
#12055=VERTEX_POINT('',#50807);
#12056=VERTEX_POINT('',#50811);
#12057=VERTEX_POINT('',#50813);
#12058=VERTEX_POINT('',#50819);
#12059=VERTEX_POINT('',#50825);
#12060=VERTEX_POINT('',#50826);
#12061=VERTEX_POINT('',#50828);
#12062=VERTEX_POINT('',#50832);
#12063=VERTEX_POINT('',#50834);
#12064=VERTEX_POINT('',#50840);
#12065=VERTEX_POINT('',#50846);
#12066=VERTEX_POINT('',#50847);
#12067=VERTEX_POINT('',#50849);
#12068=VERTEX_POINT('',#50853);
#12069=VERTEX_POINT('',#50855);
#12070=VERTEX_POINT('',#50861);
#12071=VERTEX_POINT('',#50867);
#12072=VERTEX_POINT('',#50868);
#12073=VERTEX_POINT('',#50870);
#12074=VERTEX_POINT('',#50874);
#12075=VERTEX_POINT('',#50876);
#12076=VERTEX_POINT('',#50882);
#12077=VERTEX_POINT('',#50888);
#12078=VERTEX_POINT('',#50889);
#12079=VERTEX_POINT('',#50891);
#12080=VERTEX_POINT('',#50895);
#12081=VERTEX_POINT('',#50897);
#12082=VERTEX_POINT('',#50903);
#12083=VERTEX_POINT('',#50909);
#12084=VERTEX_POINT('',#50910);
#12085=VERTEX_POINT('',#50912);
#12086=VERTEX_POINT('',#50916);
#12087=VERTEX_POINT('',#50918);
#12088=VERTEX_POINT('',#50924);
#12089=VERTEX_POINT('',#50930);
#12090=VERTEX_POINT('',#50931);
#12091=VERTEX_POINT('',#50933);
#12092=VERTEX_POINT('',#50937);
#12093=VERTEX_POINT('',#50939);
#12094=VERTEX_POINT('',#50945);
#12095=VERTEX_POINT('',#50951);
#12096=VERTEX_POINT('',#50952);
#12097=VERTEX_POINT('',#50954);
#12098=VERTEX_POINT('',#50958);
#12099=VERTEX_POINT('',#50960);
#12100=VERTEX_POINT('',#50966);
#12101=VERTEX_POINT('',#50972);
#12102=VERTEX_POINT('',#50973);
#12103=VERTEX_POINT('',#50975);
#12104=VERTEX_POINT('',#50979);
#12105=VERTEX_POINT('',#50981);
#12106=VERTEX_POINT('',#50987);
#12107=VERTEX_POINT('',#50993);
#12108=VERTEX_POINT('',#50994);
#12109=VERTEX_POINT('',#50996);
#12110=VERTEX_POINT('',#51000);
#12111=VERTEX_POINT('',#51002);
#12112=VERTEX_POINT('',#51008);
#12113=VERTEX_POINT('',#51014);
#12114=VERTEX_POINT('',#51015);
#12115=VERTEX_POINT('',#51017);
#12116=VERTEX_POINT('',#51021);
#12117=VERTEX_POINT('',#51023);
#12118=VERTEX_POINT('',#51029);
#12119=VERTEX_POINT('',#51035);
#12120=VERTEX_POINT('',#51036);
#12121=VERTEX_POINT('',#51038);
#12122=VERTEX_POINT('',#51042);
#12123=VERTEX_POINT('',#51044);
#12124=VERTEX_POINT('',#51050);
#12125=VERTEX_POINT('',#51056);
#12126=VERTEX_POINT('',#51057);
#12127=VERTEX_POINT('',#51059);
#12128=VERTEX_POINT('',#51063);
#12129=VERTEX_POINT('',#51065);
#12130=VERTEX_POINT('',#51071);
#12131=VERTEX_POINT('',#51077);
#12132=VERTEX_POINT('',#51078);
#12133=VERTEX_POINT('',#51080);
#12134=VERTEX_POINT('',#51084);
#12135=VERTEX_POINT('',#51086);
#12136=VERTEX_POINT('',#51092);
#12137=VERTEX_POINT('',#51098);
#12138=VERTEX_POINT('',#51099);
#12139=VERTEX_POINT('',#51101);
#12140=VERTEX_POINT('',#51105);
#12141=VERTEX_POINT('',#51107);
#12142=VERTEX_POINT('',#51113);
#12143=VERTEX_POINT('',#51119);
#12144=VERTEX_POINT('',#51120);
#12145=VERTEX_POINT('',#51122);
#12146=VERTEX_POINT('',#51126);
#12147=VERTEX_POINT('',#51128);
#12148=VERTEX_POINT('',#51134);
#12149=VERTEX_POINT('',#51140);
#12150=VERTEX_POINT('',#51141);
#12151=VERTEX_POINT('',#51143);
#12152=VERTEX_POINT('',#51147);
#12153=VERTEX_POINT('',#51149);
#12154=VERTEX_POINT('',#51155);
#12155=VERTEX_POINT('',#51178);
#12156=VERTEX_POINT('',#51198);
#12157=VERTEX_POINT('',#51200);
#12158=VERTEX_POINT('',#51202);
#12159=VERTEX_POINT('',#51204);
#12160=VERTEX_POINT('',#51208);
#12161=VERTEX_POINT('',#51210);
#12162=VERTEX_POINT('',#51222);
#12163=VERTEX_POINT('',#51226);
#12164=VERTEX_POINT('',#51227);
#12165=VERTEX_POINT('',#51231);
#12166=VERTEX_POINT('',#51232);
#12167=VERTEX_POINT('',#51234);
#12168=VERTEX_POINT('',#51236);
#12169=VERTEX_POINT('',#51240);
#12170=VERTEX_POINT('',#51242);
#12171=VERTEX_POINT('',#51246);
#12172=VERTEX_POINT('',#51248);
#12173=VERTEX_POINT('',#51252);
#12174=VERTEX_POINT('',#51254);
#12175=VERTEX_POINT('',#51258);
#12176=VERTEX_POINT('',#51260);
#12177=VERTEX_POINT('',#51268);
#12178=VERTEX_POINT('',#51273);
#12179=VERTEX_POINT('',#51280);
#12180=VERTEX_POINT('',#51281);
#12181=VERTEX_POINT('',#51283);
#12182=VERTEX_POINT('',#51300);
#12183=VERTEX_POINT('',#51302);
#12184=VERTEX_POINT('',#51305);
#12185=VERTEX_POINT('',#51321);
#12186=VERTEX_POINT('',#51322);
#12187=VERTEX_POINT('',#51369);
#12188=VERTEX_POINT('',#51370);
#12189=VERTEX_POINT('',#51417);
#12190=VERTEX_POINT('',#51418);
#12191=VERTEX_POINT('',#51471);
#12192=VERTEX_POINT('',#51472);
#12193=VERTEX_POINT('',#51519);
#12194=VERTEX_POINT('',#51520);
#12195=VERTEX_POINT('',#51567);
#12196=VERTEX_POINT('',#51568);
#12197=VERTEX_POINT('',#51621);
#12198=VERTEX_POINT('',#51622);
#12199=VERTEX_POINT('',#51624);
#12200=VERTEX_POINT('',#51631);
#12201=VERTEX_POINT('',#51639);
#12202=VERTEX_POINT('',#51640);
#12203=VERTEX_POINT('',#51664);
#12204=VERTEX_POINT('',#51665);
#12205=VERTEX_POINT('',#51689);
#12206=VERTEX_POINT('',#51690);
#12207=VERTEX_POINT('',#51713);
#12208=VERTEX_POINT('',#51714);
#12209=VERTEX_POINT('',#51738);
#12210=VERTEX_POINT('',#51739);
#12211=VERTEX_POINT('',#51763);
#12212=VERTEX_POINT('',#51764);
#12213=VERTEX_POINT('',#51787);
#12214=VERTEX_POINT('',#51788);
#12215=VERTEX_POINT('',#51790);
#12216=VERTEX_POINT('',#52020);
#12217=VERTEX_POINT('',#52086);
#12218=VERTEX_POINT('',#52395);
#12219=VERTEX_POINT('',#52459);
#12220=VERTEX_POINT('',#52460);
#12221=VERTEX_POINT('',#52462);
#12222=VERTEX_POINT('',#52464);
#12223=VERTEX_POINT('',#52468);
#12224=VERTEX_POINT('',#52469);
#12225=VERTEX_POINT('',#52471);
#12226=VERTEX_POINT('',#52473);
#12227=VERTEX_POINT('',#52477);
#12228=VERTEX_POINT('',#52478);
#12229=VERTEX_POINT('',#52480);
#12230=VERTEX_POINT('',#52482);
#12231=VERTEX_POINT('',#52486);
#12232=VERTEX_POINT('',#52488);
#12233=VERTEX_POINT('',#52495);
#12234=VERTEX_POINT('',#52497);
#12235=VERTEX_POINT('',#52501);
#12236=VERTEX_POINT('',#52503);
#12237=VERTEX_POINT('',#52505);
#12238=VERTEX_POINT('',#52508);
#12239=VERTEX_POINT('',#52510);
#12240=VERTEX_POINT('',#52514);
#12241=VERTEX_POINT('',#52518);
#12242=VERTEX_POINT('',#52522);
#12243=VERTEX_POINT('',#52526);
#12244=VERTEX_POINT('',#52535);
#12245=VERTEX_POINT('',#52542);
#12246=VERTEX_POINT('',#52545);
#12247=VERTEX_POINT('',#52552);
#12248=VERTEX_POINT('',#52553);
#12249=VERTEX_POINT('',#52555);
#12250=VERTEX_POINT('',#52572);
#12251=VERTEX_POINT('',#52574);
#12252=VERTEX_POINT('',#52577);
#12253=VERTEX_POINT('',#52593);
#12254=VERTEX_POINT('',#52594);
#12255=VERTEX_POINT('',#52641);
#12256=VERTEX_POINT('',#52642);
#12257=VERTEX_POINT('',#52689);
#12258=VERTEX_POINT('',#52690);
#12259=VERTEX_POINT('',#52743);
#12260=VERTEX_POINT('',#52744);
#12261=VERTEX_POINT('',#52791);
#12262=VERTEX_POINT('',#52792);
#12263=VERTEX_POINT('',#52839);
#12264=VERTEX_POINT('',#52840);
#12265=VERTEX_POINT('',#52893);
#12266=VERTEX_POINT('',#52894);
#12267=VERTEX_POINT('',#52941);
#12268=VERTEX_POINT('',#52942);
#12269=VERTEX_POINT('',#52989);
#12270=VERTEX_POINT('',#52990);
#12271=VERTEX_POINT('',#53037);
#12272=VERTEX_POINT('',#53038);
#12273=VERTEX_POINT('',#53091);
#12274=VERTEX_POINT('',#53092);
#12275=VERTEX_POINT('',#53139);
#12276=VERTEX_POINT('',#53140);
#12277=VERTEX_POINT('',#53187);
#12278=VERTEX_POINT('',#53188);
#12279=VERTEX_POINT('',#53241);
#12280=VERTEX_POINT('',#53242);
#12281=VERTEX_POINT('',#53289);
#12282=VERTEX_POINT('',#53290);
#12283=VERTEX_POINT('',#53337);
#12284=VERTEX_POINT('',#53338);
#12285=VERTEX_POINT('',#53340);
#12286=VERTEX_POINT('',#53347);
#12287=VERTEX_POINT('',#53348);
#12288=VERTEX_POINT('',#53360);
#12289=VERTEX_POINT('',#53372);
#12290=VERTEX_POINT('',#53373);
#12291=VERTEX_POINT('',#53396);
#12292=VERTEX_POINT('',#53397);
#12293=VERTEX_POINT('',#53421);
#12294=VERTEX_POINT('',#53422);
#12295=VERTEX_POINT('',#53446);
#12296=VERTEX_POINT('',#53447);
#12297=VERTEX_POINT('',#53470);
#12298=VERTEX_POINT('',#53471);
#12299=VERTEX_POINT('',#53495);
#12300=VERTEX_POINT('',#53496);
#12301=VERTEX_POINT('',#53520);
#12302=VERTEX_POINT('',#53521);
#12303=VERTEX_POINT('',#53544);
#12304=VERTEX_POINT('',#53545);
#12305=VERTEX_POINT('',#53568);
#12306=VERTEX_POINT('',#53569);
#12307=VERTEX_POINT('',#53593);
#12308=VERTEX_POINT('',#53594);
#12309=VERTEX_POINT('',#53618);
#12310=VERTEX_POINT('',#53619);
#12311=VERTEX_POINT('',#53642);
#12312=VERTEX_POINT('',#53643);
#12313=VERTEX_POINT('',#53667);
#12314=VERTEX_POINT('',#53668);
#12315=VERTEX_POINT('',#53692);
#12316=VERTEX_POINT('',#53693);
#12317=VERTEX_POINT('',#53716);
#12318=VERTEX_POINT('',#53717);
#12319=VERTEX_POINT('',#53719);
#12320=VERTEX_POINT('',#54165);
#12321=VERTEX_POINT('',#54225);
#12322=VERTEX_POINT('',#54753);
#12323=VERTEX_POINT('',#54816);
#12324=VERTEX_POINT('',#54817);
#12325=VERTEX_POINT('',#54819);
#12326=VERTEX_POINT('',#54821);
#12327=VERTEX_POINT('',#54825);
#12328=VERTEX_POINT('',#54826);
#12329=VERTEX_POINT('',#54828);
#12330=VERTEX_POINT('',#54830);
#12331=VERTEX_POINT('',#54834);
#12332=VERTEX_POINT('',#54835);
#12333=VERTEX_POINT('',#54837);
#12334=VERTEX_POINT('',#54839);
#12335=VERTEX_POINT('',#54843);
#12336=VERTEX_POINT('',#54845);
#12337=VERTEX_POINT('',#54852);
#12338=VERTEX_POINT('',#54854);
#12339=VERTEX_POINT('',#54858);
#12340=VERTEX_POINT('',#54860);
#12341=VERTEX_POINT('',#54862);
#12342=VERTEX_POINT('',#54865);
#12343=VERTEX_POINT('',#54867);
#12344=VERTEX_POINT('',#54871);
#12345=VERTEX_POINT('',#54875);
#12346=VERTEX_POINT('',#54879);
#12347=VERTEX_POINT('',#54883);
#12348=VERTEX_POINT('',#54892);
#12349=VERTEX_POINT('',#54897);
#12350=VERTEX_POINT('',#54900);
#12351=EDGE_CURVE('',#10026,#10026,#9022,.T.);
#12352=EDGE_CURVE('',#10026,#10027,#5380,.T.);
#12353=EDGE_CURVE('',#10027,#10028,#9023,.T.);
#12354=EDGE_CURVE('',#10028,#10027,#9024,.T.);
#12355=EDGE_CURVE('',#10026,#10029,#5381,.T.);
#12356=EDGE_CURVE('',#10029,#10029,#9025,.T.);
#12357=EDGE_CURVE('',#10030,#10030,#9026,.T.);
#12358=EDGE_CURVE('',#10030,#10028,#5382,.T.);
#12359=EDGE_CURVE('',#10031,#10031,#9027,.T.);
#12360=EDGE_CURVE('',#10031,#10032,#5383,.T.);
#12361=EDGE_CURVE('',#10032,#10032,#9028,.T.);
#12362=EDGE_CURVE('',#10031,#10033,#5384,.T.);
#12363=EDGE_CURVE('',#10033,#10033,#9029,.T.);
#12364=EDGE_CURVE('',#10034,#10034,#9030,.T.);
#12365=EDGE_CURVE('',#10035,#10035,#9031,.T.);
#12366=EDGE_CURVE('',#10036,#10036,#9032,.T.);
#12367=EDGE_CURVE('',#10037,#10037,#9033,.T.);
#12368=EDGE_CURVE('',#10038,#10038,#9034,.T.);
#12369=EDGE_CURVE('',#10039,#10039,#9035,.T.);
#12370=EDGE_CURVE('',#10040,#10040,#9036,.T.);
#12371=EDGE_CURVE('',#10029,#10041,#5385,.T.);
#12372=EDGE_CURVE('',#10041,#10041,#9037,.T.);
#12373=EDGE_CURVE('',#10042,#10042,#9038,.T.);
#12374=EDGE_CURVE('',#10043,#10043,#9039,.T.);
#12375=EDGE_CURVE('',#10044,#10044,#9040,.T.);
#12376=EDGE_CURVE('',#10045,#10045,#9041,.T.);
#12377=EDGE_CURVE('',#10046,#10046,#9042,.T.);
#12378=EDGE_CURVE('',#10047,#10047,#9043,.T.);
#12379=EDGE_CURVE('',#10048,#10048,#9044,.T.);
#12380=EDGE_CURVE('',#10049,#10049,#9045,.T.);
#12381=EDGE_CURVE('',#10049,#10042,#5386,.T.);
#12382=EDGE_CURVE('',#10049,#10050,#5387,.T.);
#12383=EDGE_CURVE('',#10050,#10050,#9046,.T.);
#12384=EDGE_CURVE('',#10050,#10051,#5388,.T.);
#12385=EDGE_CURVE('',#10051,#10052,#9047,.T.);
#12386=EDGE_CURVE('',#10052,#10051,#9048,.T.);
#12387=EDGE_CURVE('',#10053,#10054,#9049,.T.);
#12388=EDGE_CURVE('',#10054,#10053,#9050,.T.);
#12389=EDGE_CURVE('',#10054,#10052,#5389,.T.);
#12390=EDGE_CURVE('',#10055,#10055,#9051,.T.);
#12391=EDGE_CURVE('',#10055,#10053,#5390,.T.);
#12392=EDGE_CURVE('',#10055,#10056,#5391,.T.);
#12393=EDGE_CURVE('',#10056,#10056,#9052,.T.);
#12394=EDGE_CURVE('',#10056,#10057,#5392,.T.);
#12395=EDGE_CURVE('',#10057,#10057,#9053,.T.);
#12396=EDGE_CURVE('',#10058,#10058,#9054,.T.);
#12397=EDGE_CURVE('',#10059,#10059,#9055,.T.);
#12398=EDGE_CURVE('',#10060,#10060,#9056,.T.);
#12399=EDGE_CURVE('',#10061,#10061,#9057,.T.);
#12400=EDGE_CURVE('',#10048,#10062,#5393,.T.);
#12401=EDGE_CURVE('',#10062,#10063,#9058,.T.);
#12402=EDGE_CURVE('',#10063,#10062,#9059,.T.);
#12403=EDGE_CURVE('',#10064,#10064,#9060,.T.);
#12404=EDGE_CURVE('',#10064,#10063,#5394,.T.);
#12405=EDGE_CURVE('',#10043,#10065,#5395,.T.);
#12406=EDGE_CURVE('',#10065,#10066,#9061,.T.);
#12407=EDGE_CURVE('',#10066,#10065,#9062,.T.);
#12408=EDGE_CURVE('',#10067,#10067,#9063,.T.);
#12409=EDGE_CURVE('',#10067,#10066,#5396,.T.);
#12410=EDGE_CURVE('',#10047,#10068,#5397,.T.);
#12411=EDGE_CURVE('',#10068,#10069,#9064,.T.);
#12412=EDGE_CURVE('',#10069,#10068,#9065,.T.);
#12413=EDGE_CURVE('',#10070,#10070,#9066,.T.);
#12414=EDGE_CURVE('',#10070,#10069,#5398,.T.);
#12415=EDGE_CURVE('',#10044,#10071,#5399,.T.);
#12416=EDGE_CURVE('',#10071,#10072,#9067,.T.);
#12417=EDGE_CURVE('',#10072,#10071,#9068,.T.);
#12418=EDGE_CURVE('',#10073,#10073,#9069,.T.);
#12419=EDGE_CURVE('',#10073,#10072,#5400,.T.);
#12420=EDGE_CURVE('',#10046,#10074,#5401,.T.);
#12421=EDGE_CURVE('',#10074,#10075,#9070,.T.);
#12422=EDGE_CURVE('',#10075,#10074,#9071,.T.);
#12423=EDGE_CURVE('',#10076,#10076,#9072,.T.);
#12424=EDGE_CURVE('',#10076,#10075,#5402,.T.);
#12425=EDGE_CURVE('',#10045,#10077,#5403,.T.);
#12426=EDGE_CURVE('',#10077,#10078,#9073,.T.);
#12427=EDGE_CURVE('',#10078,#10077,#9074,.T.);
#12428=EDGE_CURVE('',#10079,#10079,#9075,.T.);
#12429=EDGE_CURVE('',#10079,#10078,#5404,.T.);
#12430=EDGE_CURVE('',#10033,#10080,#5405,.T.);
#12431=EDGE_CURVE('',#10080,#10081,#9076,.T.);
#12432=EDGE_CURVE('',#10081,#10080,#9077,.T.);
#12433=EDGE_CURVE('',#10081,#10082,#5406,.T.);
#12434=EDGE_CURVE('',#10082,#10082,#9078,.T.);
#12435=EDGE_CURVE('',#10082,#10083,#5407,.T.);
#12436=EDGE_CURVE('',#10083,#10083,#9079,.T.);
#12437=EDGE_CURVE('',#10084,#10084,#9080,.T.);
#12438=EDGE_CURVE('',#10030,#10085,#5408,.T.);
#12439=EDGE_CURVE('',#10085,#10085,#9081,.T.);
#12440=EDGE_CURVE('',#10086,#10086,#9082,.T.);
#12441=EDGE_CURVE('',#10086,#10084,#5409,.T.);
#12442=EDGE_CURVE('',#10087,#10088,#5410,.T.);
#12443=EDGE_CURVE('',#10088,#10088,#9083,.T.);
#12444=EDGE_CURVE('',#10088,#10089,#5411,.T.);
#12445=EDGE_CURVE('',#10089,#10089,#9084,.T.);
#12446=EDGE_CURVE('',#10089,#10061,#5412,.T.);
#12447=EDGE_CURVE('',#10090,#10091,#5413,.T.);
#12448=EDGE_CURVE('',#10091,#10091,#9085,.T.);
#12449=EDGE_CURVE('',#10091,#10092,#5414,.T.);
#12450=EDGE_CURVE('',#10092,#10092,#9086,.T.);
#12451=EDGE_CURVE('',#10092,#10060,#5415,.T.);
#12452=EDGE_CURVE('',#10093,#10094,#5416,.T.);
#12453=EDGE_CURVE('',#10094,#10094,#9087,.T.);
#12454=EDGE_CURVE('',#10094,#10095,#5417,.T.);
#12455=EDGE_CURVE('',#10095,#10095,#9088,.T.);
#12456=EDGE_CURVE('',#10095,#10059,#5418,.T.);
#12457=EDGE_CURVE('',#10040,#10096,#5419,.T.);
#12458=EDGE_CURVE('',#10096,#10096,#9089,.T.);
#12459=EDGE_CURVE('',#10096,#10097,#5420,.T.);
#12460=EDGE_CURVE('',#10097,#10097,#9090,.T.);
#12461=EDGE_CURVE('',#10097,#10098,#5421,.T.);
#12462=EDGE_CURVE('',#10098,#10098,#9091,.T.);
#12463=EDGE_CURVE('',#10039,#10099,#5422,.T.);
#12464=EDGE_CURVE('',#10099,#10099,#9092,.T.);
#12465=EDGE_CURVE('',#10099,#10100,#5423,.T.);
#12466=EDGE_CURVE('',#10100,#10100,#9093,.T.);
#12467=EDGE_CURVE('',#10100,#10101,#5424,.T.);
#12468=EDGE_CURVE('',#10101,#10101,#9094,.T.);
#12469=EDGE_CURVE('',#10038,#10102,#5425,.T.);
#12470=EDGE_CURVE('',#10102,#10102,#9095,.T.);
#12471=EDGE_CURVE('',#10102,#10103,#5426,.T.);
#12472=EDGE_CURVE('',#10103,#10103,#9096,.T.);
#12473=EDGE_CURVE('',#10103,#10104,#5427,.T.);
#12474=EDGE_CURVE('',#10104,#10104,#9097,.T.);
#12475=EDGE_CURVE('',#10037,#10105,#5428,.T.);
#12476=EDGE_CURVE('',#10105,#10105,#9098,.T.);
#12477=EDGE_CURVE('',#10105,#10106,#5429,.T.);
#12478=EDGE_CURVE('',#10106,#10106,#9099,.T.);
#12479=EDGE_CURVE('',#10106,#10107,#5430,.T.);
#12480=EDGE_CURVE('',#10107,#10107,#9100,.T.);
#12481=EDGE_CURVE('',#10036,#10108,#5431,.T.);
#12482=EDGE_CURVE('',#10108,#10108,#9101,.T.);
#12483=EDGE_CURVE('',#10108,#10109,#5432,.T.);
#12484=EDGE_CURVE('',#10109,#10109,#9102,.T.);
#12485=EDGE_CURVE('',#10109,#10110,#5433,.T.);
#12486=EDGE_CURVE('',#10110,#10110,#9103,.T.);
#12487=EDGE_CURVE('',#10035,#10111,#5434,.T.);
#12488=EDGE_CURVE('',#10111,#10111,#9104,.T.);
#12489=EDGE_CURVE('',#10111,#10112,#5435,.T.);
#12490=EDGE_CURVE('',#10112,#10112,#9105,.T.);
#12491=EDGE_CURVE('',#10112,#10113,#5436,.T.);
#12492=EDGE_CURVE('',#10113,#10113,#9106,.T.);
#12493=EDGE_CURVE('',#10058,#10114,#5437,.T.);
#12494=EDGE_CURVE('',#10114,#10115,#9107,.T.);
#12495=EDGE_CURVE('',#10115,#10114,#9108,.T.);
#12496=EDGE_CURVE('',#10115,#10034,#5438,.T.);
#12497=EDGE_CURVE('',#10116,#10117,#5439,.T.);
#12498=EDGE_CURVE('',#10117,#10117,#9109,.T.);
#12499=EDGE_CURVE('',#10117,#10118,#5440,.T.);
#12500=EDGE_CURVE('',#10118,#10118,#9110,.T.);
#12501=EDGE_CURVE('',#10118,#10119,#5441,.T.);
#12502=EDGE_CURVE('',#10119,#10119,#9111,.T.);
#12503=EDGE_CURVE('',#10120,#10121,#5442,.T.);
#12504=EDGE_CURVE('',#10121,#10121,#9112,.T.);
#12505=EDGE_CURVE('',#10121,#10122,#5443,.T.);
#12506=EDGE_CURVE('',#10122,#10122,#9113,.T.);
#12507=EDGE_CURVE('',#10122,#10123,#5444,.T.);
#12508=EDGE_CURVE('',#10123,#10123,#9114,.T.);
#12509=EDGE_CURVE('',#10124,#10125,#5445,.T.);
#12510=EDGE_CURVE('',#10125,#10125,#9115,.T.);
#12511=EDGE_CURVE('',#10125,#10126,#5446,.T.);
#12512=EDGE_CURVE('',#10126,#10126,#9116,.T.);
#12513=EDGE_CURVE('',#10126,#10127,#5447,.T.);
#12514=EDGE_CURVE('',#10127,#10127,#9117,.T.);
#12515=EDGE_CURVE('',#10128,#10129,#5448,.T.);
#12516=EDGE_CURVE('',#10129,#10129,#9118,.T.);
#12517=EDGE_CURVE('',#10129,#10130,#5449,.T.);
#12518=EDGE_CURVE('',#10130,#10130,#9119,.T.);
#12519=EDGE_CURVE('',#10130,#10131,#5450,.T.);
#12520=EDGE_CURVE('',#10131,#10131,#9120,.T.);
#12521=EDGE_CURVE('',#10132,#10133,#5451,.T.);
#12522=EDGE_CURVE('',#10133,#10133,#9121,.T.);
#12523=EDGE_CURVE('',#10133,#10134,#5452,.T.);
#12524=EDGE_CURVE('',#10134,#10134,#9122,.T.);
#12525=EDGE_CURVE('',#10134,#10135,#5453,.T.);
#12526=EDGE_CURVE('',#10135,#10135,#9123,.T.);
#12527=EDGE_CURVE('',#10136,#10137,#5454,.T.);
#12528=EDGE_CURVE('',#10137,#10137,#9124,.T.);
#12529=EDGE_CURVE('',#10137,#10138,#5455,.T.);
#12530=EDGE_CURVE('',#10138,#10138,#9125,.T.);
#12531=EDGE_CURVE('',#10138,#10139,#5456,.T.);
#12532=EDGE_CURVE('',#10139,#10139,#9126,.T.);
#12533=EDGE_CURVE('',#10140,#10141,#5457,.T.);
#12534=EDGE_CURVE('',#10141,#10141,#9127,.T.);
#12535=EDGE_CURVE('',#10141,#10142,#5458,.T.);
#12536=EDGE_CURVE('',#10142,#10142,#9128,.T.);
#12537=EDGE_CURVE('',#10142,#10143,#5459,.T.);
#12538=EDGE_CURVE('',#10143,#10143,#9129,.T.);
#12539=EDGE_CURVE('',#10144,#10145,#5460,.T.);
#12540=EDGE_CURVE('',#10145,#10145,#9130,.T.);
#12541=EDGE_CURVE('',#10145,#10146,#5461,.T.);
#12542=EDGE_CURVE('',#10146,#10146,#9131,.T.);
#12543=EDGE_CURVE('',#10146,#10147,#5462,.T.);
#12544=EDGE_CURVE('',#10147,#10147,#9132,.T.);
#12545=EDGE_CURVE('',#10148,#10149,#5463,.T.);
#12546=EDGE_CURVE('',#10149,#10149,#9133,.T.);
#12547=EDGE_CURVE('',#10149,#10150,#5464,.T.);
#12548=EDGE_CURVE('',#10150,#10150,#9134,.T.);
#12549=EDGE_CURVE('',#10150,#10151,#5465,.T.);
#12550=EDGE_CURVE('',#10151,#10151,#9135,.T.);
#12551=EDGE_CURVE('',#10152,#10153,#5466,.T.);
#12552=EDGE_CURVE('',#10153,#10153,#9136,.T.);
#12553=EDGE_CURVE('',#10153,#10154,#5467,.T.);
#12554=EDGE_CURVE('',#10154,#10154,#9137,.T.);
#12555=EDGE_CURVE('',#10154,#10155,#5468,.T.);
#12556=EDGE_CURVE('',#10155,#10155,#9138,.T.);
#12557=EDGE_CURVE('',#10156,#10157,#5469,.T.);
#12558=EDGE_CURVE('',#10157,#10157,#9139,.T.);
#12559=EDGE_CURVE('',#10157,#10158,#5470,.T.);
#12560=EDGE_CURVE('',#10158,#10158,#9140,.T.);
#12561=EDGE_CURVE('',#10158,#10159,#5471,.T.);
#12562=EDGE_CURVE('',#10159,#10159,#9141,.T.);
#12563=EDGE_CURVE('',#10160,#10161,#5472,.T.);
#12564=EDGE_CURVE('',#10161,#10161,#9142,.T.);
#12565=EDGE_CURVE('',#10161,#10162,#5473,.T.);
#12566=EDGE_CURVE('',#10162,#10162,#9143,.T.);
#12567=EDGE_CURVE('',#10162,#10163,#5474,.T.);
#12568=EDGE_CURVE('',#10163,#10163,#9144,.T.);
#12569=EDGE_CURVE('',#10164,#10165,#5475,.T.);
#12570=EDGE_CURVE('',#10165,#10165,#9145,.T.);
#12571=EDGE_CURVE('',#10165,#10166,#5476,.T.);
#12572=EDGE_CURVE('',#10166,#10166,#9146,.T.);
#12573=EDGE_CURVE('',#10166,#10167,#5477,.T.);
#12574=EDGE_CURVE('',#10167,#10167,#9147,.T.);
#12575=EDGE_CURVE('',#10168,#10169,#5478,.T.);
#12576=EDGE_CURVE('',#10169,#10169,#9148,.T.);
#12577=EDGE_CURVE('',#10169,#10170,#5479,.T.);
#12578=EDGE_CURVE('',#10170,#10170,#9149,.T.);
#12579=EDGE_CURVE('',#10170,#10171,#5480,.T.);
#12580=EDGE_CURVE('',#10171,#10171,#9150,.T.);
#12581=EDGE_CURVE('',#10172,#10173,#5481,.T.);
#12582=EDGE_CURVE('',#10173,#10173,#9151,.T.);
#12583=EDGE_CURVE('',#10173,#10174,#5482,.T.);
#12584=EDGE_CURVE('',#10174,#10174,#9152,.T.);
#12585=EDGE_CURVE('',#10174,#10175,#5483,.T.);
#12586=EDGE_CURVE('',#10175,#10175,#9153,.T.);
#12587=EDGE_CURVE('',#10176,#10177,#5484,.T.);
#12588=EDGE_CURVE('',#10177,#10177,#9154,.T.);
#12589=EDGE_CURVE('',#10177,#10178,#5485,.T.);
#12590=EDGE_CURVE('',#10178,#10178,#9155,.T.);
#12591=EDGE_CURVE('',#10178,#10179,#5486,.T.);
#12592=EDGE_CURVE('',#10179,#10179,#9156,.T.);
#12593=EDGE_CURVE('',#10180,#10181,#5487,.T.);
#12594=EDGE_CURVE('',#10181,#10181,#9157,.T.);
#12595=EDGE_CURVE('',#10181,#10182,#5488,.T.);
#12596=EDGE_CURVE('',#10182,#10182,#9158,.T.);
#12597=EDGE_CURVE('',#10182,#10183,#5489,.T.);
#12598=EDGE_CURVE('',#10183,#10183,#9159,.T.);
#12599=EDGE_CURVE('',#10184,#10185,#5490,.T.);
#12600=EDGE_CURVE('',#10185,#10185,#9160,.T.);
#12601=EDGE_CURVE('',#10185,#10186,#5491,.T.);
#12602=EDGE_CURVE('',#10186,#10186,#9161,.T.);
#12603=EDGE_CURVE('',#10186,#10187,#5492,.T.);
#12604=EDGE_CURVE('',#10187,#10187,#9162,.T.);
#12605=EDGE_CURVE('',#10188,#10188,#9163,.T.);
#12606=EDGE_CURVE('',#10188,#10189,#5493,.T.);
#12607=EDGE_CURVE('',#10189,#10190,#9164,.T.);
#12608=EDGE_CURVE('',#10190,#10189,#9165,.T.);
#12609=EDGE_CURVE('',#10191,#10192,#9166,.T.);
#12610=EDGE_CURVE('',#10192,#10191,#9167,.T.);
#12611=EDGE_CURVE('',#10192,#10190,#5494,.T.);
#12612=EDGE_CURVE('',#10193,#10193,#9168,.T.);
#12613=EDGE_CURVE('',#10191,#10194,#5495,.T.);
#12614=EDGE_CURVE('',#10194,#10194,#9169,.T.);
#12615=EDGE_CURVE('',#10195,#10195,#9170,.T.);
#12616=EDGE_CURVE('',#10195,#10196,#5496,.T.);
#12617=EDGE_CURVE('',#10196,#10197,#9171,.T.);
#12618=EDGE_CURVE('',#10197,#10196,#9172,.T.);
#12619=EDGE_CURVE('',#10197,#10198,#5497,.T.);
#12620=EDGE_CURVE('',#10199,#10198,#9173,.T.);
#12621=EDGE_CURVE('',#10198,#10199,#9174,.T.);
#12622=EDGE_CURVE('',#10199,#10193,#5498,.T.);
#12623=EDGE_CURVE('',#10200,#10201,#5499,.T.);
#12624=EDGE_CURVE('',#10201,#10201,#9175,.T.);
#12625=EDGE_CURVE('',#10201,#10202,#5500,.T.);
#12626=EDGE_CURVE('',#10202,#10202,#9176,.T.);
#12627=EDGE_CURVE('',#10202,#10203,#5501,.T.);
#12628=EDGE_CURVE('',#10203,#10203,#9177,.T.);
#12629=EDGE_CURVE('',#10204,#10205,#5502,.T.);
#12630=EDGE_CURVE('',#10205,#10205,#9178,.T.);
#12631=EDGE_CURVE('',#10205,#10206,#5503,.T.);
#12632=EDGE_CURVE('',#10206,#10206,#9179,.T.);
#12633=EDGE_CURVE('',#10206,#10207,#5504,.T.);
#12634=EDGE_CURVE('',#10207,#10207,#9180,.T.);
#12635=EDGE_CURVE('',#10208,#10209,#5505,.T.);
#12636=EDGE_CURVE('',#10209,#10209,#9181,.T.);
#12637=EDGE_CURVE('',#10209,#10210,#5506,.T.);
#12638=EDGE_CURVE('',#10210,#10210,#9182,.T.);
#12639=EDGE_CURVE('',#10210,#10211,#5507,.T.);
#12640=EDGE_CURVE('',#10211,#10211,#9183,.T.);
#12641=EDGE_CURVE('',#10212,#10213,#5508,.T.);
#12642=EDGE_CURVE('',#10213,#10213,#9184,.T.);
#12643=EDGE_CURVE('',#10213,#10214,#5509,.T.);
#12644=EDGE_CURVE('',#10214,#10214,#9185,.T.);
#12645=EDGE_CURVE('',#10214,#10215,#5510,.T.);
#12646=EDGE_CURVE('',#10215,#10215,#9186,.T.);
#12647=EDGE_CURVE('',#10216,#10217,#5511,.T.);
#12648=EDGE_CURVE('',#10217,#10217,#9187,.T.);
#12649=EDGE_CURVE('',#10217,#10218,#5512,.T.);
#12650=EDGE_CURVE('',#10218,#10218,#9188,.T.);
#12651=EDGE_CURVE('',#10218,#10219,#5513,.T.);
#12652=EDGE_CURVE('',#10219,#10219,#9189,.T.);
#12653=EDGE_CURVE('',#10220,#10220,#9190,.T.);
#12654=EDGE_CURVE('',#10220,#10221,#5514,.T.);
#12655=EDGE_CURVE('',#10221,#10221,#9191,.T.);
#12656=EDGE_CURVE('',#10221,#10222,#5515,.T.);
#12657=EDGE_CURVE('',#10222,#10222,#9192,.T.);
#12658=EDGE_CURVE('',#10222,#10223,#5516,.T.);
#12659=EDGE_CURVE('',#10223,#10223,#9193,.T.);
#12660=EDGE_CURVE('',#10224,#10224,#9194,.T.);
#12661=EDGE_CURVE('',#10224,#10225,#5517,.T.);
#12662=EDGE_CURVE('',#10225,#10225,#9195,.T.);
#12663=EDGE_CURVE('',#10226,#10226,#9196,.T.);
#12664=EDGE_CURVE('',#10226,#10227,#5518,.T.);
#12665=EDGE_CURVE('',#10227,#10227,#9197,.T.);
#12666=EDGE_CURVE('',#10227,#10228,#5519,.T.);
#12667=EDGE_CURVE('',#10228,#10228,#9198,.T.);
#12668=EDGE_CURVE('',#10228,#10229,#5520,.T.);
#12669=EDGE_CURVE('',#10229,#10229,#9199,.T.);
#12670=EDGE_CURVE('',#10230,#10230,#9200,.T.);
#12671=EDGE_CURVE('',#10230,#10231,#5521,.T.);
#12672=EDGE_CURVE('',#10231,#10231,#9201,.T.);
#12673=EDGE_CURVE('',#10232,#10232,#9202,.T.);
#12674=EDGE_CURVE('',#10232,#10233,#5522,.T.);
#12675=EDGE_CURVE('',#10233,#10233,#9203,.T.);
#12676=EDGE_CURVE('',#10233,#10234,#5523,.T.);
#12677=EDGE_CURVE('',#10234,#10234,#9204,.T.);
#12678=EDGE_CURVE('',#10234,#10235,#5524,.T.);
#12679=EDGE_CURVE('',#10235,#10235,#9205,.T.);
#12680=EDGE_CURVE('',#10236,#10236,#9206,.T.);
#12681=EDGE_CURVE('',#10236,#10237,#5525,.T.);
#12682=EDGE_CURVE('',#10237,#10237,#9207,.T.);
#12683=EDGE_CURVE('',#10238,#10238,#9208,.T.);
#12684=EDGE_CURVE('',#10238,#10239,#5526,.T.);
#12685=EDGE_CURVE('',#10239,#10239,#9209,.T.);
#12686=EDGE_CURVE('',#10239,#10240,#5527,.T.);
#12687=EDGE_CURVE('',#10240,#10240,#9210,.T.);
#12688=EDGE_CURVE('',#10240,#10241,#5528,.T.);
#12689=EDGE_CURVE('',#10241,#10241,#9211,.T.);
#12690=EDGE_CURVE('',#10242,#10242,#9212,.T.);
#12691=EDGE_CURVE('',#10242,#10243,#5529,.T.);
#12692=EDGE_CURVE('',#10243,#10243,#9213,.T.);
#12693=EDGE_CURVE('',#10244,#10244,#9214,.T.);
#12694=EDGE_CURVE('',#10244,#10245,#5530,.T.);
#12695=EDGE_CURVE('',#10245,#10245,#9215,.T.);
#12696=EDGE_CURVE('',#10245,#10246,#5531,.T.);
#12697=EDGE_CURVE('',#10246,#10246,#9216,.T.);
#12698=EDGE_CURVE('',#10246,#10247,#5532,.T.);
#12699=EDGE_CURVE('',#10247,#10247,#9217,.T.);
#12700=EDGE_CURVE('',#10248,#10248,#9218,.T.);
#12701=EDGE_CURVE('',#10248,#10249,#5533,.T.);
#12702=EDGE_CURVE('',#10249,#10249,#9219,.T.);
#12703=EDGE_CURVE('',#10250,#10250,#9220,.T.);
#12704=EDGE_CURVE('',#10250,#10251,#5534,.T.);
#12705=EDGE_CURVE('',#10251,#10251,#9221,.T.);
#12706=EDGE_CURVE('',#10251,#10252,#5535,.T.);
#12707=EDGE_CURVE('',#10252,#10252,#9222,.T.);
#12708=EDGE_CURVE('',#10252,#10253,#5536,.T.);
#12709=EDGE_CURVE('',#10253,#10253,#9223,.T.);
#12710=EDGE_CURVE('',#10254,#10254,#9224,.T.);
#12711=EDGE_CURVE('',#10254,#10255,#5537,.T.);
#12712=EDGE_CURVE('',#10255,#10255,#9225,.T.);
#12713=EDGE_CURVE('',#10256,#10256,#9226,.T.);
#12714=EDGE_CURVE('',#10256,#10257,#5538,.T.);
#12715=EDGE_CURVE('',#10257,#10257,#9227,.T.);
#12716=EDGE_CURVE('',#10257,#10258,#5539,.T.);
#12717=EDGE_CURVE('',#10258,#10258,#9228,.T.);
#12718=EDGE_CURVE('',#10258,#10259,#5540,.T.);
#12719=EDGE_CURVE('',#10259,#10259,#9229,.T.);
#12720=EDGE_CURVE('',#10260,#10260,#9230,.T.);
#12721=EDGE_CURVE('',#10260,#10261,#5541,.T.);
#12722=EDGE_CURVE('',#10261,#10261,#9231,.T.);
#12723=EDGE_CURVE('',#10262,#10262,#9232,.T.);
#12724=EDGE_CURVE('',#10262,#10263,#5542,.T.);
#12725=EDGE_CURVE('',#10263,#10263,#9233,.T.);
#12726=EDGE_CURVE('',#10263,#10264,#5543,.T.);
#12727=EDGE_CURVE('',#10264,#10264,#9234,.T.);
#12728=EDGE_CURVE('',#10264,#10265,#5544,.T.);
#12729=EDGE_CURVE('',#10265,#10265,#9235,.T.);
#12730=EDGE_CURVE('',#10266,#10266,#9236,.T.);
#12731=EDGE_CURVE('',#10266,#10267,#5545,.T.);
#12732=EDGE_CURVE('',#10267,#10267,#9237,.T.);
#12733=EDGE_CURVE('',#10268,#10268,#9238,.T.);
#12734=EDGE_CURVE('',#10268,#10269,#5546,.T.);
#12735=EDGE_CURVE('',#10269,#10269,#9239,.T.);
#12736=EDGE_CURVE('',#10269,#10270,#5547,.T.);
#12737=EDGE_CURVE('',#10270,#10270,#9240,.T.);
#12738=EDGE_CURVE('',#10270,#10271,#5548,.T.);
#12739=EDGE_CURVE('',#10271,#10271,#9241,.T.);
#12740=EDGE_CURVE('',#10272,#10272,#9242,.T.);
#12741=EDGE_CURVE('',#10272,#10273,#5549,.T.);
#12742=EDGE_CURVE('',#10273,#10273,#9243,.T.);
#12743=EDGE_CURVE('',#10274,#10274,#9244,.T.);
#12744=EDGE_CURVE('',#10274,#10275,#5550,.T.);
#12745=EDGE_CURVE('',#10275,#10275,#9245,.T.);
#12746=EDGE_CURVE('',#10275,#10276,#5551,.T.);
#12747=EDGE_CURVE('',#10276,#10276,#9246,.T.);
#12748=EDGE_CURVE('',#10276,#10277,#5552,.T.);
#12749=EDGE_CURVE('',#10277,#10277,#9247,.T.);
#12750=EDGE_CURVE('',#10278,#10278,#9248,.T.);
#12751=EDGE_CURVE('',#10278,#10279,#5553,.T.);
#12752=EDGE_CURVE('',#10279,#10279,#9249,.T.);
#12753=EDGE_CURVE('',#10280,#10280,#9250,.T.);
#12754=EDGE_CURVE('',#10280,#10281,#5554,.T.);
#12755=EDGE_CURVE('',#10281,#10281,#9251,.T.);
#12756=EDGE_CURVE('',#10281,#10282,#5555,.T.);
#12757=EDGE_CURVE('',#10282,#10282,#9252,.T.);
#12758=EDGE_CURVE('',#10282,#10283,#5556,.T.);
#12759=EDGE_CURVE('',#10283,#10283,#9253,.T.);
#12760=EDGE_CURVE('',#10284,#10284,#9254,.T.);
#12761=EDGE_CURVE('',#10284,#10285,#5557,.T.);
#12762=EDGE_CURVE('',#10285,#10285,#9255,.T.);
#12763=EDGE_CURVE('',#10286,#10286,#9256,.T.);
#12764=EDGE_CURVE('',#10286,#10287,#5558,.T.);
#12765=EDGE_CURVE('',#10287,#10287,#9257,.T.);
#12766=EDGE_CURVE('',#10287,#10288,#5559,.T.);
#12767=EDGE_CURVE('',#10288,#10288,#9258,.T.);
#12768=EDGE_CURVE('',#10288,#10289,#5560,.T.);
#12769=EDGE_CURVE('',#10289,#10289,#9259,.T.);
#12770=EDGE_CURVE('',#10290,#10290,#9260,.T.);
#12771=EDGE_CURVE('',#10290,#10291,#5561,.T.);
#12772=EDGE_CURVE('',#10291,#10291,#9261,.T.);
#12773=EDGE_CURVE('',#10292,#10292,#9262,.T.);
#12774=EDGE_CURVE('',#10292,#10293,#5562,.T.);
#12775=EDGE_CURVE('',#10293,#10294,#9263,.T.);
#12776=EDGE_CURVE('',#10294,#10293,#9264,.T.);
#12777=EDGE_CURVE('',#10295,#10296,#9265,.T.);
#12778=EDGE_CURVE('',#10296,#10295,#9266,.T.);
#12779=EDGE_CURVE('',#10296,#10294,#5563,.T.);
#12780=EDGE_CURVE('',#10297,#10297,#9267,.T.);
#12781=EDGE_CURVE('',#10295,#10298,#5564,.T.);
#12782=EDGE_CURVE('',#10298,#10298,#9268,.T.);
#12783=EDGE_CURVE('',#10299,#10299,#9269,.T.);
#12784=EDGE_CURVE('',#10300,#10301,#9270,.T.);
#12785=EDGE_CURVE('',#10301,#10300,#9271,.T.);
#12786=EDGE_CURVE('',#10300,#10302,#5565,.T.);
#12787=EDGE_CURVE('',#10302,#10302,#9272,.T.);
#12788=EDGE_CURVE('',#10303,#10304,#9273,.T.);
#12789=EDGE_CURVE('',#10304,#10303,#9274,.T.);
#12790=EDGE_CURVE('',#10304,#10301,#5566,.T.);
#12791=EDGE_CURVE('',#10305,#10305,#9275,.T.);
#12792=EDGE_CURVE('',#10306,#10306,#9276,.T.);
#12793=EDGE_CURVE('',#10306,#10303,#5567,.T.);
#12794=EDGE_CURVE('',#10307,#10308,#5568,.T.);
#12795=EDGE_CURVE('',#10309,#10308,#9277,.T.);
#12796=EDGE_CURVE('',#10309,#10310,#5569,.T.);
#12797=EDGE_CURVE('',#10311,#10310,#9278,.T.);
#12798=EDGE_CURVE('',#10311,#10307,#9279,.F.);
#12799=EDGE_CURVE('',#10312,#10313,#9280,.T.);
#12800=EDGE_CURVE('',#10312,#10314,#5570,.T.);
#12801=EDGE_CURVE('',#10315,#10314,#9281,.T.);
#12802=EDGE_CURVE('',#10315,#10316,#5571,.T.);
#12803=EDGE_CURVE('',#10316,#10313,#9282,.F.);
#12804=EDGE_CURVE('',#10317,#10318,#5572,.T.);
#12805=EDGE_CURVE('',#10319,#10318,#9283,.T.);
#12806=EDGE_CURVE('',#10319,#10320,#5573,.T.);
#12807=EDGE_CURVE('',#10320,#10321,#9284,.F.);
#12808=EDGE_CURVE('',#10317,#10321,#9285,.T.);
#12809=EDGE_CURVE('',#10322,#10323,#9286,.T.);
#12810=EDGE_CURVE('',#10322,#10324,#9287,.F.);
#12811=EDGE_CURVE('',#10324,#10325,#5574,.T.);
#12812=EDGE_CURVE('',#10326,#10325,#9288,.T.);
#12813=EDGE_CURVE('',#10326,#10323,#5575,.T.);
#12814=EDGE_CURVE('',#10327,#10328,#5576,.T.);
#12815=EDGE_CURVE('',#10329,#10328,#9289,.T.);
#12816=EDGE_CURVE('',#10329,#10330,#5577,.T.);
#12817=EDGE_CURVE('',#10331,#10330,#9290,.T.);
#12818=EDGE_CURVE('',#10331,#10327,#9291,.F.);
#12819=EDGE_CURVE('',#10332,#10333,#9292,.T.);
#12820=EDGE_CURVE('',#10332,#10334,#5578,.T.);
#12821=EDGE_CURVE('',#10335,#10334,#9293,.T.);
#12822=EDGE_CURVE('',#10335,#10336,#5579,.T.);
#12823=EDGE_CURVE('',#10336,#10333,#9294,.F.);
#12824=EDGE_CURVE('',#10337,#10338,#5580,.T.);
#12825=EDGE_CURVE('',#10339,#10338,#9295,.T.);
#12826=EDGE_CURVE('',#10339,#10340,#5581,.T.);
#12827=EDGE_CURVE('',#10340,#10341,#9296,.F.);
#12828=EDGE_CURVE('',#10337,#10341,#9297,.T.);
#12829=EDGE_CURVE('',#10342,#10343,#9298,.T.);
#12830=EDGE_CURVE('',#10342,#10344,#9299,.F.);
#12831=EDGE_CURVE('',#10344,#10345,#5582,.T.);
#12832=EDGE_CURVE('',#10346,#10345,#9300,.T.);
#12833=EDGE_CURVE('',#10346,#10343,#5583,.T.);
#12834=EDGE_CURVE('',#10347,#10348,#5584,.T.);
#12835=EDGE_CURVE('',#10349,#10348,#9301,.T.);
#12836=EDGE_CURVE('',#10349,#10350,#5585,.T.);
#12837=EDGE_CURVE('',#10351,#10350,#9302,.T.);
#12838=EDGE_CURVE('',#10351,#10347,#9303,.F.);
#12839=EDGE_CURVE('',#10352,#10353,#9304,.T.);
#12840=EDGE_CURVE('',#10352,#10354,#5586,.T.);
#12841=EDGE_CURVE('',#10355,#10354,#9305,.T.);
#12842=EDGE_CURVE('',#10355,#10356,#5587,.T.);
#12843=EDGE_CURVE('',#10356,#10353,#9306,.F.);
#12844=EDGE_CURVE('',#10357,#10358,#5588,.T.);
#12845=EDGE_CURVE('',#10359,#10358,#9307,.T.);
#12846=EDGE_CURVE('',#10359,#10360,#5589,.T.);
#12847=EDGE_CURVE('',#10360,#10361,#9308,.F.);
#12848=EDGE_CURVE('',#10357,#10361,#9309,.T.);
#12849=EDGE_CURVE('',#10362,#10363,#9310,.T.);
#12850=EDGE_CURVE('',#10362,#10364,#9311,.F.);
#12851=EDGE_CURVE('',#10364,#10365,#5590,.T.);
#12852=EDGE_CURVE('',#10366,#10365,#9312,.T.);
#12853=EDGE_CURVE('',#10366,#10363,#5591,.T.);
#12854=EDGE_CURVE('',#10367,#10368,#5592,.T.);
#12855=EDGE_CURVE('',#10369,#10368,#9313,.T.);
#12856=EDGE_CURVE('',#10369,#10370,#5593,.T.);
#12857=EDGE_CURVE('',#10371,#10370,#9314,.T.);
#12858=EDGE_CURVE('',#10371,#10372,#5594,.T.);
#12859=EDGE_CURVE('',#10367,#10372,#9315,.T.);
#12860=EDGE_CURVE('',#10373,#10374,#5595,.T.);
#12861=EDGE_CURVE('',#10375,#10374,#9316,.T.);
#12862=EDGE_CURVE('',#10375,#10376,#5596,.T.);
#12863=EDGE_CURVE('',#10377,#10376,#9317,.T.);
#12864=EDGE_CURVE('',#10377,#10378,#5597,.T.);
#12865=EDGE_CURVE('',#10373,#10378,#9318,.T.);
#12866=EDGE_CURVE('',#10379,#10380,#5598,.T.);
#12867=EDGE_CURVE('',#10381,#10380,#9319,.T.);
#12868=EDGE_CURVE('',#10381,#10382,#5599,.T.);
#12869=EDGE_CURVE('',#10383,#10382,#9320,.T.);
#12870=EDGE_CURVE('',#10383,#10384,#5600,.T.);
#12871=EDGE_CURVE('',#10379,#10384,#9321,.T.);
#12872=EDGE_CURVE('',#10385,#10386,#5601,.T.);
#12873=EDGE_CURVE('',#10387,#10386,#9322,.T.);
#12874=EDGE_CURVE('',#10387,#10388,#5602,.T.);
#12875=EDGE_CURVE('',#10389,#10388,#9323,.T.);
#12876=EDGE_CURVE('',#10389,#10390,#5603,.T.);
#12877=EDGE_CURVE('',#10385,#10390,#9324,.T.);
#12878=EDGE_CURVE('',#10391,#10392,#5604,.T.);
#12879=EDGE_CURVE('',#10393,#10392,#9325,.T.);
#12880=EDGE_CURVE('',#10393,#10394,#5605,.T.);
#12881=EDGE_CURVE('',#10395,#10394,#9326,.T.);
#12882=EDGE_CURVE('',#10395,#10396,#5606,.T.);
#12883=EDGE_CURVE('',#10391,#10396,#9327,.T.);
#12884=EDGE_CURVE('',#10397,#10398,#5607,.T.);
#12885=EDGE_CURVE('',#10399,#10398,#9328,.T.);
#12886=EDGE_CURVE('',#10399,#10400,#5608,.T.);
#12887=EDGE_CURVE('',#10401,#10400,#9329,.T.);
#12888=EDGE_CURVE('',#10401,#10402,#5609,.T.);
#12889=EDGE_CURVE('',#10397,#10402,#9330,.T.);
#12890=EDGE_CURVE('',#10403,#10404,#5610,.T.);
#12891=EDGE_CURVE('',#10405,#10404,#9331,.T.);
#12892=EDGE_CURVE('',#10405,#10406,#5611,.T.);
#12893=EDGE_CURVE('',#10407,#10406,#9332,.T.);
#12894=EDGE_CURVE('',#10407,#10408,#5612,.T.);
#12895=EDGE_CURVE('',#10403,#10408,#9333,.T.);
#12896=EDGE_CURVE('',#10409,#10410,#5613,.T.);
#12897=EDGE_CURVE('',#10411,#10410,#9334,.T.);
#12898=EDGE_CURVE('',#10411,#10412,#5614,.T.);
#12899=EDGE_CURVE('',#10413,#10412,#9335,.T.);
#12900=EDGE_CURVE('',#10413,#10414,#5615,.T.);
#12901=EDGE_CURVE('',#10409,#10414,#9336,.T.);
#12902=EDGE_CURVE('',#10415,#10416,#5616,.T.);
#12903=EDGE_CURVE('',#10417,#10416,#9337,.T.);
#12904=EDGE_CURVE('',#10417,#10418,#5617,.T.);
#12905=EDGE_CURVE('',#10419,#10418,#9338,.T.);
#12906=EDGE_CURVE('',#10419,#10420,#5618,.T.);
#12907=EDGE_CURVE('',#10415,#10420,#9339,.T.);
#12908=EDGE_CURVE('',#10421,#10422,#5619,.T.);
#12909=EDGE_CURVE('',#10423,#10422,#9340,.T.);
#12910=EDGE_CURVE('',#10423,#10424,#5620,.T.);
#12911=EDGE_CURVE('',#10425,#10424,#9341,.T.);
#12912=EDGE_CURVE('',#10425,#10426,#5621,.T.);
#12913=EDGE_CURVE('',#10421,#10426,#9342,.T.);
#12914=EDGE_CURVE('',#10427,#10428,#5622,.T.);
#12915=EDGE_CURVE('',#10429,#10428,#9343,.T.);
#12916=EDGE_CURVE('',#10429,#10430,#5623,.T.);
#12917=EDGE_CURVE('',#10431,#10430,#9344,.T.);
#12918=EDGE_CURVE('',#10431,#10432,#5624,.T.);
#12919=EDGE_CURVE('',#10427,#10432,#9345,.T.);
#12920=EDGE_CURVE('',#10433,#10434,#5625,.T.);
#12921=EDGE_CURVE('',#10435,#10434,#9346,.T.);
#12922=EDGE_CURVE('',#10435,#10436,#5626,.T.);
#12923=EDGE_CURVE('',#10437,#10436,#9347,.T.);
#12924=EDGE_CURVE('',#10437,#10438,#5627,.T.);
#12925=EDGE_CURVE('',#10433,#10438,#9348,.T.);
#12926=EDGE_CURVE('',#10439,#10440,#5628,.T.);
#12927=EDGE_CURVE('',#10441,#10440,#9349,.T.);
#12928=EDGE_CURVE('',#10441,#10442,#5629,.T.);
#12929=EDGE_CURVE('',#10443,#10442,#9350,.T.);
#12930=EDGE_CURVE('',#10443,#10444,#5630,.T.);
#12931=EDGE_CURVE('',#10439,#10444,#9351,.T.);
#12932=EDGE_CURVE('',#10445,#10446,#5631,.T.);
#12933=EDGE_CURVE('',#10447,#10446,#9352,.T.);
#12934=EDGE_CURVE('',#10447,#10448,#5632,.T.);
#12935=EDGE_CURVE('',#10449,#10448,#9353,.T.);
#12936=EDGE_CURVE('',#10449,#10450,#5633,.T.);
#12937=EDGE_CURVE('',#10445,#10450,#9354,.T.);
#12938=EDGE_CURVE('',#10451,#10452,#5634,.T.);
#12939=EDGE_CURVE('',#10453,#10452,#9355,.T.);
#12940=EDGE_CURVE('',#10453,#10454,#5635,.T.);
#12941=EDGE_CURVE('',#10455,#10454,#9356,.T.);
#12942=EDGE_CURVE('',#10455,#10456,#5636,.T.);
#12943=EDGE_CURVE('',#10451,#10456,#9357,.T.);
#12944=EDGE_CURVE('',#10457,#10458,#5637,.T.);
#12945=EDGE_CURVE('',#10459,#10458,#9358,.T.);
#12946=EDGE_CURVE('',#10459,#10460,#5638,.T.);
#12947=EDGE_CURVE('',#10461,#10460,#9359,.T.);
#12948=EDGE_CURVE('',#10461,#10462,#5639,.T.);
#12949=EDGE_CURVE('',#10457,#10462,#9360,.T.);
#12950=EDGE_CURVE('',#10463,#10464,#5640,.T.);
#12951=EDGE_CURVE('',#10465,#10464,#9361,.T.);
#12952=EDGE_CURVE('',#10465,#10466,#5641,.T.);
#12953=EDGE_CURVE('',#10467,#10466,#9362,.T.);
#12954=EDGE_CURVE('',#10467,#10468,#5642,.T.);
#12955=EDGE_CURVE('',#10463,#10468,#9363,.T.);
#12956=EDGE_CURVE('',#10469,#10470,#5643,.T.);
#12957=EDGE_CURVE('',#10471,#10470,#9364,.T.);
#12958=EDGE_CURVE('',#10471,#10472,#5644,.T.);
#12959=EDGE_CURVE('',#10473,#10472,#9365,.T.);
#12960=EDGE_CURVE('',#10473,#10474,#5645,.T.);
#12961=EDGE_CURVE('',#10469,#10474,#9366,.T.);
#12962=EDGE_CURVE('',#10475,#10475,#9367,.T.);
#12963=EDGE_CURVE('',#10360,#10476,#5646,.T.);
#12964=EDGE_CURVE('',#10477,#10476,#9368,.T.);
#12965=EDGE_CURVE('',#10477,#10361,#5647,.T.);
#12966=EDGE_CURVE('',#10478,#10479,#9369,.T.);
#12967=EDGE_CURVE('',#10478,#10366,#5648,.T.);
#12968=EDGE_CURVE('',#10365,#10479,#5649,.T.);
#12969=EDGE_CURVE('',#10478,#10480,#5650,.T.);
#12970=EDGE_CURVE('',#10480,#10363,#5651,.T.);
#12971=EDGE_CURVE('',#10481,#10482,#9370,.T.);
#12972=EDGE_CURVE('',#10481,#10364,#5652,.T.);
#12973=EDGE_CURVE('',#10362,#10482,#5653,.T.);
#12974=EDGE_CURVE('',#10481,#10479,#5654,.T.);
#12975=EDGE_CURVE('',#10482,#10480,#9371,.T.);
#12976=EDGE_CURVE('',#10483,#10484,#9372,.T.);
#12977=EDGE_CURVE('',#10483,#10473,#5655,.T.);
#12978=EDGE_CURVE('',#10472,#10484,#5656,.T.);
#12979=EDGE_CURVE('',#10483,#10485,#5657,.T.);
#12980=EDGE_CURVE('',#10474,#10485,#5658,.T.);
#12981=EDGE_CURVE('',#10486,#10487,#9373,.T.);
#12982=EDGE_CURVE('',#10486,#10471,#5659,.T.);
#12983=EDGE_CURVE('',#10470,#10487,#5660,.T.);
#12984=EDGE_CURVE('',#10486,#10484,#5661,.T.);
#12985=EDGE_CURVE('',#10488,#10487,#5662,.T.);
#12986=EDGE_CURVE('',#10488,#10485,#9374,.T.);
#12987=EDGE_CURVE('',#10488,#10469,#5663,.T.);
#12988=EDGE_CURVE('',#10489,#10490,#9375,.T.);
#12989=EDGE_CURVE('',#10489,#10467,#5664,.T.);
#12990=EDGE_CURVE('',#10466,#10490,#5665,.T.);
#12991=EDGE_CURVE('',#10489,#10491,#5666,.T.);
#12992=EDGE_CURVE('',#10468,#10491,#5667,.T.);
#12993=EDGE_CURVE('',#10492,#10493,#9376,.T.);
#12994=EDGE_CURVE('',#10492,#10465,#5668,.T.);
#12995=EDGE_CURVE('',#10464,#10493,#5669,.T.);
#12996=EDGE_CURVE('',#10492,#10490,#5670,.T.);
#12997=EDGE_CURVE('',#10494,#10493,#5671,.T.);
#12998=EDGE_CURVE('',#10494,#10491,#9377,.T.);
#12999=EDGE_CURVE('',#10494,#10463,#5672,.T.);
#13000=EDGE_CURVE('',#10340,#10495,#5673,.T.);
#13001=EDGE_CURVE('',#10496,#10495,#9378,.T.);
#13002=EDGE_CURVE('',#10496,#10341,#5674,.T.);
#13003=EDGE_CURVE('',#10497,#10498,#9379,.T.);
#13004=EDGE_CURVE('',#10497,#10461,#5675,.T.);
#13005=EDGE_CURVE('',#10460,#10498,#5676,.T.);
#13006=EDGE_CURVE('',#10497,#10499,#5677,.T.);
#13007=EDGE_CURVE('',#10462,#10499,#5678,.T.);
#13008=EDGE_CURVE('',#10500,#10501,#9380,.T.);
#13009=EDGE_CURVE('',#10500,#10459,#5679,.T.);
#13010=EDGE_CURVE('',#10458,#10501,#5680,.T.);
#13011=EDGE_CURVE('',#10500,#10498,#5681,.T.);
#13012=EDGE_CURVE('',#10502,#10501,#5682,.T.);
#13013=EDGE_CURVE('',#10502,#10499,#9381,.T.);
#13014=EDGE_CURVE('',#10502,#10457,#5683,.T.);
#13015=EDGE_CURVE('',#10503,#10504,#9382,.T.);
#13016=EDGE_CURVE('',#10503,#10455,#5684,.T.);
#13017=EDGE_CURVE('',#10454,#10504,#5685,.T.);
#13018=EDGE_CURVE('',#10503,#10505,#5686,.T.);
#13019=EDGE_CURVE('',#10456,#10505,#5687,.T.);
#13020=EDGE_CURVE('',#10506,#10507,#9383,.T.);
#13021=EDGE_CURVE('',#10506,#10453,#5688,.T.);
#13022=EDGE_CURVE('',#10452,#10507,#5689,.T.);
#13023=EDGE_CURVE('',#10506,#10504,#5690,.T.);
#13024=EDGE_CURVE('',#10508,#10507,#5691,.T.);
#13025=EDGE_CURVE('',#10508,#10505,#9384,.T.);
#13026=EDGE_CURVE('',#10508,#10451,#5692,.T.);
#13027=EDGE_CURVE('',#10509,#10510,#9385,.T.);
#13028=EDGE_CURVE('',#10509,#10329,#5693,.T.);
#13029=EDGE_CURVE('',#10328,#10510,#5694,.T.);
#13030=EDGE_CURVE('',#10509,#10511,#5695,.T.);
#13031=EDGE_CURVE('',#10511,#10330,#5696,.T.);
#13032=EDGE_CURVE('',#10512,#10513,#9386,.T.);
#13033=EDGE_CURVE('',#10512,#10346,#5697,.T.);
#13034=EDGE_CURVE('',#10345,#10513,#5698,.T.);
#13035=EDGE_CURVE('',#10514,#10513,#5699,.T.);
#13036=EDGE_CURVE('',#10514,#10515,#9387,.T.);
#13037=EDGE_CURVE('',#10515,#10516,#9388,.T.);
#13038=EDGE_CURVE('',#10512,#10516,#5700,.T.);
#13039=EDGE_CURVE('',#10514,#10344,#5701,.T.);
#13040=EDGE_CURVE('',#10342,#10515,#5702,.T.);
#13041=EDGE_CURVE('',#10517,#10518,#9389,.T.);
#13042=EDGE_CURVE('',#10517,#10449,#5703,.T.);
#13043=EDGE_CURVE('',#10448,#10518,#5704,.T.);
#13044=EDGE_CURVE('',#10517,#10519,#5705,.T.);
#13045=EDGE_CURVE('',#10450,#10519,#5706,.T.);
#13046=EDGE_CURVE('',#10520,#10521,#9390,.T.);
#13047=EDGE_CURVE('',#10520,#10447,#5707,.T.);
#13048=EDGE_CURVE('',#10446,#10521,#5708,.T.);
#13049=EDGE_CURVE('',#10520,#10518,#5709,.T.);
#13050=EDGE_CURVE('',#10522,#10521,#5710,.T.);
#13051=EDGE_CURVE('',#10522,#10519,#9391,.T.);
#13052=EDGE_CURVE('',#10522,#10445,#5711,.T.);
#13053=EDGE_CURVE('',#10523,#10524,#9392,.T.);
#13054=EDGE_CURVE('',#10523,#10443,#5712,.T.);
#13055=EDGE_CURVE('',#10442,#10524,#5713,.T.);
#13056=EDGE_CURVE('',#10523,#10525,#5714,.T.);
#13057=EDGE_CURVE('',#10444,#10525,#5715,.T.);
#13058=EDGE_CURVE('',#10526,#10527,#9393,.T.);
#13059=EDGE_CURVE('',#10526,#10441,#5716,.T.);
#13060=EDGE_CURVE('',#10440,#10527,#5717,.T.);
#13061=EDGE_CURVE('',#10526,#10524,#5718,.T.);
#13062=EDGE_CURVE('',#10528,#10527,#5719,.T.);
#13063=EDGE_CURVE('',#10528,#10525,#9394,.T.);
#13064=EDGE_CURVE('',#10528,#10439,#5720,.T.);
#13065=EDGE_CURVE('',#10336,#10529,#5721,.T.);
#13066=EDGE_CURVE('',#10530,#10529,#9395,.T.);
#13067=EDGE_CURVE('',#10530,#10333,#5722,.T.);
#13068=EDGE_CURVE('',#10531,#10529,#5723,.T.);
#13069=EDGE_CURVE('',#10531,#10532,#9396,.T.);
#13070=EDGE_CURVE('',#10533,#10532,#5724,.T.);
#13071=EDGE_CURVE('',#10533,#10530,#9397,.T.);
#13072=EDGE_CURVE('',#10531,#10335,#5725,.T.);
#13073=EDGE_CURVE('',#10334,#10532,#5726,.T.);
#13074=EDGE_CURVE('',#10332,#10533,#5727,.T.);
#13075=EDGE_CURVE('',#10534,#10535,#9398,.T.);
#13076=EDGE_CURVE('',#10534,#10437,#5728,.T.);
#13077=EDGE_CURVE('',#10436,#10535,#5729,.T.);
#13078=EDGE_CURVE('',#10534,#10536,#5730,.T.);
#13079=EDGE_CURVE('',#10438,#10536,#5731,.T.);
#13080=EDGE_CURVE('',#10537,#10538,#9399,.T.);
#13081=EDGE_CURVE('',#10537,#10435,#5732,.T.);
#13082=EDGE_CURVE('',#10434,#10538,#5733,.T.);
#13083=EDGE_CURVE('',#10537,#10535,#5734,.T.);
#13084=EDGE_CURVE('',#10539,#10538,#5735,.T.);
#13085=EDGE_CURVE('',#10539,#10536,#9400,.T.);
#13086=EDGE_CURVE('',#10539,#10433,#5736,.T.);
#13087=EDGE_CURVE('',#10540,#10541,#9401,.T.);
#13088=EDGE_CURVE('',#10540,#10431,#5737,.T.);
#13089=EDGE_CURVE('',#10430,#10541,#5738,.T.);
#13090=EDGE_CURVE('',#10540,#10542,#5739,.T.);
#13091=EDGE_CURVE('',#10432,#10542,#5740,.T.);
#13092=EDGE_CURVE('',#10543,#10544,#9402,.T.);
#13093=EDGE_CURVE('',#10543,#10429,#5741,.T.);
#13094=EDGE_CURVE('',#10428,#10544,#5742,.T.);
#13095=EDGE_CURVE('',#10543,#10541,#5743,.T.);
#13096=EDGE_CURVE('',#10545,#10544,#5744,.T.);
#13097=EDGE_CURVE('',#10545,#10542,#9403,.T.);
#13098=EDGE_CURVE('',#10545,#10427,#5745,.T.);
#13099=EDGE_CURVE('',#10546,#10547,#9404,.T.);
#13100=EDGE_CURVE('',#10546,#10309,#5746,.T.);
#13101=EDGE_CURVE('',#10308,#10547,#5747,.T.);
#13102=EDGE_CURVE('',#10546,#10548,#5748,.T.);
#13103=EDGE_CURVE('',#10548,#10310,#5749,.T.);
#13104=EDGE_CURVE('',#10549,#10550,#9405,.T.);
#13105=EDGE_CURVE('',#10549,#10326,#5750,.T.);
#13106=EDGE_CURVE('',#10325,#10550,#5751,.T.);
#13107=EDGE_CURVE('',#10551,#10550,#5752,.T.);
#13108=EDGE_CURVE('',#10551,#10552,#9406,.T.);
#13109=EDGE_CURVE('',#10552,#10553,#9407,.T.);
#13110=EDGE_CURVE('',#10549,#10553,#5753,.T.);
#13111=EDGE_CURVE('',#10551,#10324,#5754,.T.);
#13112=EDGE_CURVE('',#10322,#10552,#5755,.T.);
#13113=EDGE_CURVE('',#10554,#10555,#9408,.T.);
#13114=EDGE_CURVE('',#10554,#10425,#5756,.T.);
#13115=EDGE_CURVE('',#10424,#10555,#5757,.T.);
#13116=EDGE_CURVE('',#10554,#10556,#5758,.T.);
#13117=EDGE_CURVE('',#10426,#10556,#5759,.T.);
#13118=EDGE_CURVE('',#10557,#10558,#9409,.T.);
#13119=EDGE_CURVE('',#10557,#10423,#5760,.T.);
#13120=EDGE_CURVE('',#10422,#10558,#5761,.T.);
#13121=EDGE_CURVE('',#10557,#10555,#5762,.T.);
#13122=EDGE_CURVE('',#10559,#10558,#5763,.T.);
#13123=EDGE_CURVE('',#10559,#10556,#9410,.T.);
#13124=EDGE_CURVE('',#10559,#10421,#5764,.T.);
#13125=EDGE_CURVE('',#10560,#10561,#9411,.T.);
#13126=EDGE_CURVE('',#10560,#10419,#5765,.T.);
#13127=EDGE_CURVE('',#10418,#10561,#5766,.T.);
#13128=EDGE_CURVE('',#10560,#10562,#5767,.T.);
#13129=EDGE_CURVE('',#10420,#10562,#5768,.T.);
#13130=EDGE_CURVE('',#10563,#10564,#9412,.T.);
#13131=EDGE_CURVE('',#10563,#10417,#5769,.T.);
#13132=EDGE_CURVE('',#10416,#10564,#5770,.T.);
#13133=EDGE_CURVE('',#10563,#10561,#5771,.T.);
#13134=EDGE_CURVE('',#10565,#10564,#5772,.T.);
#13135=EDGE_CURVE('',#10565,#10562,#9413,.T.);
#13136=EDGE_CURVE('',#10565,#10415,#5773,.T.);
#13137=EDGE_CURVE('',#10566,#10567,#9414,.T.);
#13138=EDGE_CURVE('',#10566,#10413,#5774,.T.);
#13139=EDGE_CURVE('',#10412,#10567,#5775,.T.);
#13140=EDGE_CURVE('',#10566,#10568,#5776,.T.);
#13141=EDGE_CURVE('',#10414,#10568,#5777,.T.);
#13142=EDGE_CURVE('',#10569,#10570,#9415,.T.);
#13143=EDGE_CURVE('',#10569,#10411,#5778,.T.);
#13144=EDGE_CURVE('',#10410,#10570,#5779,.T.);
#13145=EDGE_CURVE('',#10569,#10567,#5780,.T.);
#13146=EDGE_CURVE('',#10571,#10570,#5781,.T.);
#13147=EDGE_CURVE('',#10571,#10568,#9416,.T.);
#13148=EDGE_CURVE('',#10571,#10409,#5782,.T.);
#13149=EDGE_CURVE('',#10320,#10572,#5783,.T.);
#13150=EDGE_CURVE('',#10573,#10572,#9417,.T.);
#13151=EDGE_CURVE('',#10573,#10321,#5784,.T.);
#13152=EDGE_CURVE('',#10574,#10575,#9418,.T.);
#13153=EDGE_CURVE('',#10574,#10407,#5785,.T.);
#13154=EDGE_CURVE('',#10406,#10575,#5786,.T.);
#13155=EDGE_CURVE('',#10574,#10576,#5787,.T.);
#13156=EDGE_CURVE('',#10408,#10576,#5788,.T.);
#13157=EDGE_CURVE('',#10577,#10578,#9419,.T.);
#13158=EDGE_CURVE('',#10577,#10405,#5789,.T.);
#13159=EDGE_CURVE('',#10404,#10578,#5790,.T.);
#13160=EDGE_CURVE('',#10577,#10575,#5791,.T.);
#13161=EDGE_CURVE('',#10579,#10578,#5792,.T.);
#13162=EDGE_CURVE('',#10579,#10576,#9420,.T.);
#13163=EDGE_CURVE('',#10579,#10403,#5793,.T.);
#13164=EDGE_CURVE('',#10580,#10581,#9421,.T.);
#13165=EDGE_CURVE('',#10580,#10401,#5794,.T.);
#13166=EDGE_CURVE('',#10400,#10581,#5795,.T.);
#13167=EDGE_CURVE('',#10580,#10582,#5796,.T.);
#13168=EDGE_CURVE('',#10402,#10582,#5797,.T.);
#13169=EDGE_CURVE('',#10583,#10584,#9422,.T.);
#13170=EDGE_CURVE('',#10583,#10399,#5798,.T.);
#13171=EDGE_CURVE('',#10398,#10584,#5799,.T.);
#13172=EDGE_CURVE('',#10583,#10581,#5800,.T.);
#13173=EDGE_CURVE('',#10585,#10584,#5801,.T.);
#13174=EDGE_CURVE('',#10585,#10582,#9423,.T.);
#13175=EDGE_CURVE('',#10585,#10397,#5802,.T.);
#13176=EDGE_CURVE('',#10316,#10586,#5803,.T.);
#13177=EDGE_CURVE('',#10587,#10586,#9424,.T.);
#13178=EDGE_CURVE('',#10587,#10313,#5804,.T.);
#13179=EDGE_CURVE('',#10588,#10586,#5805,.T.);
#13180=EDGE_CURVE('',#10588,#10589,#9425,.T.);
#13181=EDGE_CURVE('',#10590,#10589,#5806,.T.);
#13182=EDGE_CURVE('',#10590,#10587,#9426,.T.);
#13183=EDGE_CURVE('',#10588,#10315,#5807,.T.);
#13184=EDGE_CURVE('',#10314,#10589,#5808,.T.);
#13185=EDGE_CURVE('',#10312,#10590,#5809,.T.);
#13186=EDGE_CURVE('',#10591,#10592,#9427,.T.);
#13187=EDGE_CURVE('',#10591,#10395,#5810,.T.);
#13188=EDGE_CURVE('',#10394,#10592,#5811,.T.);
#13189=EDGE_CURVE('',#10591,#10593,#5812,.T.);
#13190=EDGE_CURVE('',#10396,#10593,#5813,.T.);
#13191=EDGE_CURVE('',#10594,#10595,#9428,.T.);
#13192=EDGE_CURVE('',#10594,#10393,#5814,.T.);
#13193=EDGE_CURVE('',#10392,#10595,#5815,.T.);
#13194=EDGE_CURVE('',#10594,#10592,#5816,.T.);
#13195=EDGE_CURVE('',#10596,#10595,#5817,.T.);
#13196=EDGE_CURVE('',#10596,#10593,#9429,.T.);
#13197=EDGE_CURVE('',#10596,#10391,#5818,.T.);
#13198=EDGE_CURVE('',#10597,#10598,#9430,.T.);
#13199=EDGE_CURVE('',#10597,#10389,#5819,.T.);
#13200=EDGE_CURVE('',#10388,#10598,#5820,.T.);
#13201=EDGE_CURVE('',#10597,#10599,#5821,.T.);
#13202=EDGE_CURVE('',#10390,#10599,#5822,.T.);
#13203=EDGE_CURVE('',#10600,#10601,#9431,.T.);
#13204=EDGE_CURVE('',#10600,#10387,#5823,.T.);
#13205=EDGE_CURVE('',#10386,#10601,#5824,.T.);
#13206=EDGE_CURVE('',#10600,#10598,#5825,.T.);
#13207=EDGE_CURVE('',#10602,#10601,#5826,.T.);
#13208=EDGE_CURVE('',#10602,#10599,#9432,.T.);
#13209=EDGE_CURVE('',#10602,#10385,#5827,.T.);
#13210=EDGE_CURVE('',#10356,#10603,#5828,.T.);
#13211=EDGE_CURVE('',#10604,#10603,#9433,.T.);
#13212=EDGE_CURVE('',#10604,#10353,#5829,.T.);
#13213=EDGE_CURVE('',#10605,#10606,#9434,.T.);
#13214=EDGE_CURVE('',#10605,#10355,#5830,.T.);
#13215=EDGE_CURVE('',#10354,#10606,#5831,.T.);
#13216=EDGE_CURVE('',#10605,#10603,#5832,.T.);
#13217=EDGE_CURVE('',#10607,#10606,#5833,.T.);
#13218=EDGE_CURVE('',#10607,#10604,#9435,.T.);
#13219=EDGE_CURVE('',#10352,#10607,#5834,.T.);
#13220=EDGE_CURVE('',#10608,#10609,#9436,.T.);
#13221=EDGE_CURVE('',#10608,#10383,#5835,.T.);
#13222=EDGE_CURVE('',#10382,#10609,#5836,.T.);
#13223=EDGE_CURVE('',#10608,#10610,#5837,.T.);
#13224=EDGE_CURVE('',#10384,#10610,#5838,.T.);
#13225=EDGE_CURVE('',#10611,#10612,#9437,.T.);
#13226=EDGE_CURVE('',#10611,#10381,#5839,.T.);
#13227=EDGE_CURVE('',#10380,#10612,#5840,.T.);
#13228=EDGE_CURVE('',#10611,#10609,#5841,.T.);
#13229=EDGE_CURVE('',#10613,#10612,#5842,.T.);
#13230=EDGE_CURVE('',#10613,#10610,#9438,.T.);
#13231=EDGE_CURVE('',#10613,#10379,#5843,.T.);
#13232=EDGE_CURVE('',#10614,#10615,#9439,.T.);
#13233=EDGE_CURVE('',#10614,#10377,#5844,.T.);
#13234=EDGE_CURVE('',#10376,#10615,#5845,.T.);
#13235=EDGE_CURVE('',#10614,#10616,#5846,.T.);
#13236=EDGE_CURVE('',#10378,#10616,#5847,.T.);
#13237=EDGE_CURVE('',#10617,#10618,#9440,.T.);
#13238=EDGE_CURVE('',#10617,#10375,#5848,.T.);
#13239=EDGE_CURVE('',#10374,#10618,#5849,.T.);
#13240=EDGE_CURVE('',#10617,#10615,#5850,.T.);
#13241=EDGE_CURVE('',#10619,#10618,#5851,.T.);
#13242=EDGE_CURVE('',#10619,#10616,#9441,.T.);
#13243=EDGE_CURVE('',#10619,#10373,#5852,.T.);
#13244=EDGE_CURVE('',#10620,#10621,#9442,.T.);
#13245=EDGE_CURVE('',#10620,#10371,#5853,.T.);
#13246=EDGE_CURVE('',#10370,#10621,#5854,.T.);
#13247=EDGE_CURVE('',#10620,#10622,#5855,.T.);
#13248=EDGE_CURVE('',#10372,#10622,#5856,.T.);
#13249=EDGE_CURVE('',#10623,#10624,#9443,.T.);
#13250=EDGE_CURVE('',#10623,#10369,#5857,.T.);
#13251=EDGE_CURVE('',#10368,#10624,#5858,.T.);
#13252=EDGE_CURVE('',#10623,#10621,#5859,.T.);
#13253=EDGE_CURVE('',#10625,#10624,#5860,.T.);
#13254=EDGE_CURVE('',#10625,#10622,#9444,.T.);
#13255=EDGE_CURVE('',#10625,#10367,#5861,.T.);
#13256=EDGE_CURVE('',#10626,#10627,#9445,.T.);
#13257=EDGE_CURVE('',#10626,#10359,#5862,.T.);
#13258=EDGE_CURVE('',#10358,#10627,#5863,.T.);
#13259=EDGE_CURVE('',#10626,#10476,#5864,.T.);
#13260=EDGE_CURVE('',#10628,#10627,#5865,.T.);
#13261=EDGE_CURVE('',#10628,#10477,#9446,.T.);
#13262=EDGE_CURVE('',#10357,#10628,#5866,.T.);
#13263=EDGE_CURVE('',#10629,#10630,#9447,.T.);
#13264=EDGE_CURVE('',#10629,#10349,#5867,.T.);
#13265=EDGE_CURVE('',#10348,#10630,#5868,.T.);
#13266=EDGE_CURVE('',#10629,#10631,#5869,.T.);
#13267=EDGE_CURVE('',#10631,#10350,#5870,.T.);
#13268=EDGE_CURVE('',#10632,#10633,#9448,.T.);
#13269=EDGE_CURVE('',#10632,#10347,#5871,.T.);
#13270=EDGE_CURVE('',#10351,#10633,#5872,.T.);
#13271=EDGE_CURVE('',#10632,#10630,#5873,.T.);
#13272=EDGE_CURVE('',#10633,#10631,#9449,.T.);
#13273=EDGE_CURVE('',#10634,#10635,#9450,.T.);
#13274=EDGE_CURVE('',#10634,#10339,#5874,.T.);
#13275=EDGE_CURVE('',#10338,#10635,#5875,.T.);
#13276=EDGE_CURVE('',#10634,#10495,#5876,.T.);
#13277=EDGE_CURVE('',#10636,#10635,#5877,.T.);
#13278=EDGE_CURVE('',#10636,#10496,#9451,.T.);
#13279=EDGE_CURVE('',#10337,#10636,#5878,.T.);
#13280=EDGE_CURVE('',#10637,#10638,#9452,.T.);
#13281=EDGE_CURVE('',#10637,#10327,#5879,.T.);
#13282=EDGE_CURVE('',#10331,#10638,#5880,.T.);
#13283=EDGE_CURVE('',#10637,#10510,#5881,.T.);
#13284=EDGE_CURVE('',#10638,#10511,#9453,.T.);
#13285=EDGE_CURVE('',#10639,#10640,#9454,.T.);
#13286=EDGE_CURVE('',#10639,#10319,#5882,.T.);
#13287=EDGE_CURVE('',#10318,#10640,#5883,.T.);
#13288=EDGE_CURVE('',#10639,#10572,#5884,.T.);
#13289=EDGE_CURVE('',#10641,#10640,#5885,.T.);
#13290=EDGE_CURVE('',#10641,#10573,#9455,.T.);
#13291=EDGE_CURVE('',#10317,#10641,#5886,.T.);
#13292=EDGE_CURVE('',#10642,#10643,#9456,.T.);
#13293=EDGE_CURVE('',#10642,#10307,#5887,.T.);
#13294=EDGE_CURVE('',#10311,#10643,#5888,.T.);
#13295=EDGE_CURVE('',#10642,#10547,#5889,.T.);
#13296=EDGE_CURVE('',#10643,#10548,#9457,.T.);
#13297=EDGE_CURVE('',#10516,#10343,#5890,.T.);
#13298=EDGE_CURVE('',#10553,#10323,#5891,.T.);
#13299=EDGE_CURVE('',#10297,#10644,#5892,.T.);
#13300=EDGE_CURVE('',#10644,#10644,#9458,.T.);
#13301=EDGE_CURVE('',#10645,#10645,#9459,.T.);
#13302=EDGE_CURVE('',#10305,#10645,#5893,.T.);
#13303=EDGE_CURVE('',#10475,#10299,#5894,.T.);
#13304=EDGE_CURVE('',#10646,#10646,#9460,.T.);
#13305=EDGE_CURVE('',#10646,#10647,#5895,.T.);
#13306=EDGE_CURVE('',#10647,#10648,#9461,.T.);
#13307=EDGE_CURVE('',#10648,#10647,#9462,.T.);
#13308=EDGE_CURVE('',#10648,#10649,#5896,.T.);
#13309=EDGE_CURVE('',#10650,#10649,#9463,.T.);
#13310=EDGE_CURVE('',#10649,#10650,#9464,.T.);
#13311=EDGE_CURVE('',#10651,#10651,#9465,.T.);
#13312=EDGE_CURVE('',#10650,#10652,#5897,.T.);
#13313=EDGE_CURVE('',#10652,#10652,#9466,.T.);
#13314=EDGE_CURVE('',#10653,#10653,#9467,.T.);
#13315=EDGE_CURVE('',#10654,#10654,#9468,.T.);
#13316=EDGE_CURVE('',#10654,#10655,#5898,.T.);
#13317=EDGE_CURVE('',#10655,#10655,#9469,.T.);
#13318=EDGE_CURVE('',#10656,#10656,#9470,.T.);
#13319=EDGE_CURVE('',#10656,#10654,#5899,.T.);
#13320=EDGE_CURVE('',#10657,#10657,#9471,.T.);
#13321=EDGE_CURVE('',#10656,#10658,#5900,.T.);
#13322=EDGE_CURVE('',#10658,#10659,#9472,.T.);
#13323=EDGE_CURVE('',#10659,#10658,#9473,.T.);
#13324=EDGE_CURVE('',#10659,#10660,#5901,.T.);
#13325=EDGE_CURVE('',#10661,#10660,#9474,.T.);
#13326=EDGE_CURVE('',#10660,#10661,#9475,.T.);
#13327=EDGE_CURVE('',#10662,#10662,#9476,.T.);
#13328=EDGE_CURVE('',#10662,#10661,#5902,.T.);
#13329=EDGE_CURVE('',#10663,#10663,#9477,.T.);
#13330=EDGE_CURVE('',#10663,#10662,#5903,.T.);
#13331=EDGE_CURVE('',#10663,#10664,#5904,.T.);
#13332=EDGE_CURVE('',#10664,#10664,#9478,.T.);
#13333=EDGE_CURVE('',#10665,#10665,#9479,.T.);
#13334=EDGE_CURVE('',#10666,#10667,#9480,.T.);
#13335=EDGE_CURVE('',#10667,#10666,#9481,.T.);
#13336=EDGE_CURVE('',#10666,#10665,#5905,.T.);
#13337=EDGE_CURVE('',#10653,#10667,#5906,.T.);
#13338=EDGE_CURVE('',#10657,#10668,#9482,.T.);
#13339=EDGE_CURVE('',#10668,#10668,#9483,.T.);
#13340=EDGE_CURVE('',#10668,#10669,#5907,.T.);
#13341=EDGE_CURVE('',#10669,#10669,#9484,.T.);
#13342=EDGE_CURVE('',#10669,#10670,#9485,.T.);
#13343=EDGE_CURVE('',#10670,#10670,#9486,.T.);
#13344=EDGE_CURVE('',#10670,#10671,#5908,.T.);
#13345=EDGE_CURVE('',#10671,#10671,#9487,.T.);
#13346=EDGE_CURVE('',#10671,#10651,#5909,.T.);
#13347=EDGE_CURVE('',#10672,#10672,#9488,.T.);
#13348=EDGE_CURVE('',#10672,#10673,#5910,.T.);
#13349=EDGE_CURVE('',#10673,#10674,#9489,.T.);
#13350=EDGE_CURVE('',#10674,#10673,#9490,.T.);
#13351=EDGE_CURVE('',#10675,#10675,#9491,.T.);
#13352=EDGE_CURVE('',#10676,#10676,#9492,.T.);
#13353=EDGE_CURVE('',#10677,#10677,#9493,.T.);
#13354=EDGE_CURVE('',#10678,#10678,#9494,.T.);
#13355=EDGE_CURVE('',#10678,#10674,#5911,.T.);
#13356=EDGE_CURVE('',#10679,#10679,#9495,.T.);
#13357=EDGE_CURVE('',#10679,#10675,#5912,.T.);
#13358=EDGE_CURVE('',#10680,#10680,#9496,.T.);
#13359=EDGE_CURVE('',#10680,#10679,#5913,.T.);
#13360=EDGE_CURVE('',#10680,#10681,#5914,.T.);
#13361=EDGE_CURVE('',#10681,#10682,#9497,.T.);
#13362=EDGE_CURVE('',#10682,#10681,#9498,.T.);
#13363=EDGE_CURVE('',#10683,#10684,#9499,.T.);
#13364=EDGE_CURVE('',#10684,#10683,#9500,.T.);
#13365=EDGE_CURVE('',#10684,#10682,#5915,.T.);
#13366=EDGE_CURVE('',#10685,#10685,#9501,.T.);
#13367=EDGE_CURVE('',#10685,#10683,#5916,.T.);
#13368=EDGE_CURVE('',#10686,#10686,#9502,.T.);
#13369=EDGE_CURVE('',#10686,#10685,#5917,.T.);
#13370=EDGE_CURVE('',#10687,#10687,#9503,.T.);
#13371=EDGE_CURVE('',#10687,#10688,#5918,.T.);
#13372=EDGE_CURVE('',#10688,#10689,#9504,.T.);
#13373=EDGE_CURVE('',#10689,#10688,#9505,.T.);
#13374=EDGE_CURVE('',#10690,#10691,#9506,.T.);
#13375=EDGE_CURVE('',#10691,#10690,#9507,.T.);
#13376=EDGE_CURVE('',#10691,#10689,#5919,.T.);
#13377=EDGE_CURVE('',#10686,#10692,#5920,.T.);
#13378=EDGE_CURVE('',#10692,#10693,#9508,.T.);
#13379=EDGE_CURVE('',#10694,#10693,#484,.T.);
#13380=EDGE_CURVE('',#10694,#10695,#9509,.T.);
#13381=EDGE_CURVE('',#10696,#10695,#485,.T.);
#13382=EDGE_CURVE('',#10696,#10692,#9510,.T.);
#13383=EDGE_CURVE('',#10695,#10697,#9511,.T.);
#13384=EDGE_CURVE('',#10697,#10698,#5921,.T.);
#13385=EDGE_CURVE('',#10698,#10699,#9512,.T.);
#13386=EDGE_CURVE('',#10699,#10698,#9513,.T.);
#13387=EDGE_CURVE('',#10697,#10696,#9514,.T.);
#13388=EDGE_CURVE('',#10700,#10700,#9515,.T.);
#13389=EDGE_CURVE('',#10700,#10699,#5922,.T.);
#13390=EDGE_CURVE('',#10693,#10701,#9516,.T.);
#13391=EDGE_CURVE('',#10701,#10702,#5923,.T.);
#13392=EDGE_CURVE('',#10702,#10703,#9517,.T.);
#13393=EDGE_CURVE('',#10703,#10702,#9518,.T.);
#13394=EDGE_CURVE('',#10701,#10694,#9519,.T.);
#13395=EDGE_CURVE('',#10704,#10704,#9520,.T.);
#13396=EDGE_CURVE('',#10704,#10703,#5924,.T.);
#13397=EDGE_CURVE('',#10676,#10705,#5925,.T.);
#13398=EDGE_CURVE('',#10705,#10705,#9521,.T.);
#13399=EDGE_CURVE('',#10705,#10706,#5926,.T.);
#13400=EDGE_CURVE('',#10706,#10706,#9522,.T.);
#13401=EDGE_CURVE('',#10706,#10707,#5927,.T.);
#13402=EDGE_CURVE('',#10707,#10707,#9523,.T.);
#13403=EDGE_CURVE('',#10677,#10708,#5928,.T.);
#13404=EDGE_CURVE('',#10708,#10708,#9524,.T.);
#13405=EDGE_CURVE('',#10708,#10709,#5929,.T.);
#13406=EDGE_CURVE('',#10709,#10709,#9525,.T.);
#13407=EDGE_CURVE('',#10709,#10710,#5930,.T.);
#13408=EDGE_CURVE('',#10710,#10710,#9526,.T.);
#13409=EDGE_CURVE('',#10690,#10711,#5931,.T.);
#13410=EDGE_CURVE('',#10711,#10711,#9527,.T.);
#13411=EDGE_CURVE('',#10712,#10712,#9528,.T.);
#13412=EDGE_CURVE('',#10712,#10713,#5932,.T.);
#13413=EDGE_CURVE('',#10713,#10713,#9529,.T.);
#13414=EDGE_CURVE('',#10714,#10714,#9530,.T.);
#13415=EDGE_CURVE('',#10714,#10715,#5933,.T.);
#13416=EDGE_CURVE('',#10715,#10715,#9531,.T.);
#13417=EDGE_CURVE('',#10716,#10716,#9532,.T.);
#13418=EDGE_CURVE('',#10716,#10717,#5934,.T.);
#13419=EDGE_CURVE('',#10717,#10717,#9533,.T.);
#13420=EDGE_CURVE('',#10717,#10718,#5935,.T.);
#13421=EDGE_CURVE('',#10718,#10718,#9534,.T.);
#13422=EDGE_CURVE('',#10719,#10719,#9535,.T.);
#13423=EDGE_CURVE('',#10719,#10720,#5936,.T.);
#13424=EDGE_CURVE('',#10720,#10720,#9536,.T.);
#13425=EDGE_CURVE('',#10721,#10721,#9537,.T.);
#13426=EDGE_CURVE('',#10721,#10722,#5937,.T.);
#13427=EDGE_CURVE('',#10722,#10722,#9538,.T.);
#13428=EDGE_CURVE('',#10723,#10723,#9539,.T.);
#13429=EDGE_CURVE('',#10723,#10724,#5938,.T.);
#13430=EDGE_CURVE('',#10724,#10724,#9540,.T.);
#13431=EDGE_CURVE('',#10725,#10725,#9541,.T.);
#13432=EDGE_CURVE('',#10725,#10726,#5939,.T.);
#13433=EDGE_CURVE('',#10726,#10726,#9542,.T.);
#13434=EDGE_CURVE('',#10727,#10727,#9543,.T.);
#13435=EDGE_CURVE('',#10727,#10728,#5940,.T.);
#13436=EDGE_CURVE('',#10728,#10728,#9544,.T.);
#13437=EDGE_CURVE('',#10729,#10729,#9545,.T.);
#13438=EDGE_CURVE('',#10729,#10730,#5941,.T.);
#13439=EDGE_CURVE('',#10730,#10730,#9546,.T.);
#13440=EDGE_CURVE('',#10731,#10731,#9547,.T.);
#13441=EDGE_CURVE('',#10731,#10732,#5942,.T.);
#13442=EDGE_CURVE('',#10732,#10733,#9548,.T.);
#13443=EDGE_CURVE('',#10733,#10732,#9549,.T.);
#13444=EDGE_CURVE('',#10734,#10735,#9550,.T.);
#13445=EDGE_CURVE('',#10735,#10734,#9551,.T.);
#13446=EDGE_CURVE('',#10735,#10733,#5943,.T.);
#13447=EDGE_CURVE('',#10736,#10736,#9552,.T.);
#13448=EDGE_CURVE('',#10734,#10737,#5944,.T.);
#13449=EDGE_CURVE('',#10737,#10737,#9553,.T.);
#13450=EDGE_CURVE('',#10738,#10738,#9554,.T.);
#13451=EDGE_CURVE('',#10738,#10739,#5945,.T.);
#13452=EDGE_CURVE('',#10739,#10740,#9555,.T.);
#13453=EDGE_CURVE('',#10740,#10739,#9556,.T.);
#13454=EDGE_CURVE('',#10740,#10741,#5946,.T.);
#13455=EDGE_CURVE('',#10742,#10741,#9557,.T.);
#13456=EDGE_CURVE('',#10741,#10742,#9558,.T.);
#13457=EDGE_CURVE('',#10742,#10736,#5947,.T.);
#13458=EDGE_CURVE('',#10743,#10744,#5948,.T.);
#13459=EDGE_CURVE('',#10744,#10744,#9559,.T.);
#13460=EDGE_CURVE('',#10744,#10745,#5949,.T.);
#13461=EDGE_CURVE('',#10745,#10745,#9560,.T.);
#13462=EDGE_CURVE('',#10746,#10747,#5950,.T.);
#13463=EDGE_CURVE('',#10747,#10747,#9561,.T.);
#13464=EDGE_CURVE('',#10747,#10748,#5951,.T.);
#13465=EDGE_CURVE('',#10748,#10748,#9562,.T.);
#13466=EDGE_CURVE('',#10749,#10749,#9563,.T.);
#13467=EDGE_CURVE('',#10749,#10750,#5952,.T.);
#13468=EDGE_CURVE('',#10750,#10750,#9564,.T.);
#13469=EDGE_CURVE('',#10751,#10751,#9565,.T.);
#13470=EDGE_CURVE('',#10752,#10752,#9566,.T.);
#13471=EDGE_CURVE('',#10752,#10751,#5953,.T.);
#13472=EDGE_CURVE('',#10753,#10753,#9567,.T.);
#13473=EDGE_CURVE('',#10753,#10752,#5954,.T.);
#13474=EDGE_CURVE('',#10754,#10754,#9568,.T.);
#13475=EDGE_CURVE('',#10754,#10755,#5955,.T.);
#13476=EDGE_CURVE('',#10755,#10755,#9569,.T.);
#13477=EDGE_CURVE('',#10756,#10756,#9570,.T.);
#13478=EDGE_CURVE('',#10757,#10757,#9571,.T.);
#13479=EDGE_CURVE('',#10758,#10758,#9572,.T.);
#13480=EDGE_CURVE('',#10758,#10757,#5956,.T.);
#13481=EDGE_CURVE('',#10759,#10759,#9573,.T.);
#13482=EDGE_CURVE('',#10760,#10760,#9574,.T.);
#13483=EDGE_CURVE('',#10760,#10759,#5957,.T.);
#13484=EDGE_CURVE('',#10756,#10760,#5958,.T.);
#13485=EDGE_CURVE('',#10761,#10761,#9575,.T.);
#13486=EDGE_CURVE('',#10761,#10758,#5959,.T.);
#13487=EDGE_CURVE('',#10762,#10762,#9576,.T.);
#13488=EDGE_CURVE('',#10763,#10763,#9577,.T.);
#13489=EDGE_CURVE('',#10763,#10762,#5960,.T.);
#13490=EDGE_CURVE('',#10764,#10764,#9578,.T.);
#13491=EDGE_CURVE('',#10765,#10765,#9579,.T.);
#13492=EDGE_CURVE('',#10765,#10764,#5961,.T.);
#13493=EDGE_CURVE('',#10766,#10766,#9580,.T.);
#13494=EDGE_CURVE('',#10766,#10765,#5962,.T.);
#13495=EDGE_CURVE('',#10767,#10767,#9581,.T.);
#13496=EDGE_CURVE('',#10767,#10768,#5963,.T.);
#13497=EDGE_CURVE('',#10768,#10769,#9582,.T.);
#13498=EDGE_CURVE('',#10769,#10768,#9583,.T.);
#13499=EDGE_CURVE('',#10770,#10770,#9584,.T.);
#13500=EDGE_CURVE('',#10769,#10771,#5964,.T.);
#13501=EDGE_CURVE('',#10771,#10771,#9585,.T.);
#13502=EDGE_CURVE('',#10772,#10773,#9586,.T.);
#13503=EDGE_CURVE('',#10773,#10772,#9587,.T.);
#13504=EDGE_CURVE('',#10772,#10770,#5965,.T.);
#13505=EDGE_CURVE('',#10773,#10774,#5966,.T.);
#13506=EDGE_CURVE('',#10775,#10774,#9588,.T.);
#13507=EDGE_CURVE('',#10776,#10775,#486,.T.);
#13508=EDGE_CURVE('',#10776,#10777,#5967,.T.);
#13509=EDGE_CURVE('',#10778,#10777,#487,.T.);
#13510=EDGE_CURVE('',#10778,#10779,#5968,.T.);
#13511=EDGE_CURVE('',#10780,#10779,#488,.T.);
#13512=EDGE_CURVE('',#10774,#10780,#9589,.T.);
#13513=EDGE_CURVE('',#10781,#10781,#9590,.T.);
#13514=EDGE_CURVE('',#10781,#10782,#5969,.T.);
#13515=EDGE_CURVE('',#10782,#10775,#489,.T.);
#13516=EDGE_CURVE('',#10780,#10782,#490,.T.);
#13517=EDGE_CURVE('',#10779,#10783,#491,.F.);
#13518=EDGE_CURVE('',#10783,#10784,#492,.T.);
#13519=EDGE_CURVE('',#10784,#10776,#493,.F.);
#13520=EDGE_CURVE('',#10785,#10785,#9591,.T.);
#13521=EDGE_CURVE('',#10786,#10787,#494,.T.);
#13522=EDGE_CURVE('',#10787,#10788,#495,.T.);
#13523=EDGE_CURVE('',#10788,#10789,#496,.T.);
#13524=EDGE_CURVE('',#10789,#10790,#5970,.T.);
#13525=EDGE_CURVE('',#10790,#10791,#497,.T.);
#13526=EDGE_CURVE('',#10791,#10790,#498,.T.);
#13527=EDGE_CURVE('',#10789,#10792,#499,.T.);
#13528=EDGE_CURVE('',#10793,#10792,#500,.T.);
#13529=EDGE_CURVE('',#10793,#10786,#501,.T.);
#13530=EDGE_CURVE('',#10786,#10788,#9592,.T.);
#13531=EDGE_CURVE('',#10792,#10793,#9593,.T.);
#13532=EDGE_CURVE('',#10787,#10785,#5971,.T.);
#13533=EDGE_CURVE('',#10794,#10795,#502,.T.);
#13534=EDGE_CURVE('',#10784,#10794,#9594,.T.);
#13535=EDGE_CURVE('',#10796,#10783,#9595,.T.);
#13536=EDGE_CURVE('',#10796,#10791,#5972,.T.);
#13537=EDGE_CURVE('',#10795,#10796,#9596,.T.);
#13538=EDGE_CURVE('',#10777,#10794,#503,.F.);
#13539=EDGE_CURVE('',#10795,#10778,#504,.F.);
#13540=EDGE_CURVE('',#10797,#10797,#9597,.T.);
#13541=EDGE_CURVE('',#10797,#10798,#5973,.T.);
#13542=EDGE_CURVE('',#10798,#10798,#9598,.T.);
#13543=EDGE_CURVE('',#10798,#10799,#5974,.T.);
#13544=EDGE_CURVE('',#10799,#10799,#9599,.T.);
#13545=EDGE_CURVE('',#10800,#10800,#9600,.T.);
#13546=EDGE_CURVE('',#10801,#10801,#9601,.T.);
#13547=EDGE_CURVE('',#10802,#10802,#9602,.T.);
#13548=EDGE_CURVE('',#10803,#10803,#9603,.T.);
#13549=EDGE_CURVE('',#10803,#10799,#5975,.T.);
#13550=EDGE_CURVE('',#10804,#10804,#9604,.T.);
#13551=EDGE_CURVE('',#10805,#10805,#9605,.T.);
#13552=EDGE_CURVE('',#10806,#10806,#9606,.T.);
#13553=EDGE_CURVE('',#10801,#10807,#5976,.T.);
#13554=EDGE_CURVE('',#10807,#10807,#9607,.T.);
#13555=EDGE_CURVE('',#10807,#10808,#5977,.T.);
#13556=EDGE_CURVE('',#10808,#10808,#9608,.T.);
#13557=EDGE_CURVE('',#10805,#10808,#5978,.T.);
#13558=EDGE_CURVE('',#10802,#10809,#5979,.T.);
#13559=EDGE_CURVE('',#10809,#10809,#9609,.T.);
#13560=EDGE_CURVE('',#10809,#10810,#5980,.T.);
#13561=EDGE_CURVE('',#10810,#10810,#9610,.T.);
#13562=EDGE_CURVE('',#10806,#10810,#5981,.T.);
#13563=EDGE_CURVE('',#10804,#10811,#5982,.T.);
#13564=EDGE_CURVE('',#10811,#10812,#9611,.T.);
#13565=EDGE_CURVE('',#10812,#10811,#9612,.T.);
#13566=EDGE_CURVE('',#10812,#10813,#5983,.T.);
#13567=EDGE_CURVE('',#10814,#10813,#9613,.T.);
#13568=EDGE_CURVE('',#10813,#10814,#9614,.T.);
#13569=EDGE_CURVE('',#10814,#10800,#5984,.T.);
#13570=EDGE_CURVE('',#10815,#10815,#9615,.T.);
#13571=EDGE_CURVE('',#10815,#10816,#5985,.T.);
#13572=EDGE_CURVE('',#10816,#10817,#9616,.T.);
#13573=EDGE_CURVE('',#10817,#10816,#9617,.T.);
#13574=EDGE_CURVE('',#10818,#10819,#9618,.T.);
#13575=EDGE_CURVE('',#10819,#10818,#9619,.T.);
#13576=EDGE_CURVE('',#10819,#10817,#5986,.T.);
#13577=EDGE_CURVE('',#10820,#10821,#9620,.T.);
#13578=EDGE_CURVE('',#10822,#10820,#9621,.T.);
#13579=EDGE_CURVE('',#10823,#10822,#9622,.T.);
#13580=EDGE_CURVE('',#10822,#10823,#9623,.T.);
#13581=EDGE_CURVE('',#10824,#10822,#9624,.T.);
#13582=EDGE_CURVE('',#10825,#10824,#9625,.T.);
#13583=EDGE_CURVE('',#10824,#10825,#9626,.T.);
#13584=EDGE_CURVE('',#10820,#10824,#9627,.T.);
#13585=EDGE_CURVE('',#10821,#10820,#9628,.T.);
#13586=EDGE_CURVE('',#10818,#10826,#5987,.T.);
#13587=EDGE_CURVE('',#10826,#10826,#9629,.T.);
#13588=EDGE_CURVE('',#10827,#10827,#9630,.T.);
#13589=EDGE_CURVE('',#10828,#10828,#9631,.T.);
#13590=EDGE_CURVE('',#10829,#10829,#9632,.T.);
#13591=EDGE_CURVE('',#10830,#10830,#9633,.T.);
#13592=EDGE_CURVE('',#10831,#10832,#9634,.T.);
#13593=EDGE_CURVE('',#10832,#10831,#9635,.T.);
#13594=EDGE_CURVE('',#10831,#10822,#5988,.T.);
#13595=EDGE_CURVE('',#10833,#10834,#9636,.T.);
#13596=EDGE_CURVE('',#10834,#10833,#9637,.T.);
#13597=EDGE_CURVE('',#10834,#10832,#5989,.T.);
#13598=EDGE_CURVE('',#10823,#10835,#5990,.T.);
#13599=EDGE_CURVE('',#10835,#10835,#9638,.T.);
#13600=EDGE_CURVE('',#10835,#10836,#5991,.T.);
#13601=EDGE_CURVE('',#10836,#10836,#9639,.T.);
#13602=EDGE_CURVE('',#10828,#10836,#5992,.T.);
#13603=EDGE_CURVE('',#10821,#10837,#5993,.T.);
#13604=EDGE_CURVE('',#10837,#10837,#9640,.T.);
#13605=EDGE_CURVE('',#10837,#10838,#5994,.T.);
#13606=EDGE_CURVE('',#10838,#10838,#9641,.T.);
#13607=EDGE_CURVE('',#10830,#10838,#5995,.T.);
#13608=EDGE_CURVE('',#10825,#10839,#5996,.T.);
#13609=EDGE_CURVE('',#10839,#10839,#9642,.T.);
#13610=EDGE_CURVE('',#10839,#10840,#5997,.T.);
#13611=EDGE_CURVE('',#10840,#10840,#9643,.T.);
#13612=EDGE_CURVE('',#10829,#10840,#5998,.T.);
#13613=EDGE_CURVE('',#10827,#10833,#5999,.T.);
#13614=EDGE_CURVE('',#10841,#10842,#6000,.T.);
#13615=EDGE_CURVE('',#10843,#10841,#6001,.T.);
#13616=EDGE_CURVE('',#10844,#10843,#6002,.T.);
#13617=EDGE_CURVE('',#10842,#10844,#6003,.T.);
#13618=EDGE_CURVE('',#10845,#10846,#6004,.T.);
#13619=EDGE_CURVE('',#10847,#10845,#6005,.T.);
#13620=EDGE_CURVE('',#10847,#10848,#6006,.T.);
#13621=EDGE_CURVE('',#10846,#10848,#6007,.T.);
#13622=EDGE_CURVE('',#10844,#10847,#6008,.T.);
#13623=EDGE_CURVE('',#10848,#10843,#6009,.T.);
#13624=EDGE_CURVE('',#10842,#10845,#9644,.T.);
#13625=EDGE_CURVE('',#10849,#10849,#9645,.T.);
#13626=EDGE_CURVE('',#10850,#10850,#9646,.T.);
#13627=EDGE_CURVE('',#10851,#10851,#9647,.T.);
#13628=EDGE_CURVE('',#10852,#10853,#6010,.T.);
#13629=EDGE_CURVE('',#10853,#10854,#9648,.T.);
#13630=EDGE_CURVE('',#10854,#10855,#6011,.T.);
#13631=EDGE_CURVE('',#10855,#10852,#9649,.T.);
#13632=EDGE_CURVE('',#10856,#10857,#6012,.T.);
#13633=EDGE_CURVE('',#10857,#10858,#9650,.T.);
#13634=EDGE_CURVE('',#10858,#10859,#6013,.T.);
#13635=EDGE_CURVE('',#10859,#10856,#9651,.T.);
#13636=EDGE_CURVE('',#10860,#10861,#6014,.T.);
#13637=EDGE_CURVE('',#10861,#10862,#9652,.T.);
#13638=EDGE_CURVE('',#10862,#10863,#6015,.T.);
#13639=EDGE_CURVE('',#10863,#10860,#9653,.T.);
#13640=EDGE_CURVE('',#10864,#10865,#6016,.T.);
#13641=EDGE_CURVE('',#10865,#10866,#9654,.T.);
#13642=EDGE_CURVE('',#10866,#10867,#6017,.T.);
#13643=EDGE_CURVE('',#10867,#10864,#9655,.T.);
#13644=EDGE_CURVE('',#10868,#10869,#6018,.T.);
#13645=EDGE_CURVE('',#10869,#10870,#9656,.T.);
#13646=EDGE_CURVE('',#10870,#10871,#6019,.T.);
#13647=EDGE_CURVE('',#10871,#10868,#9657,.T.);
#13648=EDGE_CURVE('',#10872,#10873,#6020,.T.);
#13649=EDGE_CURVE('',#10873,#10874,#9658,.T.);
#13650=EDGE_CURVE('',#10874,#10875,#6021,.T.);
#13651=EDGE_CURVE('',#10875,#10872,#9659,.T.);
#13652=EDGE_CURVE('',#10876,#10876,#9660,.T.);
#13653=EDGE_CURVE('',#10841,#10846,#9661,.T.);
#13654=EDGE_CURVE('',#10877,#10877,#9662,.T.);
#13655=EDGE_CURVE('',#10877,#10849,#6022,.T.);
#13656=EDGE_CURVE('',#10878,#10878,#9663,.T.);
#13657=EDGE_CURVE('',#10878,#10876,#6023,.T.);
#13658=EDGE_CURVE('',#10879,#10879,#9664,.T.);
#13659=EDGE_CURVE('',#10879,#10850,#6024,.T.);
#13660=EDGE_CURVE('',#10872,#10880,#6025,.T.);
#13661=EDGE_CURVE('',#10881,#10880,#6026,.T.);
#13662=EDGE_CURVE('',#10873,#10881,#6027,.T.);
#13663=EDGE_CURVE('',#10875,#10882,#6028,.T.);
#13664=EDGE_CURVE('',#10880,#10882,#9665,.T.);
#13665=EDGE_CURVE('',#10874,#10883,#6029,.T.);
#13666=EDGE_CURVE('',#10882,#10883,#6030,.T.);
#13667=EDGE_CURVE('',#10883,#10881,#9666,.T.);
#13668=EDGE_CURVE('',#10868,#10884,#6031,.T.);
#13669=EDGE_CURVE('',#10885,#10884,#6032,.T.);
#13670=EDGE_CURVE('',#10869,#10885,#6033,.T.);
#13671=EDGE_CURVE('',#10871,#10886,#6034,.T.);
#13672=EDGE_CURVE('',#10884,#10886,#9667,.T.);
#13673=EDGE_CURVE('',#10870,#10887,#6035,.T.);
#13674=EDGE_CURVE('',#10886,#10887,#6036,.T.);
#13675=EDGE_CURVE('',#10887,#10885,#9668,.T.);
#13676=EDGE_CURVE('',#10864,#10888,#6037,.T.);
#13677=EDGE_CURVE('',#10889,#10888,#6038,.T.);
#13678=EDGE_CURVE('',#10865,#10889,#6039,.T.);
#13679=EDGE_CURVE('',#10867,#10890,#6040,.T.);
#13680=EDGE_CURVE('',#10888,#10890,#9669,.T.);
#13681=EDGE_CURVE('',#10866,#10891,#6041,.T.);
#13682=EDGE_CURVE('',#10890,#10891,#6042,.T.);
#13683=EDGE_CURVE('',#10891,#10889,#9670,.T.);
#13684=EDGE_CURVE('',#10860,#10892,#6043,.T.);
#13685=EDGE_CURVE('',#10893,#10892,#6044,.T.);
#13686=EDGE_CURVE('',#10861,#10893,#6045,.T.);
#13687=EDGE_CURVE('',#10863,#10894,#6046,.T.);
#13688=EDGE_CURVE('',#10892,#10894,#9671,.T.);
#13689=EDGE_CURVE('',#10862,#10895,#6047,.T.);
#13690=EDGE_CURVE('',#10894,#10895,#6048,.T.);
#13691=EDGE_CURVE('',#10895,#10893,#9672,.T.);
#13692=EDGE_CURVE('',#10856,#10896,#6049,.T.);
#13693=EDGE_CURVE('',#10897,#10896,#6050,.T.);
#13694=EDGE_CURVE('',#10857,#10897,#6051,.T.);
#13695=EDGE_CURVE('',#10859,#10898,#6052,.T.);
#13696=EDGE_CURVE('',#10896,#10898,#9673,.T.);
#13697=EDGE_CURVE('',#10858,#10899,#6053,.T.);
#13698=EDGE_CURVE('',#10898,#10899,#6054,.T.);
#13699=EDGE_CURVE('',#10899,#10897,#9674,.T.);
#13700=EDGE_CURVE('',#10852,#10900,#6055,.T.);
#13701=EDGE_CURVE('',#10901,#10900,#6056,.T.);
#13702=EDGE_CURVE('',#10853,#10901,#6057,.T.);
#13703=EDGE_CURVE('',#10855,#10902,#6058,.T.);
#13704=EDGE_CURVE('',#10900,#10902,#9675,.T.);
#13705=EDGE_CURVE('',#10854,#10903,#6059,.T.);
#13706=EDGE_CURVE('',#10902,#10903,#6060,.T.);
#13707=EDGE_CURVE('',#10903,#10901,#9676,.T.);
#13708=EDGE_CURVE('',#10904,#10904,#9677,.T.);
#13709=EDGE_CURVE('',#10904,#10851,#6061,.T.);
#13710=EDGE_CURVE('',#10905,#10906,#6062,.T.);
#13711=EDGE_CURVE('',#10906,#10907,#6063,.T.);
#13712=EDGE_CURVE('',#10907,#10908,#6064,.T.);
#13713=EDGE_CURVE('',#10908,#10905,#6065,.T.);
#13714=EDGE_CURVE('',#10906,#10909,#6066,.T.);
#13715=EDGE_CURVE('',#10910,#10909,#6067,.T.);
#13716=EDGE_CURVE('',#10907,#10910,#6068,.T.);
#13717=EDGE_CURVE('',#10905,#10911,#6069,.T.);
#13718=EDGE_CURVE('',#10912,#10911,#6070,.T.);
#13719=EDGE_CURVE('',#10912,#10913,#6071,.T.);
#13720=EDGE_CURVE('',#10914,#10913,#6072,.T.);
#13721=EDGE_CURVE('',#10915,#10914,#6073,.T.);
#13722=EDGE_CURVE('',#10916,#10915,#6074,.T.);
#13723=EDGE_CURVE('',#10917,#10916,#6075,.T.);
#13724=EDGE_CURVE('',#10918,#10917,#6076,.T.);
#13725=EDGE_CURVE('',#10918,#10919,#6077,.T.);
#13726=EDGE_CURVE('',#10920,#10919,#6078,.T.);
#13727=EDGE_CURVE('',#10920,#10921,#6079,.T.);
#13728=EDGE_CURVE('',#10922,#10921,#6080,.T.);
#13729=EDGE_CURVE('',#10922,#10923,#6081,.T.);
#13730=EDGE_CURVE('',#10909,#10923,#6082,.T.);
#13731=EDGE_CURVE('',#10915,#10924,#6083,.T.);
#13732=EDGE_CURVE('',#10924,#10925,#6084,.T.);
#13733=EDGE_CURVE('',#10925,#10916,#6085,.T.);
#13734=EDGE_CURVE('',#10926,#10925,#6086,.T.);
#13735=EDGE_CURVE('',#10917,#10926,#6087,.T.);
#13736=EDGE_CURVE('',#10927,#10910,#6088,.T.);
#13737=EDGE_CURVE('',#10927,#10928,#6089,.T.);
#13738=EDGE_CURVE('',#10929,#10928,#6090,.T.);
#13739=EDGE_CURVE('',#10929,#10930,#6091,.T.);
#13740=EDGE_CURVE('',#10931,#10930,#6092,.T.);
#13741=EDGE_CURVE('',#10931,#10932,#6093,.T.);
#13742=EDGE_CURVE('',#10926,#10932,#6094,.T.);
#13743=EDGE_CURVE('',#10933,#10924,#6095,.T.);
#13744=EDGE_CURVE('',#10934,#10933,#6096,.T.);
#13745=EDGE_CURVE('',#10935,#10934,#6097,.T.);
#13746=EDGE_CURVE('',#10936,#10935,#6098,.T.);
#13747=EDGE_CURVE('',#10936,#10908,#6099,.T.);
#13748=EDGE_CURVE('',#10923,#10927,#6100,.T.);
#13749=EDGE_CURVE('',#10928,#10922,#6101,.T.);
#13750=EDGE_CURVE('',#10937,#10938,#6102,.T.);
#13751=EDGE_CURVE('',#10938,#10939,#6103,.T.);
#13752=EDGE_CURVE('',#10939,#10940,#6104,.T.);
#13753=EDGE_CURVE('',#10940,#10937,#6105,.T.);
#13754=EDGE_CURVE('',#10921,#10929,#6106,.T.);
#13755=EDGE_CURVE('',#10930,#10920,#6107,.T.);
#13756=EDGE_CURVE('',#10932,#10918,#6108,.T.);
#13757=EDGE_CURVE('',#10919,#10931,#6109,.T.);
#13758=EDGE_CURVE('',#10941,#10942,#6110,.T.);
#13759=EDGE_CURVE('',#10942,#10943,#6111,.T.);
#13760=EDGE_CURVE('',#10943,#10944,#6112,.T.);
#13761=EDGE_CURVE('',#10944,#10941,#6113,.T.);
#13762=EDGE_CURVE('',#10913,#10934,#6114,.T.);
#13763=EDGE_CURVE('',#10933,#10914,#6115,.T.);
#13764=EDGE_CURVE('',#10945,#10946,#6116,.T.);
#13765=EDGE_CURVE('',#10946,#10947,#6117,.T.);
#13766=EDGE_CURVE('',#10948,#10947,#6118,.T.);
#13767=EDGE_CURVE('',#10945,#10948,#6119,.T.);
#13768=EDGE_CURVE('',#10949,#10949,#9678,.T.);
#13769=EDGE_CURVE('',#10950,#10950,#9679,.T.);
#13770=EDGE_CURVE('',#10935,#10912,#6120,.T.);
#13771=EDGE_CURVE('',#10911,#10936,#6121,.T.);
#13772=EDGE_CURVE('',#10951,#10951,#9680,.T.);
#13773=EDGE_CURVE('',#10951,#10950,#6122,.T.);
#13774=EDGE_CURVE('',#10952,#10952,#9681,.T.);
#13775=EDGE_CURVE('',#10952,#10949,#6123,.T.);
#13776=EDGE_CURVE('',#10953,#10945,#6124,.T.);
#13777=EDGE_CURVE('',#10954,#10948,#6125,.T.);
#13778=EDGE_CURVE('',#10953,#10954,#6126,.T.);
#13779=EDGE_CURVE('',#10955,#10953,#6127,.T.);
#13780=EDGE_CURVE('',#10956,#10954,#6128,.T.);
#13781=EDGE_CURVE('',#10955,#10956,#6129,.T.);
#13782=EDGE_CURVE('',#10946,#10955,#6130,.T.);
#13783=EDGE_CURVE('',#10947,#10956,#6131,.T.);
#13784=EDGE_CURVE('',#10957,#10958,#6132,.T.);
#13785=EDGE_CURVE('',#10957,#10938,#6133,.T.);
#13786=EDGE_CURVE('',#10958,#10937,#6134,.T.);
#13787=EDGE_CURVE('',#10959,#10957,#6135,.T.);
#13788=EDGE_CURVE('',#10959,#10939,#6136,.T.);
#13789=EDGE_CURVE('',#10960,#10959,#6137,.T.);
#13790=EDGE_CURVE('',#10960,#10940,#6138,.T.);
#13791=EDGE_CURVE('',#10958,#10960,#6139,.T.);
#13792=EDGE_CURVE('',#10941,#10961,#6140,.T.);
#13793=EDGE_CURVE('',#10961,#10962,#6141,.T.);
#13794=EDGE_CURVE('',#10942,#10962,#6142,.T.);
#13795=EDGE_CURVE('',#10944,#10963,#6143,.T.);
#13796=EDGE_CURVE('',#10963,#10961,#6144,.T.);
#13797=EDGE_CURVE('',#10943,#10964,#6145,.T.);
#13798=EDGE_CURVE('',#10964,#10963,#6146,.T.);
#13799=EDGE_CURVE('',#10962,#10964,#6147,.T.);
#13800=EDGE_CURVE('',#10965,#10966,#9682,.T.);
#13801=EDGE_CURVE('',#10966,#10967,#6148,.T.);
#13802=EDGE_CURVE('',#10967,#10968,#9683,.T.);
#13803=EDGE_CURVE('',#10968,#10965,#6149,.T.);
#13804=EDGE_CURVE('',#10965,#10969,#6150,.T.);
#13805=EDGE_CURVE('',#10970,#10969,#9684,.T.);
#13806=EDGE_CURVE('',#10970,#10971,#6151,.T.);
#13807=EDGE_CURVE('',#10972,#10971,#6152,.T.);
#13808=EDGE_CURVE('',#10972,#10973,#9685,.T.);
#13809=EDGE_CURVE('',#10973,#10974,#6153,.T.);
#13810=EDGE_CURVE('',#10974,#10975,#9686,.T.);
#13811=EDGE_CURVE('',#10975,#10976,#6154,.T.);
#13812=EDGE_CURVE('',#10976,#10977,#9687,.T.);
#13813=EDGE_CURVE('',#10978,#10977,#6155,.T.);
#13814=EDGE_CURVE('',#10978,#10966,#6156,.T.);
#13815=EDGE_CURVE('',#10968,#10979,#6157,.T.);
#13816=EDGE_CURVE('',#10969,#10979,#6158,.T.);
#13817=EDGE_CURVE('',#10979,#10980,#9688,.T.);
#13818=EDGE_CURVE('',#10980,#10970,#6159,.T.);
#13819=EDGE_CURVE('',#10981,#10981,#9689,.T.);
#13820=EDGE_CURVE('',#10981,#10982,#6160,.T.);
#13821=EDGE_CURVE('',#10982,#10982,#9690,.T.);
#13822=EDGE_CURVE('',#10983,#10983,#9691,.T.);
#13823=EDGE_CURVE('',#10983,#10984,#6161,.T.);
#13824=EDGE_CURVE('',#10984,#10984,#9692,.T.);
#13825=EDGE_CURVE('',#10975,#10985,#6162,.T.);
#13826=EDGE_CURVE('',#10986,#10985,#6163,.T.);
#13827=EDGE_CURVE('',#10976,#10986,#6164,.T.);
#13828=EDGE_CURVE('',#10974,#10987,#6165,.T.);
#13829=EDGE_CURVE('',#10985,#10987,#9693,.T.);
#13830=EDGE_CURVE('',#10973,#10988,#6166,.T.);
#13831=EDGE_CURVE('',#10987,#10988,#6167,.T.);
#13832=EDGE_CURVE('',#10972,#10977,#9694,.T.);
#13833=EDGE_CURVE('',#10988,#10986,#9695,.T.);
#13834=EDGE_CURVE('',#10977,#10972,#6168,.T.);
#13835=EDGE_CURVE('',#10989,#10978,#9696,.T.);
#13836=EDGE_CURVE('',#10971,#10990,#9697,.T.);
#13837=EDGE_CURVE('',#10990,#10989,#6169,.T.);
#13838=EDGE_CURVE('',#10980,#10991,#6170,.T.);
#13839=EDGE_CURVE('',#10990,#10991,#6171,.T.);
#13840=EDGE_CURVE('',#10992,#10989,#6172,.T.);
#13841=EDGE_CURVE('',#10992,#10967,#6173,.T.);
#13842=EDGE_CURVE('',#10993,#10994,#6174,.T.);
#13843=EDGE_CURVE('',#10994,#10995,#6175,.T.);
#13844=EDGE_CURVE('',#10996,#10995,#6176,.T.);
#13845=EDGE_CURVE('',#10993,#10996,#6177,.T.);
#13846=EDGE_CURVE('',#10991,#10993,#6178,.T.);
#13847=EDGE_CURVE('',#10997,#10996,#6179,.T.);
#13848=EDGE_CURVE('',#10998,#10997,#6180,.T.);
#13849=EDGE_CURVE('',#10998,#10992,#6181,.T.);
#13850=EDGE_CURVE('',#10999,#10998,#6182,.T.);
#13851=EDGE_CURVE('',#11000,#10997,#6183,.T.);
#13852=EDGE_CURVE('',#10999,#11000,#6184,.T.);
#13853=EDGE_CURVE('',#10994,#10999,#6185,.T.);
#13854=EDGE_CURVE('',#10995,#11000,#6186,.T.);
#13855=EDGE_CURVE('',#11001,#11002,#6187,.T.);
#13856=EDGE_CURVE('',#11001,#11003,#6188,.T.);
#13857=EDGE_CURVE('',#11004,#11003,#6189,.T.);
#13858=EDGE_CURVE('',#11002,#11004,#6190,.T.);
#13859=EDGE_CURVE('',#11002,#11005,#6191,.T.);
#13860=EDGE_CURVE('',#11006,#11004,#6192,.T.);
#13861=EDGE_CURVE('',#11005,#11006,#6193,.T.);
#13862=EDGE_CURVE('',#11005,#11007,#6194,.T.);
#13863=EDGE_CURVE('',#11008,#11006,#6195,.T.);
#13864=EDGE_CURVE('',#11007,#11008,#6196,.T.);
#13865=EDGE_CURVE('',#11007,#11001,#6197,.T.);
#13866=EDGE_CURVE('',#11003,#11008,#6198,.T.);
#13867=EDGE_CURVE('',#11009,#11010,#6199,.T.);
#13868=EDGE_CURVE('',#11009,#11011,#6200,.T.);
#13869=EDGE_CURVE('',#11012,#11011,#6201,.T.);
#13870=EDGE_CURVE('',#11010,#11012,#6202,.T.);
#13871=EDGE_CURVE('',#11010,#11013,#6203,.T.);
#13872=EDGE_CURVE('',#11014,#11012,#6204,.T.);
#13873=EDGE_CURVE('',#11013,#11014,#6205,.T.);
#13874=EDGE_CURVE('',#11013,#11015,#6206,.T.);
#13875=EDGE_CURVE('',#11016,#11014,#6207,.T.);
#13876=EDGE_CURVE('',#11015,#11016,#6208,.T.);
#13877=EDGE_CURVE('',#11015,#11009,#6209,.T.);
#13878=EDGE_CURVE('',#11011,#11016,#6210,.T.);
#13879=EDGE_CURVE('',#11017,#11017,#9698,.T.);
#13880=EDGE_CURVE('',#11017,#11018,#6211,.T.);
#13881=EDGE_CURVE('',#11018,#11018,#9699,.T.);
#13882=EDGE_CURVE('',#11019,#11020,#6212,.T.);
#13883=EDGE_CURVE('',#11019,#11021,#6213,.T.);
#13884=EDGE_CURVE('',#11022,#11021,#6214,.T.);
#13885=EDGE_CURVE('',#11020,#11022,#6215,.T.);
#13886=EDGE_CURVE('',#11020,#11023,#6216,.T.);
#13887=EDGE_CURVE('',#11024,#11022,#6217,.T.);
#13888=EDGE_CURVE('',#11023,#11024,#6218,.T.);
#13889=EDGE_CURVE('',#11023,#11025,#6219,.T.);
#13890=EDGE_CURVE('',#11026,#11024,#6220,.T.);
#13891=EDGE_CURVE('',#11025,#11026,#6221,.T.);
#13892=EDGE_CURVE('',#11025,#11019,#6222,.T.);
#13893=EDGE_CURVE('',#11021,#11026,#6223,.T.);
#13894=EDGE_CURVE('',#11027,#11028,#6224,.T.);
#13895=EDGE_CURVE('',#11027,#11029,#6225,.T.);
#13896=EDGE_CURVE('',#11030,#11029,#6226,.T.);
#13897=EDGE_CURVE('',#11028,#11030,#6227,.T.);
#13898=EDGE_CURVE('',#11028,#11031,#6228,.T.);
#13899=EDGE_CURVE('',#11032,#11030,#6229,.T.);
#13900=EDGE_CURVE('',#11031,#11032,#6230,.T.);
#13901=EDGE_CURVE('',#11031,#11033,#6231,.T.);
#13902=EDGE_CURVE('',#11034,#11032,#6232,.T.);
#13903=EDGE_CURVE('',#11033,#11034,#6233,.T.);
#13904=EDGE_CURVE('',#11033,#11027,#6234,.T.);
#13905=EDGE_CURVE('',#11029,#11034,#6235,.T.);
#13906=EDGE_CURVE('',#11035,#11036,#6236,.T.);
#13907=EDGE_CURVE('',#11035,#11037,#6237,.T.);
#13908=EDGE_CURVE('',#11038,#11037,#6238,.T.);
#13909=EDGE_CURVE('',#11036,#11038,#6239,.T.);
#13910=EDGE_CURVE('',#11036,#11039,#6240,.T.);
#13911=EDGE_CURVE('',#11040,#11038,#6241,.T.);
#13912=EDGE_CURVE('',#11039,#11040,#6242,.T.);
#13913=EDGE_CURVE('',#11039,#11041,#6243,.T.);
#13914=EDGE_CURVE('',#11042,#11040,#6244,.T.);
#13915=EDGE_CURVE('',#11041,#11042,#6245,.T.);
#13916=EDGE_CURVE('',#11041,#11035,#6246,.T.);
#13917=EDGE_CURVE('',#11037,#11042,#6247,.T.);
#13918=EDGE_CURVE('',#11043,#11044,#6248,.T.);
#13919=EDGE_CURVE('',#11043,#11045,#6249,.T.);
#13920=EDGE_CURVE('',#11046,#11045,#6250,.T.);
#13921=EDGE_CURVE('',#11044,#11046,#6251,.T.);
#13922=EDGE_CURVE('',#11044,#11047,#6252,.T.);
#13923=EDGE_CURVE('',#11048,#11046,#6253,.T.);
#13924=EDGE_CURVE('',#11047,#11048,#6254,.T.);
#13925=EDGE_CURVE('',#11047,#11049,#6255,.T.);
#13926=EDGE_CURVE('',#11050,#11048,#6256,.T.);
#13927=EDGE_CURVE('',#11049,#11050,#6257,.T.);
#13928=EDGE_CURVE('',#11049,#11043,#6258,.T.);
#13929=EDGE_CURVE('',#11045,#11050,#6259,.T.);
#13930=EDGE_CURVE('',#11051,#11051,#9700,.T.);
#13931=EDGE_CURVE('',#11051,#11052,#6260,.T.);
#13932=EDGE_CURVE('',#11052,#11052,#9701,.T.);
#13933=EDGE_CURVE('',#11053,#11053,#9702,.T.);
#13934=EDGE_CURVE('',#11053,#11054,#6261,.T.);
#13935=EDGE_CURVE('',#11054,#11054,#9703,.T.);
#13936=EDGE_CURVE('',#11055,#11055,#9704,.T.);
#13937=EDGE_CURVE('',#11055,#11056,#6262,.T.);
#13938=EDGE_CURVE('',#11056,#11056,#9705,.T.);
#13939=EDGE_CURVE('',#11057,#11057,#9706,.T.);
#13940=EDGE_CURVE('',#11057,#11058,#6263,.T.);
#13941=EDGE_CURVE('',#11058,#11058,#9707,.T.);
#13942=EDGE_CURVE('',#11059,#11059,#9708,.T.);
#13943=EDGE_CURVE('',#11060,#11060,#9709,.T.);
#13944=EDGE_CURVE('',#11060,#11059,#6264,.T.);
#13945=EDGE_CURVE('',#11061,#11062,#6265,.T.);
#13946=EDGE_CURVE('',#11061,#11063,#505,.T.);
#13947=EDGE_CURVE('',#11063,#11064,#6266,.T.);
#13948=EDGE_CURVE('',#11064,#11064,#9710,.T.);
#13949=EDGE_CURVE('',#11063,#11065,#506,.T.);
#13950=EDGE_CURVE('',#11065,#11066,#9711,.T.);
#13951=EDGE_CURVE('',#11066,#11062,#507,.T.);
#13952=EDGE_CURVE('',#11067,#11068,#6267,.T.);
#13953=EDGE_CURVE('',#11067,#11061,#508,.T.);
#13954=EDGE_CURVE('',#11062,#11068,#509,.T.);
#13955=EDGE_CURVE('',#11069,#11070,#6268,.T.);
#13956=EDGE_CURVE('',#11069,#11067,#510,.T.);
#13957=EDGE_CURVE('',#11068,#11070,#511,.T.);
#13958=EDGE_CURVE('',#11071,#11072,#6269,.T.);
#13959=EDGE_CURVE('',#11071,#11073,#512,.T.);
#13960=EDGE_CURVE('',#11074,#11073,#9712,.T.);
#13961=EDGE_CURVE('',#11072,#11074,#513,.T.);
#13962=EDGE_CURVE('',#11075,#11076,#6270,.T.);
#13963=EDGE_CURVE('',#11075,#11071,#514,.T.);
#13964=EDGE_CURVE('',#11076,#11072,#515,.T.);
#13965=EDGE_CURVE('',#11077,#11078,#6271,.T.);
#13966=EDGE_CURVE('',#11077,#11075,#516,.T.);
#13967=EDGE_CURVE('',#11078,#11076,#517,.T.);
#13968=EDGE_CURVE('',#11079,#11080,#6272,.T.);
#13969=EDGE_CURVE('',#11079,#11077,#518,.T.);
#13970=EDGE_CURVE('',#11080,#11078,#519,.T.);
#13971=EDGE_CURVE('',#11073,#11081,#520,.T.);
#13972=EDGE_CURVE('',#11082,#11081,#9713,.F.);
#13973=EDGE_CURVE('',#11083,#11082,#9714,.F.);
#13974=EDGE_CURVE('',#11083,#11074,#521,.T.);
#13975=EDGE_CURVE('',#11070,#11083,#522,.T.);
#13976=EDGE_CURVE('',#11084,#11066,#523,.T.);
#13977=EDGE_CURVE('',#11084,#11080,#524,.T.);
#13978=EDGE_CURVE('',#11065,#11085,#525,.T.);
#13979=EDGE_CURVE('',#11085,#11084,#9715,.T.);
#13980=EDGE_CURVE('',#11085,#11079,#526,.T.);
#13981=EDGE_CURVE('',#11081,#11069,#527,.T.);
#13982=EDGE_CURVE('',#11081,#11083,#9716,.F.);
#13983=EDGE_CURVE('',#11086,#11087,#6273,.T.);
#13984=EDGE_CURVE('',#11087,#11087,#9717,.T.);
#13985=EDGE_CURVE('',#11088,#11089,#6274,.T.);
#13986=EDGE_CURVE('',#11088,#11090,#6275,.T.);
#13987=EDGE_CURVE('',#11090,#11091,#6276,.T.);
#13988=EDGE_CURVE('',#11089,#11091,#6277,.T.);
#13989=EDGE_CURVE('',#11092,#11088,#6278,.T.);
#13990=EDGE_CURVE('',#11092,#11093,#6279,.T.);
#13991=EDGE_CURVE('',#11093,#11090,#6280,.T.);
#13992=EDGE_CURVE('',#11094,#11092,#6281,.T.);
#13993=EDGE_CURVE('',#11094,#11095,#6282,.T.);
#13994=EDGE_CURVE('',#11095,#11093,#6283,.T.);
#13995=EDGE_CURVE('',#11096,#11094,#6284,.T.);
#13996=EDGE_CURVE('',#11096,#11097,#6285,.T.);
#13997=EDGE_CURVE('',#11097,#11095,#6286,.T.);
#13998=EDGE_CURVE('',#11098,#11096,#6287,.T.);
#13999=EDGE_CURVE('',#11098,#11099,#6288,.T.);
#14000=EDGE_CURVE('',#11099,#11097,#6289,.T.);
#14001=EDGE_CURVE('',#11089,#11098,#6290,.T.);
#14002=EDGE_CURVE('',#11091,#11099,#6291,.T.);
#14003=EDGE_CURVE('',#11100,#11100,#9718,.T.);
#14004=EDGE_CURVE('',#11064,#11100,#6292,.T.);
#14005=EDGE_CURVE('',#11101,#11101,#9719,.T.);
#14006=EDGE_CURVE('',#11101,#11082,#6293,.T.);
#14007=EDGE_CURVE('',#11102,#11103,#6294,.T.);
#14008=EDGE_CURVE('',#11102,#11104,#528,.T.);
#14009=EDGE_CURVE('',#11104,#11105,#9720,.T.);
#14010=EDGE_CURVE('',#11105,#11106,#6295,.T.);
#14011=EDGE_CURVE('',#11106,#11106,#9721,.T.);
#14012=EDGE_CURVE('',#11105,#11107,#9722,.T.);
#14013=EDGE_CURVE('',#11107,#11103,#529,.T.);
#14014=EDGE_CURVE('',#11108,#11109,#6296,.T.);
#14015=EDGE_CURVE('',#11108,#11102,#530,.T.);
#14016=EDGE_CURVE('',#11103,#11109,#531,.T.);
#14017=EDGE_CURVE('',#11110,#11111,#6297,.T.);
#14018=EDGE_CURVE('',#11110,#11108,#532,.T.);
#14019=EDGE_CURVE('',#11109,#11111,#533,.T.);
#14020=EDGE_CURVE('',#11112,#11113,#6298,.T.);
#14021=EDGE_CURVE('',#11112,#11110,#534,.T.);
#14022=EDGE_CURVE('',#11111,#11113,#535,.T.);
#14023=EDGE_CURVE('',#11114,#11115,#6299,.T.);
#14024=EDGE_CURVE('',#11114,#11112,#536,.T.);
#14025=EDGE_CURVE('',#11113,#11115,#537,.T.);
#14026=EDGE_CURVE('',#11116,#11117,#6300,.T.);
#14027=EDGE_CURVE('',#11116,#11114,#538,.T.);
#14028=EDGE_CURVE('',#11115,#11117,#539,.T.);
#14029=EDGE_CURVE('',#11118,#11119,#6301,.T.);
#14030=EDGE_CURVE('',#11118,#11116,#540,.T.);
#14031=EDGE_CURVE('',#11117,#11119,#541,.T.);
#14032=EDGE_CURVE('',#11120,#11121,#6302,.T.);
#14033=EDGE_CURVE('',#11120,#11118,#542,.T.);
#14034=EDGE_CURVE('',#11119,#11121,#543,.T.);
#14035=EDGE_CURVE('',#11122,#11123,#6303,.T.);
#14036=EDGE_CURVE('',#11122,#11124,#544,.T.);
#14037=EDGE_CURVE('',#11125,#11124,#9723,.T.);
#14038=EDGE_CURVE('',#11123,#11125,#545,.T.);
#14039=EDGE_CURVE('',#11126,#11127,#6304,.T.);
#14040=EDGE_CURVE('',#11126,#11122,#546,.T.);
#14041=EDGE_CURVE('',#11127,#11123,#547,.T.);
#14042=EDGE_CURVE('',#11128,#11129,#6305,.T.);
#14043=EDGE_CURVE('',#11128,#11126,#548,.T.);
#14044=EDGE_CURVE('',#11129,#11127,#549,.T.);
#14045=EDGE_CURVE('',#11130,#11131,#6306,.T.);
#14046=EDGE_CURVE('',#11130,#11128,#550,.T.);
#14047=EDGE_CURVE('',#11131,#11129,#551,.T.);
#14048=EDGE_CURVE('',#11132,#11133,#6307,.T.);
#14049=EDGE_CURVE('',#11132,#11130,#552,.T.);
#14050=EDGE_CURVE('',#11133,#11131,#553,.T.);
#14051=EDGE_CURVE('',#11134,#11135,#6308,.T.);
#14052=EDGE_CURVE('',#11134,#11132,#554,.T.);
#14053=EDGE_CURVE('',#11135,#11133,#555,.T.);
#14054=EDGE_CURVE('',#11136,#11137,#6309,.T.);
#14055=EDGE_CURVE('',#11136,#11134,#556,.T.);
#14056=EDGE_CURVE('',#11137,#11135,#557,.T.);
#14057=EDGE_CURVE('',#11138,#11139,#6310,.T.);
#14058=EDGE_CURVE('',#11138,#11136,#558,.T.);
#14059=EDGE_CURVE('',#11139,#11137,#559,.T.);
#14060=EDGE_CURVE('',#11140,#11125,#560,.T.);
#14061=EDGE_CURVE('',#11121,#11140,#561,.T.);
#14062=EDGE_CURVE('',#11141,#11107,#562,.T.);
#14063=EDGE_CURVE('',#11141,#11139,#563,.T.);
#14064=EDGE_CURVE('',#11104,#11142,#564,.T.);
#14065=EDGE_CURVE('',#11142,#11141,#9724,.T.);
#14066=EDGE_CURVE('',#11142,#11138,#565,.T.);
#14067=EDGE_CURVE('',#11124,#11143,#566,.T.);
#14068=EDGE_CURVE('',#11143,#11120,#567,.T.);
#14069=EDGE_CURVE('',#11143,#11140,#9725,.F.);
#14070=EDGE_CURVE('',#11144,#11145,#6311,.T.);
#14071=EDGE_CURVE('',#11145,#11145,#9726,.T.);
#14072=EDGE_CURVE('',#11145,#11146,#6312,.T.);
#14073=EDGE_CURVE('',#11146,#11146,#9727,.T.);
#14074=EDGE_CURVE('',#11146,#11147,#6313,.T.);
#14075=EDGE_CURVE('',#11147,#11147,#9728,.T.);
#14076=EDGE_CURVE('',#11148,#11149,#227,.T.);
#14077=EDGE_CURVE('',#11150,#11148,#228,.T.);
#14078=EDGE_CURVE('',#11149,#11150,#9729,.T.);
#14079=EDGE_CURVE('',#11151,#11152,#229,.T.);
#14080=EDGE_CURVE('',#11153,#11151,#230,.T.);
#14081=EDGE_CURVE('',#11152,#11153,#9730,.T.);
#14082=EDGE_CURVE('',#11154,#11155,#231,.T.);
#14083=EDGE_CURVE('',#11156,#11154,#232,.T.);
#14084=EDGE_CURVE('',#11155,#11156,#9731,.T.);
#14085=EDGE_CURVE('',#11157,#11158,#233,.T.);
#14086=EDGE_CURVE('',#11159,#11157,#234,.T.);
#14087=EDGE_CURVE('',#11158,#11159,#9732,.T.);
#14088=EDGE_CURVE('',#11160,#11161,#235,.T.);
#14089=EDGE_CURVE('',#11162,#11160,#236,.T.);
#14090=EDGE_CURVE('',#11161,#11162,#9733,.T.);
#14091=EDGE_CURVE('',#11163,#11164,#237,.T.);
#14092=EDGE_CURVE('',#11165,#11163,#9734,.T.);
#14093=EDGE_CURVE('',#11164,#11165,#238,.T.);
#14094=EDGE_CURVE('',#11160,#11166,#6314,.T.);
#14095=EDGE_CURVE('',#11166,#11167,#239,.T.);
#14096=EDGE_CURVE('',#11168,#11167,#6315,.T.);
#14097=EDGE_CURVE('',#11168,#11169,#240,.T.);
#14098=EDGE_CURVE('',#11157,#11169,#6316,.T.);
#14099=EDGE_CURVE('',#11158,#11162,#6317,.T.);
#14100=EDGE_CURVE('',#11169,#11170,#241,.T.);
#14101=EDGE_CURVE('',#11171,#11170,#6318,.T.);
#14102=EDGE_CURVE('',#11171,#11172,#242,.T.);
#14103=EDGE_CURVE('',#11154,#11172,#6319,.T.);
#14104=EDGE_CURVE('',#11155,#11159,#6320,.T.);
#14105=EDGE_CURVE('',#11172,#11173,#243,.T.);
#14106=EDGE_CURVE('',#11174,#11173,#6321,.T.);
#14107=EDGE_CURVE('',#11174,#11175,#244,.T.);
#14108=EDGE_CURVE('',#11151,#11175,#6322,.T.);
#14109=EDGE_CURVE('',#11152,#11156,#6323,.T.);
#14110=EDGE_CURVE('',#11161,#11163,#6324,.T.);
#14111=EDGE_CURVE('',#11149,#11153,#6325,.T.);
#14112=EDGE_CURVE('',#11165,#11150,#6326,.T.);
#14113=EDGE_CURVE('',#11175,#11176,#245,.T.);
#14114=EDGE_CURVE('',#11177,#11176,#6327,.T.);
#14115=EDGE_CURVE('',#11177,#11178,#246,.T.);
#14116=EDGE_CURVE('',#11148,#11178,#6328,.T.);
#14117=EDGE_CURVE('',#11179,#11180,#247,.T.);
#14118=EDGE_CURVE('',#11181,#11179,#9735,.T.);
#14119=EDGE_CURVE('',#11180,#11181,#248,.T.);
#14120=EDGE_CURVE('',#11182,#11177,#9736,.T.);
#14121=EDGE_CURVE('',#11178,#11182,#249,.T.);
#14122=EDGE_CURVE('',#11176,#11174,#9737,.T.);
#14123=EDGE_CURVE('',#11173,#11171,#9738,.T.);
#14124=EDGE_CURVE('',#11170,#11168,#9739,.T.);
#14125=EDGE_CURVE('',#11183,#11166,#250,.T.);
#14126=EDGE_CURVE('',#11167,#11183,#9740,.T.);
#14127=EDGE_CURVE('',#11164,#11180,#6329,.T.);
#14128=EDGE_CURVE('',#11183,#11181,#6330,.T.);
#14129=EDGE_CURVE('',#11184,#11184,#9741,.T.);
#14130=EDGE_CURVE('',#11106,#11184,#6331,.T.);
#14131=EDGE_CURVE('',#11179,#11182,#6332,.T.);
#14132=EDGE_CURVE('',#11185,#11186,#6333,.T.);
#14133=EDGE_CURVE('',#11185,#11187,#568,.T.);
#14134=EDGE_CURVE('',#11187,#11188,#9742,.T.);
#14135=EDGE_CURVE('',#11188,#11189,#6334,.T.);
#14136=EDGE_CURVE('',#11189,#11189,#9743,.T.);
#14137=EDGE_CURVE('',#11188,#11190,#9744,.T.);
#14138=EDGE_CURVE('',#11190,#11186,#569,.T.);
#14139=EDGE_CURVE('',#11191,#11192,#6335,.T.);
#14140=EDGE_CURVE('',#11191,#11185,#570,.T.);
#14141=EDGE_CURVE('',#11186,#11192,#571,.T.);
#14142=EDGE_CURVE('',#11193,#11194,#6336,.T.);
#14143=EDGE_CURVE('',#11193,#11191,#572,.T.);
#14144=EDGE_CURVE('',#11192,#11194,#573,.T.);
#14145=EDGE_CURVE('',#11195,#11196,#6337,.T.);
#14146=EDGE_CURVE('',#11195,#11193,#574,.T.);
#14147=EDGE_CURVE('',#11194,#11196,#575,.T.);
#14148=EDGE_CURVE('',#11197,#11198,#6338,.T.);
#14149=EDGE_CURVE('',#11197,#11195,#576,.T.);
#14150=EDGE_CURVE('',#11196,#11198,#577,.T.);
#14151=EDGE_CURVE('',#11199,#11200,#6339,.T.);
#14152=EDGE_CURVE('',#11199,#11197,#578,.T.);
#14153=EDGE_CURVE('',#11198,#11200,#579,.T.);
#14154=EDGE_CURVE('',#11201,#11202,#6340,.T.);
#14155=EDGE_CURVE('',#11201,#11199,#580,.T.);
#14156=EDGE_CURVE('',#11200,#11202,#581,.T.);
#14157=EDGE_CURVE('',#11203,#11204,#6341,.T.);
#14158=EDGE_CURVE('',#11203,#11201,#582,.T.);
#14159=EDGE_CURVE('',#11202,#11204,#583,.T.);
#14160=EDGE_CURVE('',#11205,#11206,#6342,.T.);
#14161=EDGE_CURVE('',#11205,#11203,#584,.T.);
#14162=EDGE_CURVE('',#11204,#11206,#585,.T.);
#14163=EDGE_CURVE('',#11207,#11208,#6343,.T.);
#14164=EDGE_CURVE('',#11207,#11205,#586,.T.);
#14165=EDGE_CURVE('',#11206,#11208,#587,.T.);
#14166=EDGE_CURVE('',#11209,#11210,#6344,.T.);
#14167=EDGE_CURVE('',#11209,#11207,#588,.T.);
#14168=EDGE_CURVE('',#11208,#11210,#589,.T.);
#14169=EDGE_CURVE('',#11211,#11212,#6345,.T.);
#14170=EDGE_CURVE('',#11211,#11209,#590,.T.);
#14171=EDGE_CURVE('',#11210,#11212,#591,.T.);
#14172=EDGE_CURVE('',#11213,#11214,#6346,.T.);
#14173=EDGE_CURVE('',#11213,#11211,#592,.T.);
#14174=EDGE_CURVE('',#11212,#11214,#593,.T.);
#14175=EDGE_CURVE('',#11215,#11216,#6347,.T.);
#14176=EDGE_CURVE('',#11215,#11213,#594,.T.);
#14177=EDGE_CURVE('',#11214,#11216,#595,.T.);
#14178=EDGE_CURVE('',#11217,#11218,#6348,.T.);
#14179=EDGE_CURVE('',#11217,#11215,#596,.T.);
#14180=EDGE_CURVE('',#11216,#11218,#597,.T.);
#14181=EDGE_CURVE('',#11219,#11220,#6349,.T.);
#14182=EDGE_CURVE('',#11219,#11217,#598,.T.);
#14183=EDGE_CURVE('',#11218,#11220,#599,.T.);
#14184=EDGE_CURVE('',#11221,#11222,#6350,.T.);
#14185=EDGE_CURVE('',#11221,#11219,#600,.T.);
#14186=EDGE_CURVE('',#11220,#11222,#601,.T.);
#14187=EDGE_CURVE('',#11223,#11224,#6351,.T.);
#14188=EDGE_CURVE('',#11223,#11221,#602,.T.);
#14189=EDGE_CURVE('',#11222,#11224,#603,.T.);
#14190=EDGE_CURVE('',#11225,#11226,#6352,.T.);
#14191=EDGE_CURVE('',#11225,#11223,#604,.T.);
#14192=EDGE_CURVE('',#11224,#11226,#605,.T.);
#14193=EDGE_CURVE('',#11227,#11228,#6353,.T.);
#14194=EDGE_CURVE('',#11227,#11225,#606,.T.);
#14195=EDGE_CURVE('',#11226,#11228,#607,.T.);
#14196=EDGE_CURVE('',#11229,#11230,#6354,.T.);
#14197=EDGE_CURVE('',#11229,#11227,#608,.T.);
#14198=EDGE_CURVE('',#11228,#11230,#609,.T.);
#14199=EDGE_CURVE('',#11231,#11232,#6355,.T.);
#14200=EDGE_CURVE('',#11231,#11229,#610,.T.);
#14201=EDGE_CURVE('',#11230,#11232,#611,.T.);
#14202=EDGE_CURVE('',#11233,#11234,#6356,.T.);
#14203=EDGE_CURVE('',#11233,#11231,#612,.T.);
#14204=EDGE_CURVE('',#11232,#11234,#613,.T.);
#14205=EDGE_CURVE('',#11235,#11236,#6357,.T.);
#14206=EDGE_CURVE('',#11235,#11233,#614,.T.);
#14207=EDGE_CURVE('',#11234,#11236,#615,.T.);
#14208=EDGE_CURVE('',#11237,#11238,#6358,.T.);
#14209=EDGE_CURVE('',#11237,#11235,#616,.T.);
#14210=EDGE_CURVE('',#11236,#11238,#617,.T.);
#14211=EDGE_CURVE('',#11239,#11240,#6359,.T.);
#14212=EDGE_CURVE('',#11239,#11237,#618,.T.);
#14213=EDGE_CURVE('',#11238,#11240,#619,.T.);
#14214=EDGE_CURVE('',#11241,#11242,#6360,.T.);
#14215=EDGE_CURVE('',#11241,#11239,#620,.T.);
#14216=EDGE_CURVE('',#11240,#11242,#621,.T.);
#14217=EDGE_CURVE('',#11243,#11244,#6361,.T.);
#14218=EDGE_CURVE('',#11243,#11241,#622,.T.);
#14219=EDGE_CURVE('',#11242,#11244,#623,.T.);
#14220=EDGE_CURVE('',#11245,#11246,#6362,.T.);
#14221=EDGE_CURVE('',#11245,#11247,#624,.T.);
#14222=EDGE_CURVE('',#11248,#11247,#9745,.T.);
#14223=EDGE_CURVE('',#11246,#11248,#625,.T.);
#14224=EDGE_CURVE('',#11249,#11250,#6363,.T.);
#14225=EDGE_CURVE('',#11249,#11245,#626,.T.);
#14226=EDGE_CURVE('',#11250,#11246,#627,.T.);
#14227=EDGE_CURVE('',#11251,#11252,#6364,.T.);
#14228=EDGE_CURVE('',#11251,#11249,#628,.T.);
#14229=EDGE_CURVE('',#11252,#11250,#629,.T.);
#14230=EDGE_CURVE('',#11253,#11254,#6365,.T.);
#14231=EDGE_CURVE('',#11253,#11251,#630,.T.);
#14232=EDGE_CURVE('',#11254,#11252,#631,.T.);
#14233=EDGE_CURVE('',#11255,#11256,#6366,.T.);
#14234=EDGE_CURVE('',#11255,#11253,#632,.T.);
#14235=EDGE_CURVE('',#11256,#11254,#633,.T.);
#14236=EDGE_CURVE('',#11257,#11258,#6367,.T.);
#14237=EDGE_CURVE('',#11257,#11255,#634,.T.);
#14238=EDGE_CURVE('',#11258,#11256,#635,.T.);
#14239=EDGE_CURVE('',#11259,#11260,#6368,.T.);
#14240=EDGE_CURVE('',#11259,#11257,#636,.T.);
#14241=EDGE_CURVE('',#11260,#11258,#637,.T.);
#14242=EDGE_CURVE('',#11261,#11262,#6369,.T.);
#14243=EDGE_CURVE('',#11261,#11259,#638,.T.);
#14244=EDGE_CURVE('',#11262,#11260,#639,.T.);
#14245=EDGE_CURVE('',#11263,#11264,#6370,.T.);
#14246=EDGE_CURVE('',#11263,#11261,#640,.T.);
#14247=EDGE_CURVE('',#11264,#11262,#641,.T.);
#14248=EDGE_CURVE('',#11265,#11266,#6371,.T.);
#14249=EDGE_CURVE('',#11265,#11263,#642,.T.);
#14250=EDGE_CURVE('',#11266,#11264,#643,.T.);
#14251=EDGE_CURVE('',#11267,#11268,#6372,.T.);
#14252=EDGE_CURVE('',#11267,#11265,#644,.T.);
#14253=EDGE_CURVE('',#11268,#11266,#645,.T.);
#14254=EDGE_CURVE('',#11269,#11270,#6373,.T.);
#14255=EDGE_CURVE('',#11269,#11267,#646,.T.);
#14256=EDGE_CURVE('',#11270,#11268,#647,.T.);
#14257=EDGE_CURVE('',#11271,#11272,#6374,.T.);
#14258=EDGE_CURVE('',#11271,#11269,#648,.T.);
#14259=EDGE_CURVE('',#11272,#11270,#649,.T.);
#14260=EDGE_CURVE('',#11273,#11274,#6375,.T.);
#14261=EDGE_CURVE('',#11273,#11271,#650,.T.);
#14262=EDGE_CURVE('',#11274,#11272,#651,.T.);
#14263=EDGE_CURVE('',#11275,#11276,#6376,.T.);
#14264=EDGE_CURVE('',#11275,#11273,#652,.T.);
#14265=EDGE_CURVE('',#11276,#11274,#653,.T.);
#14266=EDGE_CURVE('',#11277,#11278,#6377,.T.);
#14267=EDGE_CURVE('',#11277,#11275,#654,.T.);
#14268=EDGE_CURVE('',#11278,#11276,#655,.T.);
#14269=EDGE_CURVE('',#11279,#11280,#6378,.T.);
#14270=EDGE_CURVE('',#11279,#11277,#656,.T.);
#14271=EDGE_CURVE('',#11280,#11278,#657,.T.);
#14272=EDGE_CURVE('',#11281,#11282,#6379,.T.);
#14273=EDGE_CURVE('',#11281,#11279,#658,.T.);
#14274=EDGE_CURVE('',#11282,#11280,#659,.T.);
#14275=EDGE_CURVE('',#11283,#11284,#6380,.T.);
#14276=EDGE_CURVE('',#11283,#11281,#660,.T.);
#14277=EDGE_CURVE('',#11284,#11282,#661,.T.);
#14278=EDGE_CURVE('',#11285,#11286,#6381,.T.);
#14279=EDGE_CURVE('',#11285,#11283,#662,.T.);
#14280=EDGE_CURVE('',#11286,#11284,#663,.T.);
#14281=EDGE_CURVE('',#11287,#11288,#6382,.T.);
#14282=EDGE_CURVE('',#11287,#11285,#664,.T.);
#14283=EDGE_CURVE('',#11288,#11286,#665,.T.);
#14284=EDGE_CURVE('',#11289,#11290,#6383,.T.);
#14285=EDGE_CURVE('',#11289,#11287,#666,.T.);
#14286=EDGE_CURVE('',#11290,#11288,#667,.T.);
#14287=EDGE_CURVE('',#11291,#11292,#6384,.T.);
#14288=EDGE_CURVE('',#11291,#11289,#668,.T.);
#14289=EDGE_CURVE('',#11292,#11290,#669,.T.);
#14290=EDGE_CURVE('',#11293,#11294,#6385,.T.);
#14291=EDGE_CURVE('',#11293,#11291,#670,.T.);
#14292=EDGE_CURVE('',#11294,#11292,#671,.T.);
#14293=EDGE_CURVE('',#11295,#11296,#6386,.T.);
#14294=EDGE_CURVE('',#11295,#11293,#672,.T.);
#14295=EDGE_CURVE('',#11296,#11294,#673,.T.);
#14296=EDGE_CURVE('',#11297,#11298,#6387,.T.);
#14297=EDGE_CURVE('',#11297,#11295,#674,.T.);
#14298=EDGE_CURVE('',#11298,#11296,#675,.T.);
#14299=EDGE_CURVE('',#11299,#11300,#6388,.T.);
#14300=EDGE_CURVE('',#11299,#11297,#676,.T.);
#14301=EDGE_CURVE('',#11300,#11298,#677,.T.);
#14302=EDGE_CURVE('',#11301,#11302,#6389,.T.);
#14303=EDGE_CURVE('',#11301,#11299,#678,.T.);
#14304=EDGE_CURVE('',#11302,#11300,#679,.T.);
#14305=EDGE_CURVE('',#11303,#11304,#6390,.T.);
#14306=EDGE_CURVE('',#11305,#11303,#9746,.T.);
#14307=EDGE_CURVE('',#11305,#11301,#680,.T.);
#14308=EDGE_CURVE('',#11304,#11302,#681,.T.);
#14309=EDGE_CURVE('',#11247,#11306,#682,.T.);
#14310=EDGE_CURVE('',#11307,#11306,#9747,.T.);
#14311=EDGE_CURVE('',#11308,#11307,#9748,.T.);
#14312=EDGE_CURVE('',#11308,#11248,#683,.T.);
#14313=EDGE_CURVE('',#11244,#11308,#684,.T.);
#14314=EDGE_CURVE('',#11309,#11190,#685,.T.);
#14315=EDGE_CURVE('',#11309,#11304,#686,.T.);
#14316=EDGE_CURVE('',#11187,#11305,#687,.T.);
#14317=EDGE_CURVE('',#11303,#11309,#9749,.T.);
#14318=EDGE_CURVE('',#11306,#11243,#688,.T.);
#14319=EDGE_CURVE('',#11310,#11311,#9750,.T.);
#14320=EDGE_CURVE('',#11310,#11312,#6391,.T.);
#14321=EDGE_CURVE('',#11312,#11311,#6392,.T.);
#14322=EDGE_CURVE('',#11311,#11313,#6393,.T.);
#14323=EDGE_CURVE('',#11312,#11314,#6394,.T.);
#14324=EDGE_CURVE('',#11313,#11314,#251,.T.);
#14325=EDGE_CURVE('',#11315,#11310,#6395,.T.);
#14326=EDGE_CURVE('',#11314,#11315,#252,.T.);
#14327=EDGE_CURVE('',#11316,#11317,#9751,.T.);
#14328=EDGE_CURVE('',#11316,#11318,#6396,.T.);
#14329=EDGE_CURVE('',#11318,#11317,#6397,.T.);
#14330=EDGE_CURVE('',#11317,#11319,#6398,.T.);
#14331=EDGE_CURVE('',#11318,#11320,#6399,.T.);
#14332=EDGE_CURVE('',#11319,#11320,#253,.T.);
#14333=EDGE_CURVE('',#11321,#11316,#6400,.T.);
#14334=EDGE_CURVE('',#11320,#11321,#254,.T.);
#14335=EDGE_CURVE('',#11322,#11323,#9752,.T.);
#14336=EDGE_CURVE('',#11322,#11324,#6401,.T.);
#14337=EDGE_CURVE('',#11324,#11323,#6402,.T.);
#14338=EDGE_CURVE('',#11323,#11325,#6403,.T.);
#14339=EDGE_CURVE('',#11324,#11326,#6404,.T.);
#14340=EDGE_CURVE('',#11325,#11326,#255,.T.);
#14341=EDGE_CURVE('',#11327,#11322,#6405,.T.);
#14342=EDGE_CURVE('',#11326,#11327,#256,.T.);
#14343=EDGE_CURVE('',#11328,#11329,#9753,.T.);
#14344=EDGE_CURVE('',#11328,#11330,#6406,.T.);
#14345=EDGE_CURVE('',#11330,#11329,#6407,.T.);
#14346=EDGE_CURVE('',#11329,#11331,#6408,.T.);
#14347=EDGE_CURVE('',#11330,#11332,#6409,.T.);
#14348=EDGE_CURVE('',#11331,#11332,#257,.T.);
#14349=EDGE_CURVE('',#11333,#11328,#6410,.T.);
#14350=EDGE_CURVE('',#11332,#11333,#258,.T.);
#14351=EDGE_CURVE('',#11334,#11335,#9754,.T.);
#14352=EDGE_CURVE('',#11334,#11336,#6411,.T.);
#14353=EDGE_CURVE('',#11336,#11335,#6412,.T.);
#14354=EDGE_CURVE('',#11335,#11337,#6413,.T.);
#14355=EDGE_CURVE('',#11336,#11338,#6414,.T.);
#14356=EDGE_CURVE('',#11337,#11338,#259,.T.);
#14357=EDGE_CURVE('',#11339,#11334,#6415,.T.);
#14358=EDGE_CURVE('',#11338,#11339,#260,.T.);
#14359=EDGE_CURVE('',#11340,#11341,#9755,.T.);
#14360=EDGE_CURVE('',#11340,#11342,#6416,.T.);
#14361=EDGE_CURVE('',#11342,#11341,#6417,.T.);
#14362=EDGE_CURVE('',#11341,#11343,#6418,.T.);
#14363=EDGE_CURVE('',#11342,#11344,#6419,.T.);
#14364=EDGE_CURVE('',#11343,#11344,#261,.T.);
#14365=EDGE_CURVE('',#11345,#11340,#6420,.T.);
#14366=EDGE_CURVE('',#11344,#11345,#262,.T.);
#14367=EDGE_CURVE('',#11346,#11347,#9756,.T.);
#14368=EDGE_CURVE('',#11346,#11348,#6421,.T.);
#14369=EDGE_CURVE('',#11348,#11347,#6422,.T.);
#14370=EDGE_CURVE('',#11347,#11349,#6423,.T.);
#14371=EDGE_CURVE('',#11348,#11350,#6424,.T.);
#14372=EDGE_CURVE('',#11349,#11350,#263,.T.);
#14373=EDGE_CURVE('',#11351,#11346,#6425,.T.);
#14374=EDGE_CURVE('',#11350,#11351,#264,.T.);
#14375=EDGE_CURVE('',#11352,#11353,#9757,.T.);
#14376=EDGE_CURVE('',#11352,#11354,#6426,.T.);
#14377=EDGE_CURVE('',#11354,#11353,#6427,.T.);
#14378=EDGE_CURVE('',#11353,#11355,#6428,.T.);
#14379=EDGE_CURVE('',#11354,#11356,#6429,.T.);
#14380=EDGE_CURVE('',#11355,#11356,#265,.T.);
#14381=EDGE_CURVE('',#11357,#11352,#6430,.T.);
#14382=EDGE_CURVE('',#11356,#11357,#266,.T.);
#14383=EDGE_CURVE('',#11358,#11359,#9758,.T.);
#14384=EDGE_CURVE('',#11358,#11360,#6431,.T.);
#14385=EDGE_CURVE('',#11360,#11359,#6432,.T.);
#14386=EDGE_CURVE('',#11359,#11361,#6433,.T.);
#14387=EDGE_CURVE('',#11360,#11362,#6434,.T.);
#14388=EDGE_CURVE('',#11361,#11362,#267,.T.);
#14389=EDGE_CURVE('',#11363,#11358,#6435,.T.);
#14390=EDGE_CURVE('',#11362,#11363,#268,.T.);
#14391=EDGE_CURVE('',#11364,#11365,#9759,.T.);
#14392=EDGE_CURVE('',#11364,#11366,#6436,.T.);
#14393=EDGE_CURVE('',#11366,#11365,#6437,.T.);
#14394=EDGE_CURVE('',#11365,#11367,#6438,.T.);
#14395=EDGE_CURVE('',#11366,#11368,#6439,.T.);
#14396=EDGE_CURVE('',#11367,#11368,#269,.T.);
#14397=EDGE_CURVE('',#11369,#11364,#6440,.T.);
#14398=EDGE_CURVE('',#11368,#11369,#270,.T.);
#14399=EDGE_CURVE('',#11370,#11371,#9760,.T.);
#14400=EDGE_CURVE('',#11370,#11372,#6441,.T.);
#14401=EDGE_CURVE('',#11372,#11371,#6442,.T.);
#14402=EDGE_CURVE('',#11371,#11373,#6443,.T.);
#14403=EDGE_CURVE('',#11372,#11374,#6444,.T.);
#14404=EDGE_CURVE('',#11373,#11374,#271,.T.);
#14405=EDGE_CURVE('',#11375,#11370,#6445,.T.);
#14406=EDGE_CURVE('',#11374,#11375,#272,.T.);
#14407=EDGE_CURVE('',#11376,#11377,#9761,.T.);
#14408=EDGE_CURVE('',#11376,#11378,#6446,.T.);
#14409=EDGE_CURVE('',#11378,#11377,#6447,.T.);
#14410=EDGE_CURVE('',#11377,#11379,#6448,.T.);
#14411=EDGE_CURVE('',#11378,#11380,#6449,.T.);
#14412=EDGE_CURVE('',#11379,#11380,#273,.T.);
#14413=EDGE_CURVE('',#11381,#11376,#6450,.T.);
#14414=EDGE_CURVE('',#11380,#11381,#274,.T.);
#14415=EDGE_CURVE('',#11382,#11383,#9762,.T.);
#14416=EDGE_CURVE('',#11382,#11384,#6451,.T.);
#14417=EDGE_CURVE('',#11384,#11383,#6452,.T.);
#14418=EDGE_CURVE('',#11383,#11385,#6453,.T.);
#14419=EDGE_CURVE('',#11384,#11386,#6454,.T.);
#14420=EDGE_CURVE('',#11385,#11386,#275,.T.);
#14421=EDGE_CURVE('',#11387,#11382,#6455,.T.);
#14422=EDGE_CURVE('',#11386,#11387,#276,.T.);
#14423=EDGE_CURVE('',#11388,#11389,#9763,.T.);
#14424=EDGE_CURVE('',#11388,#11390,#6456,.T.);
#14425=EDGE_CURVE('',#11390,#11389,#6457,.T.);
#14426=EDGE_CURVE('',#11389,#11391,#6458,.T.);
#14427=EDGE_CURVE('',#11390,#11392,#6459,.T.);
#14428=EDGE_CURVE('',#11391,#11392,#277,.T.);
#14429=EDGE_CURVE('',#11393,#11388,#6460,.T.);
#14430=EDGE_CURVE('',#11392,#11393,#278,.T.);
#14431=EDGE_CURVE('',#11394,#11395,#9764,.T.);
#14432=EDGE_CURVE('',#11394,#11396,#6461,.T.);
#14433=EDGE_CURVE('',#11396,#11395,#6462,.T.);
#14434=EDGE_CURVE('',#11395,#11397,#6463,.T.);
#14435=EDGE_CURVE('',#11396,#11398,#6464,.T.);
#14436=EDGE_CURVE('',#11397,#11398,#279,.T.);
#14437=EDGE_CURVE('',#11399,#11394,#6465,.T.);
#14438=EDGE_CURVE('',#11398,#11399,#280,.T.);
#14439=EDGE_CURVE('',#11400,#11401,#9765,.T.);
#14440=EDGE_CURVE('',#11400,#11402,#6466,.T.);
#14441=EDGE_CURVE('',#11402,#11401,#6467,.T.);
#14442=EDGE_CURVE('',#11401,#11403,#6468,.T.);
#14443=EDGE_CURVE('',#11402,#11404,#6469,.T.);
#14444=EDGE_CURVE('',#11403,#11404,#281,.T.);
#14445=EDGE_CURVE('',#11405,#11400,#6470,.T.);
#14446=EDGE_CURVE('',#11404,#11405,#282,.T.);
#14447=EDGE_CURVE('',#11406,#11407,#9766,.T.);
#14448=EDGE_CURVE('',#11406,#11408,#6471,.T.);
#14449=EDGE_CURVE('',#11408,#11407,#6472,.T.);
#14450=EDGE_CURVE('',#11407,#11409,#6473,.T.);
#14451=EDGE_CURVE('',#11408,#11410,#6474,.T.);
#14452=EDGE_CURVE('',#11409,#11410,#283,.T.);
#14453=EDGE_CURVE('',#11411,#11406,#6475,.T.);
#14454=EDGE_CURVE('',#11410,#11411,#284,.T.);
#14455=EDGE_CURVE('',#11412,#11413,#9767,.T.);
#14456=EDGE_CURVE('',#11412,#11414,#6476,.T.);
#14457=EDGE_CURVE('',#11414,#11415,#6477,.T.);
#14458=EDGE_CURVE('',#11413,#11415,#9768,.T.);
#14459=EDGE_CURVE('',#11415,#11416,#6478,.T.);
#14460=EDGE_CURVE('',#11414,#11417,#6479,.T.);
#14461=EDGE_CURVE('',#11416,#11417,#285,.T.);
#14462=EDGE_CURVE('',#11418,#11412,#6480,.T.);
#14463=EDGE_CURVE('',#11417,#11418,#286,.T.);
#14464=EDGE_CURVE('',#11419,#11420,#9769,.T.);
#14465=EDGE_CURVE('',#11419,#11421,#6481,.T.);
#14466=EDGE_CURVE('',#11421,#11420,#6482,.T.);
#14467=EDGE_CURVE('',#11420,#11422,#6483,.T.);
#14468=EDGE_CURVE('',#11421,#11423,#6484,.T.);
#14469=EDGE_CURVE('',#11422,#11423,#287,.T.);
#14470=EDGE_CURVE('',#11424,#11419,#6485,.T.);
#14471=EDGE_CURVE('',#11423,#11424,#288,.T.);
#14472=EDGE_CURVE('',#11425,#11426,#9770,.T.);
#14473=EDGE_CURVE('',#11425,#11427,#6486,.T.);
#14474=EDGE_CURVE('',#11427,#11426,#6487,.T.);
#14475=EDGE_CURVE('',#11426,#11428,#6488,.T.);
#14476=EDGE_CURVE('',#11427,#11429,#6489,.T.);
#14477=EDGE_CURVE('',#11428,#11429,#289,.T.);
#14478=EDGE_CURVE('',#11430,#11425,#6490,.T.);
#14479=EDGE_CURVE('',#11429,#11430,#290,.T.);
#14480=EDGE_CURVE('',#11431,#11432,#9771,.T.);
#14481=EDGE_CURVE('',#11431,#11433,#6491,.T.);
#14482=EDGE_CURVE('',#11433,#11432,#6492,.T.);
#14483=EDGE_CURVE('',#11432,#11434,#6493,.T.);
#14484=EDGE_CURVE('',#11433,#11435,#6494,.T.);
#14485=EDGE_CURVE('',#11434,#11435,#291,.T.);
#14486=EDGE_CURVE('',#11436,#11431,#6495,.T.);
#14487=EDGE_CURVE('',#11435,#11436,#292,.T.);
#14488=EDGE_CURVE('',#11437,#11438,#9772,.T.);
#14489=EDGE_CURVE('',#11437,#11439,#6496,.T.);
#14490=EDGE_CURVE('',#11439,#11438,#6497,.T.);
#14491=EDGE_CURVE('',#11438,#11440,#6498,.T.);
#14492=EDGE_CURVE('',#11439,#11441,#6499,.T.);
#14493=EDGE_CURVE('',#11440,#11441,#293,.T.);
#14494=EDGE_CURVE('',#11442,#11437,#6500,.T.);
#14495=EDGE_CURVE('',#11441,#11442,#294,.T.);
#14496=EDGE_CURVE('',#11443,#11444,#9773,.T.);
#14497=EDGE_CURVE('',#11443,#11445,#6501,.T.);
#14498=EDGE_CURVE('',#11445,#11444,#6502,.T.);
#14499=EDGE_CURVE('',#11444,#11446,#6503,.T.);
#14500=EDGE_CURVE('',#11445,#11447,#6504,.T.);
#14501=EDGE_CURVE('',#11446,#11447,#295,.T.);
#14502=EDGE_CURVE('',#11448,#11443,#6505,.T.);
#14503=EDGE_CURVE('',#11447,#11448,#296,.T.);
#14504=EDGE_CURVE('',#11449,#11450,#9774,.T.);
#14505=EDGE_CURVE('',#11449,#11451,#6506,.T.);
#14506=EDGE_CURVE('',#11451,#11450,#6507,.T.);
#14507=EDGE_CURVE('',#11450,#11452,#6508,.T.);
#14508=EDGE_CURVE('',#11451,#11453,#6509,.T.);
#14509=EDGE_CURVE('',#11452,#11453,#297,.T.);
#14510=EDGE_CURVE('',#11454,#11449,#6510,.T.);
#14511=EDGE_CURVE('',#11453,#11454,#298,.T.);
#14512=EDGE_CURVE('',#11455,#11456,#9775,.T.);
#14513=EDGE_CURVE('',#11455,#11457,#6511,.T.);
#14514=EDGE_CURVE('',#11457,#11456,#6512,.T.);
#14515=EDGE_CURVE('',#11456,#11458,#6513,.T.);
#14516=EDGE_CURVE('',#11457,#11459,#6514,.T.);
#14517=EDGE_CURVE('',#11458,#11459,#299,.T.);
#14518=EDGE_CURVE('',#11460,#11455,#6515,.T.);
#14519=EDGE_CURVE('',#11459,#11460,#300,.T.);
#14520=EDGE_CURVE('',#11461,#11462,#9776,.T.);
#14521=EDGE_CURVE('',#11461,#11463,#6516,.T.);
#14522=EDGE_CURVE('',#11463,#11462,#6517,.T.);
#14523=EDGE_CURVE('',#11462,#11464,#6518,.T.);
#14524=EDGE_CURVE('',#11463,#11465,#6519,.T.);
#14525=EDGE_CURVE('',#11464,#11465,#301,.T.);
#14526=EDGE_CURVE('',#11466,#11461,#6520,.T.);
#14527=EDGE_CURVE('',#11465,#11466,#302,.T.);
#14528=EDGE_CURVE('',#11467,#11468,#9777,.T.);
#14529=EDGE_CURVE('',#11467,#11469,#6521,.T.);
#14530=EDGE_CURVE('',#11469,#11468,#6522,.T.);
#14531=EDGE_CURVE('',#11468,#11470,#6523,.T.);
#14532=EDGE_CURVE('',#11469,#11471,#6524,.T.);
#14533=EDGE_CURVE('',#11470,#11471,#303,.T.);
#14534=EDGE_CURVE('',#11472,#11467,#6525,.T.);
#14535=EDGE_CURVE('',#11471,#11472,#304,.T.);
#14536=EDGE_CURVE('',#11473,#11474,#9778,.T.);
#14537=EDGE_CURVE('',#11473,#11475,#6526,.T.);
#14538=EDGE_CURVE('',#11475,#11474,#6527,.T.);
#14539=EDGE_CURVE('',#11474,#11476,#6528,.T.);
#14540=EDGE_CURVE('',#11475,#11477,#6529,.T.);
#14541=EDGE_CURVE('',#11476,#11477,#305,.T.);
#14542=EDGE_CURVE('',#11478,#11473,#6530,.T.);
#14543=EDGE_CURVE('',#11477,#11478,#306,.T.);
#14544=EDGE_CURVE('',#11479,#11480,#9779,.T.);
#14545=EDGE_CURVE('',#11479,#11481,#6531,.T.);
#14546=EDGE_CURVE('',#11481,#11480,#6532,.T.);
#14547=EDGE_CURVE('',#11480,#11482,#6533,.T.);
#14548=EDGE_CURVE('',#11481,#11483,#6534,.T.);
#14549=EDGE_CURVE('',#11482,#11483,#307,.T.);
#14550=EDGE_CURVE('',#11484,#11479,#6535,.T.);
#14551=EDGE_CURVE('',#11483,#11484,#308,.T.);
#14552=EDGE_CURVE('',#11485,#11486,#9780,.T.);
#14553=EDGE_CURVE('',#11485,#11487,#6536,.T.);
#14554=EDGE_CURVE('',#11487,#11486,#6537,.T.);
#14555=EDGE_CURVE('',#11486,#11488,#6538,.T.);
#14556=EDGE_CURVE('',#11487,#11489,#6539,.T.);
#14557=EDGE_CURVE('',#11488,#11489,#309,.T.);
#14558=EDGE_CURVE('',#11490,#11485,#6540,.T.);
#14559=EDGE_CURVE('',#11489,#11490,#310,.T.);
#14560=EDGE_CURVE('',#11491,#11492,#9781,.T.);
#14561=EDGE_CURVE('',#11491,#11493,#6541,.T.);
#14562=EDGE_CURVE('',#11493,#11492,#6542,.T.);
#14563=EDGE_CURVE('',#11492,#11494,#6543,.T.);
#14564=EDGE_CURVE('',#11493,#11495,#6544,.T.);
#14565=EDGE_CURVE('',#11494,#11495,#311,.T.);
#14566=EDGE_CURVE('',#11496,#11491,#6545,.T.);
#14567=EDGE_CURVE('',#11495,#11496,#312,.T.);
#14568=EDGE_CURVE('',#11497,#11498,#9782,.T.);
#14569=EDGE_CURVE('',#11497,#11499,#6546,.T.);
#14570=EDGE_CURVE('',#11499,#11498,#6547,.T.);
#14571=EDGE_CURVE('',#11498,#11500,#6548,.T.);
#14572=EDGE_CURVE('',#11499,#11501,#6549,.T.);
#14573=EDGE_CURVE('',#11500,#11501,#313,.T.);
#14574=EDGE_CURVE('',#11502,#11497,#6550,.T.);
#14575=EDGE_CURVE('',#11501,#11502,#314,.T.);
#14576=EDGE_CURVE('',#11503,#11504,#9783,.T.);
#14577=EDGE_CURVE('',#11503,#11505,#6551,.T.);
#14578=EDGE_CURVE('',#11505,#11504,#6552,.T.);
#14579=EDGE_CURVE('',#11504,#11506,#6553,.T.);
#14580=EDGE_CURVE('',#11505,#11507,#6554,.T.);
#14581=EDGE_CURVE('',#11506,#11507,#315,.T.);
#14582=EDGE_CURVE('',#11508,#11503,#6555,.T.);
#14583=EDGE_CURVE('',#11507,#11508,#316,.T.);
#14584=EDGE_CURVE('',#11509,#11510,#9784,.T.);
#14585=EDGE_CURVE('',#11509,#11511,#6556,.T.);
#14586=EDGE_CURVE('',#11511,#11510,#6557,.T.);
#14587=EDGE_CURVE('',#11510,#11512,#6558,.T.);
#14588=EDGE_CURVE('',#11511,#11513,#6559,.T.);
#14589=EDGE_CURVE('',#11512,#11513,#317,.T.);
#14590=EDGE_CURVE('',#11514,#11509,#6560,.T.);
#14591=EDGE_CURVE('',#11513,#11514,#318,.T.);
#14592=EDGE_CURVE('',#11515,#11516,#9785,.T.);
#14593=EDGE_CURVE('',#11515,#11517,#6561,.T.);
#14594=EDGE_CURVE('',#11517,#11516,#6562,.T.);
#14595=EDGE_CURVE('',#11516,#11518,#6563,.T.);
#14596=EDGE_CURVE('',#11517,#11519,#6564,.T.);
#14597=EDGE_CURVE('',#11518,#11519,#319,.T.);
#14598=EDGE_CURVE('',#11520,#11515,#6565,.T.);
#14599=EDGE_CURVE('',#11519,#11520,#320,.T.);
#14600=EDGE_CURVE('',#11321,#11313,#9786,.T.);
#14601=EDGE_CURVE('',#11327,#11319,#9787,.T.);
#14602=EDGE_CURVE('',#11333,#11325,#9788,.T.);
#14603=EDGE_CURVE('',#11339,#11331,#9789,.T.);
#14604=EDGE_CURVE('',#11345,#11337,#9790,.T.);
#14605=EDGE_CURVE('',#11351,#11343,#9791,.T.);
#14606=EDGE_CURVE('',#11357,#11349,#9792,.T.);
#14607=EDGE_CURVE('',#11363,#11355,#9793,.T.);
#14608=EDGE_CURVE('',#11369,#11361,#9794,.T.);
#14609=EDGE_CURVE('',#11375,#11367,#9795,.T.);
#14610=EDGE_CURVE('',#11381,#11373,#9796,.T.);
#14611=EDGE_CURVE('',#11387,#11379,#9797,.T.);
#14612=EDGE_CURVE('',#11393,#11385,#9798,.T.);
#14613=EDGE_CURVE('',#11399,#11391,#9799,.T.);
#14614=EDGE_CURVE('',#11405,#11397,#9800,.T.);
#14615=EDGE_CURVE('',#11411,#11403,#9801,.T.);
#14616=EDGE_CURVE('',#11418,#11409,#9802,.T.);
#14617=EDGE_CURVE('',#11413,#11521,#6566,.T.);
#14618=EDGE_CURVE('',#11521,#11521,#9803,.T.);
#14619=EDGE_CURVE('',#11424,#11416,#9804,.T.);
#14620=EDGE_CURVE('',#11430,#11422,#9805,.T.);
#14621=EDGE_CURVE('',#11436,#11428,#9806,.T.);
#14622=EDGE_CURVE('',#11442,#11434,#9807,.T.);
#14623=EDGE_CURVE('',#11448,#11440,#9808,.T.);
#14624=EDGE_CURVE('',#11454,#11446,#9809,.T.);
#14625=EDGE_CURVE('',#11460,#11452,#9810,.T.);
#14626=EDGE_CURVE('',#11466,#11458,#9811,.T.);
#14627=EDGE_CURVE('',#11472,#11464,#9812,.T.);
#14628=EDGE_CURVE('',#11478,#11470,#9813,.T.);
#14629=EDGE_CURVE('',#11484,#11476,#9814,.T.);
#14630=EDGE_CURVE('',#11490,#11482,#9815,.T.);
#14631=EDGE_CURVE('',#11496,#11488,#9816,.T.);
#14632=EDGE_CURVE('',#11502,#11494,#9817,.T.);
#14633=EDGE_CURVE('',#11508,#11500,#9818,.T.);
#14634=EDGE_CURVE('',#11514,#11506,#9819,.T.);
#14635=EDGE_CURVE('',#11520,#11512,#9820,.T.);
#14636=EDGE_CURVE('',#11522,#11518,#9821,.T.);
#14637=EDGE_CURVE('',#11522,#11523,#6567,.T.);
#14638=EDGE_CURVE('',#11523,#11524,#9822,.T.);
#14639=EDGE_CURVE('',#11524,#11525,#6568,.T.);
#14640=EDGE_CURVE('',#11315,#11525,#9823,.T.);
#14641=EDGE_CURVE('',#11526,#11524,#6569,.T.);
#14642=EDGE_CURVE('',#11526,#11527,#6570,.T.);
#14643=EDGE_CURVE('',#11525,#11527,#321,.T.);
#14644=EDGE_CURVE('',#11527,#11522,#322,.T.);
#14645=EDGE_CURVE('',#11523,#11526,#6571,.T.);
#14646=EDGE_CURVE('',#11528,#11528,#9824,.T.);
#14647=EDGE_CURVE('',#11528,#11417,#6572,.T.);
#14648=EDGE_CURVE('',#11529,#11530,#6573,.T.);
#14649=EDGE_CURVE('',#11530,#11530,#9825,.T.);
#14650=EDGE_CURVE('',#11531,#11532,#6574,.T.);
#14651=EDGE_CURVE('',#11531,#11533,#6575,.T.);
#14652=EDGE_CURVE('',#11533,#11534,#6576,.T.);
#14653=EDGE_CURVE('',#11532,#11534,#6577,.T.);
#14654=EDGE_CURVE('',#11535,#11531,#6578,.T.);
#14655=EDGE_CURVE('',#11535,#11536,#6579,.T.);
#14656=EDGE_CURVE('',#11536,#11533,#6580,.T.);
#14657=EDGE_CURVE('',#11537,#11535,#6581,.T.);
#14658=EDGE_CURVE('',#11537,#11538,#6582,.T.);
#14659=EDGE_CURVE('',#11538,#11536,#6583,.T.);
#14660=EDGE_CURVE('',#11539,#11537,#6584,.T.);
#14661=EDGE_CURVE('',#11539,#11540,#6585,.T.);
#14662=EDGE_CURVE('',#11540,#11538,#6586,.T.);
#14663=EDGE_CURVE('',#11541,#11539,#6587,.T.);
#14664=EDGE_CURVE('',#11541,#11542,#6588,.T.);
#14665=EDGE_CURVE('',#11542,#11540,#6589,.T.);
#14666=EDGE_CURVE('',#11532,#11541,#6590,.T.);
#14667=EDGE_CURVE('',#11534,#11542,#6591,.T.);
#14668=EDGE_CURVE('',#11543,#11543,#9826,.T.);
#14669=EDGE_CURVE('',#11189,#11543,#6592,.T.);
#14670=EDGE_CURVE('',#11306,#11308,#9827,.T.);
#14671=EDGE_CURVE('',#11544,#11544,#9828,.T.);
#14672=EDGE_CURVE('',#11544,#11307,#6593,.T.);
#14673=EDGE_CURVE('',#11545,#11546,#6594,.T.);
#14674=EDGE_CURVE('',#11545,#11547,#689,.T.);
#14675=EDGE_CURVE('',#11547,#11548,#9829,.T.);
#14676=EDGE_CURVE('',#11548,#11549,#6595,.T.);
#14677=EDGE_CURVE('',#11549,#11549,#9830,.T.);
#14678=EDGE_CURVE('',#11548,#11550,#9831,.T.);
#14679=EDGE_CURVE('',#11550,#11546,#690,.T.);
#14680=EDGE_CURVE('',#11551,#11552,#6596,.T.);
#14681=EDGE_CURVE('',#11551,#11545,#691,.T.);
#14682=EDGE_CURVE('',#11546,#11552,#692,.T.);
#14683=EDGE_CURVE('',#11553,#11554,#6597,.T.);
#14684=EDGE_CURVE('',#11553,#11551,#693,.T.);
#14685=EDGE_CURVE('',#11552,#11554,#694,.T.);
#14686=EDGE_CURVE('',#11555,#11556,#6598,.T.);
#14687=EDGE_CURVE('',#11555,#11553,#695,.T.);
#14688=EDGE_CURVE('',#11554,#11556,#696,.T.);
#14689=EDGE_CURVE('',#11557,#11558,#6599,.T.);
#14690=EDGE_CURVE('',#11557,#11555,#697,.T.);
#14691=EDGE_CURVE('',#11556,#11558,#698,.T.);
#14692=EDGE_CURVE('',#11559,#11560,#6600,.T.);
#14693=EDGE_CURVE('',#11559,#11557,#699,.T.);
#14694=EDGE_CURVE('',#11558,#11560,#700,.T.);
#14695=EDGE_CURVE('',#11561,#11562,#6601,.T.);
#14696=EDGE_CURVE('',#11561,#11559,#701,.T.);
#14697=EDGE_CURVE('',#11560,#11562,#702,.T.);
#14698=EDGE_CURVE('',#11563,#11564,#6602,.T.);
#14699=EDGE_CURVE('',#11563,#11561,#703,.T.);
#14700=EDGE_CURVE('',#11562,#11564,#704,.T.);
#14701=EDGE_CURVE('',#11565,#11566,#6603,.T.);
#14702=EDGE_CURVE('',#11565,#11563,#705,.T.);
#14703=EDGE_CURVE('',#11564,#11566,#706,.T.);
#14704=EDGE_CURVE('',#11567,#11568,#6604,.T.);
#14705=EDGE_CURVE('',#11567,#11565,#707,.T.);
#14706=EDGE_CURVE('',#11566,#11568,#708,.T.);
#14707=EDGE_CURVE('',#11569,#11570,#6605,.T.);
#14708=EDGE_CURVE('',#11569,#11567,#709,.T.);
#14709=EDGE_CURVE('',#11568,#11570,#710,.T.);
#14710=EDGE_CURVE('',#11571,#11572,#6606,.T.);
#14711=EDGE_CURVE('',#11571,#11569,#711,.T.);
#14712=EDGE_CURVE('',#11570,#11572,#712,.T.);
#14713=EDGE_CURVE('',#11573,#11574,#6607,.T.);
#14714=EDGE_CURVE('',#11573,#11571,#713,.T.);
#14715=EDGE_CURVE('',#11572,#11574,#714,.T.);
#14716=EDGE_CURVE('',#11575,#11576,#6608,.T.);
#14717=EDGE_CURVE('',#11575,#11573,#715,.T.);
#14718=EDGE_CURVE('',#11574,#11576,#716,.T.);
#14719=EDGE_CURVE('',#11577,#11578,#6609,.T.);
#14720=EDGE_CURVE('',#11577,#11575,#717,.T.);
#14721=EDGE_CURVE('',#11576,#11578,#718,.T.);
#14722=EDGE_CURVE('',#11579,#11580,#6610,.T.);
#14723=EDGE_CURVE('',#11579,#11577,#719,.T.);
#14724=EDGE_CURVE('',#11578,#11580,#720,.T.);
#14725=EDGE_CURVE('',#11581,#11582,#6611,.T.);
#14726=EDGE_CURVE('',#11581,#11579,#721,.T.);
#14727=EDGE_CURVE('',#11580,#11582,#722,.T.);
#14728=EDGE_CURVE('',#11583,#11584,#6612,.T.);
#14729=EDGE_CURVE('',#11583,#11581,#723,.T.);
#14730=EDGE_CURVE('',#11582,#11584,#724,.T.);
#14731=EDGE_CURVE('',#11585,#11586,#6613,.T.);
#14732=EDGE_CURVE('',#11585,#11583,#725,.T.);
#14733=EDGE_CURVE('',#11584,#11586,#726,.T.);
#14734=EDGE_CURVE('',#11587,#11588,#6614,.T.);
#14735=EDGE_CURVE('',#11587,#11585,#727,.T.);
#14736=EDGE_CURVE('',#11586,#11588,#728,.T.);
#14737=EDGE_CURVE('',#11589,#11590,#6615,.T.);
#14738=EDGE_CURVE('',#11589,#11587,#729,.T.);
#14739=EDGE_CURVE('',#11588,#11590,#730,.T.);
#14740=EDGE_CURVE('',#11591,#11592,#6616,.T.);
#14741=EDGE_CURVE('',#11591,#11589,#731,.T.);
#14742=EDGE_CURVE('',#11590,#11592,#732,.T.);
#14743=EDGE_CURVE('',#11593,#11594,#6617,.T.);
#14744=EDGE_CURVE('',#11593,#11591,#733,.T.);
#14745=EDGE_CURVE('',#11592,#11594,#734,.T.);
#14746=EDGE_CURVE('',#11595,#11596,#6618,.T.);
#14747=EDGE_CURVE('',#11595,#11597,#735,.T.);
#14748=EDGE_CURVE('',#11598,#11597,#9832,.T.);
#14749=EDGE_CURVE('',#11596,#11598,#736,.T.);
#14750=EDGE_CURVE('',#11599,#11600,#6619,.T.);
#14751=EDGE_CURVE('',#11599,#11595,#737,.T.);
#14752=EDGE_CURVE('',#11600,#11596,#738,.T.);
#14753=EDGE_CURVE('',#11601,#11602,#6620,.T.);
#14754=EDGE_CURVE('',#11601,#11599,#739,.T.);
#14755=EDGE_CURVE('',#11602,#11600,#740,.T.);
#14756=EDGE_CURVE('',#11603,#11604,#6621,.T.);
#14757=EDGE_CURVE('',#11603,#11601,#741,.T.);
#14758=EDGE_CURVE('',#11604,#11602,#742,.T.);
#14759=EDGE_CURVE('',#11605,#11606,#6622,.T.);
#14760=EDGE_CURVE('',#11605,#11603,#743,.T.);
#14761=EDGE_CURVE('',#11606,#11604,#744,.T.);
#14762=EDGE_CURVE('',#11607,#11608,#6623,.T.);
#14763=EDGE_CURVE('',#11607,#11605,#745,.T.);
#14764=EDGE_CURVE('',#11608,#11606,#746,.T.);
#14765=EDGE_CURVE('',#11609,#11610,#6624,.T.);
#14766=EDGE_CURVE('',#11609,#11607,#747,.T.);
#14767=EDGE_CURVE('',#11610,#11608,#748,.T.);
#14768=EDGE_CURVE('',#11611,#11612,#6625,.T.);
#14769=EDGE_CURVE('',#11611,#11609,#749,.T.);
#14770=EDGE_CURVE('',#11612,#11610,#750,.T.);
#14771=EDGE_CURVE('',#11613,#11614,#6626,.T.);
#14772=EDGE_CURVE('',#11613,#11611,#751,.T.);
#14773=EDGE_CURVE('',#11614,#11612,#752,.T.);
#14774=EDGE_CURVE('',#11615,#11616,#6627,.T.);
#14775=EDGE_CURVE('',#11615,#11613,#753,.T.);
#14776=EDGE_CURVE('',#11616,#11614,#754,.T.);
#14777=EDGE_CURVE('',#11617,#11618,#6628,.T.);
#14778=EDGE_CURVE('',#11617,#11615,#755,.T.);
#14779=EDGE_CURVE('',#11618,#11616,#756,.T.);
#14780=EDGE_CURVE('',#11619,#11620,#6629,.T.);
#14781=EDGE_CURVE('',#11619,#11617,#757,.T.);
#14782=EDGE_CURVE('',#11620,#11618,#758,.T.);
#14783=EDGE_CURVE('',#11621,#11622,#6630,.T.);
#14784=EDGE_CURVE('',#11621,#11619,#759,.T.);
#14785=EDGE_CURVE('',#11622,#11620,#760,.T.);
#14786=EDGE_CURVE('',#11623,#11624,#6631,.T.);
#14787=EDGE_CURVE('',#11623,#11621,#761,.T.);
#14788=EDGE_CURVE('',#11624,#11622,#762,.T.);
#14789=EDGE_CURVE('',#11625,#11626,#6632,.T.);
#14790=EDGE_CURVE('',#11625,#11623,#763,.T.);
#14791=EDGE_CURVE('',#11626,#11624,#764,.T.);
#14792=EDGE_CURVE('',#11627,#11628,#6633,.T.);
#14793=EDGE_CURVE('',#11627,#11625,#765,.T.);
#14794=EDGE_CURVE('',#11628,#11626,#766,.T.);
#14795=EDGE_CURVE('',#11629,#11630,#6634,.T.);
#14796=EDGE_CURVE('',#11629,#11627,#767,.T.);
#14797=EDGE_CURVE('',#11630,#11628,#768,.T.);
#14798=EDGE_CURVE('',#11631,#11632,#6635,.T.);
#14799=EDGE_CURVE('',#11631,#11629,#769,.T.);
#14800=EDGE_CURVE('',#11632,#11630,#770,.T.);
#14801=EDGE_CURVE('',#11633,#11634,#6636,.T.);
#14802=EDGE_CURVE('',#11633,#11631,#771,.T.);
#14803=EDGE_CURVE('',#11634,#11632,#772,.T.);
#14804=EDGE_CURVE('',#11635,#11636,#6637,.T.);
#14805=EDGE_CURVE('',#11635,#11633,#773,.T.);
#14806=EDGE_CURVE('',#11636,#11634,#774,.T.);
#14807=EDGE_CURVE('',#11637,#11638,#6638,.T.);
#14808=EDGE_CURVE('',#11637,#11635,#775,.T.);
#14809=EDGE_CURVE('',#11638,#11636,#776,.T.);
#14810=EDGE_CURVE('',#11639,#11640,#6639,.T.);
#14811=EDGE_CURVE('',#11639,#11637,#777,.T.);
#14812=EDGE_CURVE('',#11640,#11638,#778,.T.);
#14813=EDGE_CURVE('',#11641,#11642,#6640,.T.);
#14814=EDGE_CURVE('',#11641,#11639,#779,.T.);
#14815=EDGE_CURVE('',#11642,#11640,#780,.T.);
#14816=EDGE_CURVE('',#11643,#11644,#6641,.T.);
#14817=EDGE_CURVE('',#11645,#11643,#9833,.T.);
#14818=EDGE_CURVE('',#11645,#11641,#781,.T.);
#14819=EDGE_CURVE('',#11644,#11642,#782,.T.);
#14820=EDGE_CURVE('',#11597,#11646,#783,.T.);
#14821=EDGE_CURVE('',#11647,#11646,#9834,.T.);
#14822=EDGE_CURVE('',#11648,#11647,#9835,.T.);
#14823=EDGE_CURVE('',#11648,#11598,#784,.T.);
#14824=EDGE_CURVE('',#11594,#11648,#785,.T.);
#14825=EDGE_CURVE('',#11649,#11550,#786,.T.);
#14826=EDGE_CURVE('',#11649,#11644,#787,.T.);
#14827=EDGE_CURVE('',#11547,#11645,#788,.T.);
#14828=EDGE_CURVE('',#11643,#11649,#9836,.T.);
#14829=EDGE_CURVE('',#11646,#11593,#789,.T.);
#14830=EDGE_CURVE('',#11650,#11651,#9837,.T.);
#14831=EDGE_CURVE('',#11650,#11652,#6642,.T.);
#14832=EDGE_CURVE('',#11652,#11651,#6643,.T.);
#14833=EDGE_CURVE('',#11651,#11653,#6644,.T.);
#14834=EDGE_CURVE('',#11652,#11654,#6645,.T.);
#14835=EDGE_CURVE('',#11653,#11654,#323,.T.);
#14836=EDGE_CURVE('',#11655,#11650,#6646,.T.);
#14837=EDGE_CURVE('',#11654,#11655,#324,.T.);
#14838=EDGE_CURVE('',#11656,#11657,#9838,.T.);
#14839=EDGE_CURVE('',#11656,#11658,#6647,.T.);
#14840=EDGE_CURVE('',#11658,#11657,#6648,.T.);
#14841=EDGE_CURVE('',#11657,#11659,#6649,.T.);
#14842=EDGE_CURVE('',#11658,#11660,#6650,.T.);
#14843=EDGE_CURVE('',#11659,#11660,#325,.T.);
#14844=EDGE_CURVE('',#11661,#11656,#6651,.T.);
#14845=EDGE_CURVE('',#11660,#11661,#326,.T.);
#14846=EDGE_CURVE('',#11662,#11663,#9839,.T.);
#14847=EDGE_CURVE('',#11662,#11664,#6652,.T.);
#14848=EDGE_CURVE('',#11664,#11663,#6653,.T.);
#14849=EDGE_CURVE('',#11663,#11665,#6654,.T.);
#14850=EDGE_CURVE('',#11664,#11666,#6655,.T.);
#14851=EDGE_CURVE('',#11665,#11666,#327,.T.);
#14852=EDGE_CURVE('',#11667,#11662,#6656,.T.);
#14853=EDGE_CURVE('',#11666,#11667,#328,.T.);
#14854=EDGE_CURVE('',#11668,#11669,#9840,.T.);
#14855=EDGE_CURVE('',#11668,#11670,#6657,.T.);
#14856=EDGE_CURVE('',#11670,#11669,#6658,.T.);
#14857=EDGE_CURVE('',#11669,#11671,#6659,.T.);
#14858=EDGE_CURVE('',#11670,#11672,#6660,.T.);
#14859=EDGE_CURVE('',#11671,#11672,#329,.T.);
#14860=EDGE_CURVE('',#11673,#11668,#6661,.T.);
#14861=EDGE_CURVE('',#11672,#11673,#330,.T.);
#14862=EDGE_CURVE('',#11674,#11675,#9841,.T.);
#14863=EDGE_CURVE('',#11674,#11676,#6662,.T.);
#14864=EDGE_CURVE('',#11676,#11675,#6663,.T.);
#14865=EDGE_CURVE('',#11675,#11677,#6664,.T.);
#14866=EDGE_CURVE('',#11676,#11678,#6665,.T.);
#14867=EDGE_CURVE('',#11677,#11678,#331,.T.);
#14868=EDGE_CURVE('',#11679,#11674,#6666,.T.);
#14869=EDGE_CURVE('',#11678,#11679,#332,.T.);
#14870=EDGE_CURVE('',#11680,#11681,#9842,.T.);
#14871=EDGE_CURVE('',#11680,#11682,#6667,.T.);
#14872=EDGE_CURVE('',#11682,#11681,#6668,.T.);
#14873=EDGE_CURVE('',#11681,#11683,#6669,.T.);
#14874=EDGE_CURVE('',#11682,#11684,#6670,.T.);
#14875=EDGE_CURVE('',#11683,#11684,#333,.T.);
#14876=EDGE_CURVE('',#11685,#11680,#6671,.T.);
#14877=EDGE_CURVE('',#11684,#11685,#334,.T.);
#14878=EDGE_CURVE('',#11686,#11687,#9843,.T.);
#14879=EDGE_CURVE('',#11686,#11688,#6672,.T.);
#14880=EDGE_CURVE('',#11688,#11687,#6673,.T.);
#14881=EDGE_CURVE('',#11687,#11689,#6674,.T.);
#14882=EDGE_CURVE('',#11688,#11690,#6675,.T.);
#14883=EDGE_CURVE('',#11689,#11690,#335,.T.);
#14884=EDGE_CURVE('',#11691,#11686,#6676,.T.);
#14885=EDGE_CURVE('',#11690,#11691,#336,.T.);
#14886=EDGE_CURVE('',#11692,#11693,#9844,.T.);
#14887=EDGE_CURVE('',#11692,#11694,#6677,.T.);
#14888=EDGE_CURVE('',#11694,#11693,#6678,.T.);
#14889=EDGE_CURVE('',#11693,#11695,#6679,.T.);
#14890=EDGE_CURVE('',#11694,#11696,#6680,.T.);
#14891=EDGE_CURVE('',#11695,#11696,#337,.T.);
#14892=EDGE_CURVE('',#11697,#11692,#6681,.T.);
#14893=EDGE_CURVE('',#11696,#11697,#338,.T.);
#14894=EDGE_CURVE('',#11698,#11699,#9845,.T.);
#14895=EDGE_CURVE('',#11698,#11700,#6682,.T.);
#14896=EDGE_CURVE('',#11700,#11699,#6683,.T.);
#14897=EDGE_CURVE('',#11699,#11701,#6684,.T.);
#14898=EDGE_CURVE('',#11700,#11702,#6685,.T.);
#14899=EDGE_CURVE('',#11701,#11702,#339,.T.);
#14900=EDGE_CURVE('',#11703,#11698,#6686,.T.);
#14901=EDGE_CURVE('',#11702,#11703,#340,.T.);
#14902=EDGE_CURVE('',#11704,#11705,#9846,.T.);
#14903=EDGE_CURVE('',#11704,#11706,#6687,.T.);
#14904=EDGE_CURVE('',#11706,#11705,#6688,.T.);
#14905=EDGE_CURVE('',#11705,#11707,#6689,.T.);
#14906=EDGE_CURVE('',#11706,#11708,#6690,.T.);
#14907=EDGE_CURVE('',#11707,#11708,#341,.T.);
#14908=EDGE_CURVE('',#11709,#11704,#6691,.T.);
#14909=EDGE_CURVE('',#11708,#11709,#342,.T.);
#14910=EDGE_CURVE('',#11710,#11711,#9847,.T.);
#14911=EDGE_CURVE('',#11710,#11712,#6692,.T.);
#14912=EDGE_CURVE('',#11712,#11711,#6693,.T.);
#14913=EDGE_CURVE('',#11711,#11713,#6694,.T.);
#14914=EDGE_CURVE('',#11712,#11714,#6695,.T.);
#14915=EDGE_CURVE('',#11713,#11714,#343,.T.);
#14916=EDGE_CURVE('',#11715,#11710,#6696,.T.);
#14917=EDGE_CURVE('',#11714,#11715,#344,.T.);
#14918=EDGE_CURVE('',#11716,#11717,#9848,.T.);
#14919=EDGE_CURVE('',#11716,#11718,#6697,.T.);
#14920=EDGE_CURVE('',#11718,#11717,#6698,.T.);
#14921=EDGE_CURVE('',#11717,#11719,#6699,.T.);
#14922=EDGE_CURVE('',#11718,#11720,#6700,.T.);
#14923=EDGE_CURVE('',#11719,#11720,#345,.T.);
#14924=EDGE_CURVE('',#11721,#11716,#6701,.T.);
#14925=EDGE_CURVE('',#11720,#11721,#346,.T.);
#14926=EDGE_CURVE('',#11722,#11723,#9849,.T.);
#14927=EDGE_CURVE('',#11722,#11724,#6702,.T.);
#14928=EDGE_CURVE('',#11724,#11723,#6703,.T.);
#14929=EDGE_CURVE('',#11723,#11725,#6704,.T.);
#14930=EDGE_CURVE('',#11724,#11726,#6705,.T.);
#14931=EDGE_CURVE('',#11725,#11726,#347,.T.);
#14932=EDGE_CURVE('',#11727,#11722,#6706,.T.);
#14933=EDGE_CURVE('',#11726,#11727,#348,.T.);
#14934=EDGE_CURVE('',#11728,#11729,#9850,.T.);
#14935=EDGE_CURVE('',#11728,#11730,#6707,.T.);
#14936=EDGE_CURVE('',#11730,#11729,#6708,.T.);
#14937=EDGE_CURVE('',#11729,#11731,#6709,.T.);
#14938=EDGE_CURVE('',#11730,#11732,#6710,.T.);
#14939=EDGE_CURVE('',#11731,#11732,#349,.T.);
#14940=EDGE_CURVE('',#11733,#11728,#6711,.T.);
#14941=EDGE_CURVE('',#11732,#11733,#350,.T.);
#14942=EDGE_CURVE('',#11734,#11735,#9851,.T.);
#14943=EDGE_CURVE('',#11734,#11736,#6712,.T.);
#14944=EDGE_CURVE('',#11736,#11735,#6713,.T.);
#14945=EDGE_CURVE('',#11735,#11737,#6714,.T.);
#14946=EDGE_CURVE('',#11736,#11738,#6715,.T.);
#14947=EDGE_CURVE('',#11737,#11738,#351,.T.);
#14948=EDGE_CURVE('',#11739,#11734,#6716,.T.);
#14949=EDGE_CURVE('',#11738,#11739,#352,.T.);
#14950=EDGE_CURVE('',#11740,#11741,#9852,.T.);
#14951=EDGE_CURVE('',#11740,#11742,#6717,.T.);
#14952=EDGE_CURVE('',#11742,#11741,#6718,.T.);
#14953=EDGE_CURVE('',#11741,#11743,#6719,.T.);
#14954=EDGE_CURVE('',#11742,#11744,#6720,.T.);
#14955=EDGE_CURVE('',#11743,#11744,#353,.T.);
#14956=EDGE_CURVE('',#11745,#11740,#6721,.T.);
#14957=EDGE_CURVE('',#11744,#11745,#354,.T.);
#14958=EDGE_CURVE('',#11746,#11747,#9853,.T.);
#14959=EDGE_CURVE('',#11746,#11748,#6722,.T.);
#14960=EDGE_CURVE('',#11748,#11747,#6723,.T.);
#14961=EDGE_CURVE('',#11747,#11749,#6724,.T.);
#14962=EDGE_CURVE('',#11748,#11750,#6725,.T.);
#14963=EDGE_CURVE('',#11749,#11750,#355,.T.);
#14964=EDGE_CURVE('',#11751,#11746,#6726,.T.);
#14965=EDGE_CURVE('',#11750,#11751,#356,.T.);
#14966=EDGE_CURVE('',#11752,#11753,#9854,.T.);
#14967=EDGE_CURVE('',#11752,#11754,#6727,.T.);
#14968=EDGE_CURVE('',#11754,#11755,#6728,.T.);
#14969=EDGE_CURVE('',#11753,#11755,#9855,.T.);
#14970=EDGE_CURVE('',#11755,#11756,#6729,.T.);
#14971=EDGE_CURVE('',#11754,#11757,#6730,.T.);
#14972=EDGE_CURVE('',#11756,#11757,#357,.T.);
#14973=EDGE_CURVE('',#11758,#11752,#6731,.T.);
#14974=EDGE_CURVE('',#11757,#11758,#358,.T.);
#14975=EDGE_CURVE('',#11759,#11760,#9856,.T.);
#14976=EDGE_CURVE('',#11759,#11761,#6732,.T.);
#14977=EDGE_CURVE('',#11761,#11760,#6733,.T.);
#14978=EDGE_CURVE('',#11760,#11762,#6734,.T.);
#14979=EDGE_CURVE('',#11761,#11763,#6735,.T.);
#14980=EDGE_CURVE('',#11762,#11763,#359,.T.);
#14981=EDGE_CURVE('',#11764,#11759,#6736,.T.);
#14982=EDGE_CURVE('',#11763,#11764,#360,.T.);
#14983=EDGE_CURVE('',#11765,#11766,#9857,.T.);
#14984=EDGE_CURVE('',#11765,#11767,#6737,.T.);
#14985=EDGE_CURVE('',#11767,#11766,#6738,.T.);
#14986=EDGE_CURVE('',#11766,#11768,#6739,.T.);
#14987=EDGE_CURVE('',#11767,#11769,#6740,.T.);
#14988=EDGE_CURVE('',#11768,#11769,#361,.T.);
#14989=EDGE_CURVE('',#11770,#11765,#6741,.T.);
#14990=EDGE_CURVE('',#11769,#11770,#362,.T.);
#14991=EDGE_CURVE('',#11771,#11772,#9858,.T.);
#14992=EDGE_CURVE('',#11771,#11773,#6742,.T.);
#14993=EDGE_CURVE('',#11773,#11772,#6743,.T.);
#14994=EDGE_CURVE('',#11772,#11774,#6744,.T.);
#14995=EDGE_CURVE('',#11773,#11775,#6745,.T.);
#14996=EDGE_CURVE('',#11774,#11775,#363,.T.);
#14997=EDGE_CURVE('',#11776,#11771,#6746,.T.);
#14998=EDGE_CURVE('',#11775,#11776,#364,.T.);
#14999=EDGE_CURVE('',#11777,#11778,#9859,.T.);
#15000=EDGE_CURVE('',#11777,#11779,#6747,.T.);
#15001=EDGE_CURVE('',#11779,#11778,#6748,.T.);
#15002=EDGE_CURVE('',#11778,#11780,#6749,.T.);
#15003=EDGE_CURVE('',#11779,#11781,#6750,.T.);
#15004=EDGE_CURVE('',#11780,#11781,#365,.T.);
#15005=EDGE_CURVE('',#11782,#11777,#6751,.T.);
#15006=EDGE_CURVE('',#11781,#11782,#366,.T.);
#15007=EDGE_CURVE('',#11783,#11784,#9860,.T.);
#15008=EDGE_CURVE('',#11783,#11785,#6752,.T.);
#15009=EDGE_CURVE('',#11785,#11784,#6753,.T.);
#15010=EDGE_CURVE('',#11784,#11786,#6754,.T.);
#15011=EDGE_CURVE('',#11785,#11787,#6755,.T.);
#15012=EDGE_CURVE('',#11786,#11787,#367,.T.);
#15013=EDGE_CURVE('',#11788,#11783,#6756,.T.);
#15014=EDGE_CURVE('',#11787,#11788,#368,.T.);
#15015=EDGE_CURVE('',#11789,#11790,#9861,.T.);
#15016=EDGE_CURVE('',#11789,#11791,#6757,.T.);
#15017=EDGE_CURVE('',#11791,#11790,#6758,.T.);
#15018=EDGE_CURVE('',#11790,#11792,#6759,.T.);
#15019=EDGE_CURVE('',#11791,#11793,#6760,.T.);
#15020=EDGE_CURVE('',#11792,#11793,#369,.T.);
#15021=EDGE_CURVE('',#11794,#11789,#6761,.T.);
#15022=EDGE_CURVE('',#11793,#11794,#370,.T.);
#15023=EDGE_CURVE('',#11795,#11796,#9862,.T.);
#15024=EDGE_CURVE('',#11795,#11797,#6762,.T.);
#15025=EDGE_CURVE('',#11797,#11796,#6763,.T.);
#15026=EDGE_CURVE('',#11796,#11798,#6764,.T.);
#15027=EDGE_CURVE('',#11797,#11799,#6765,.T.);
#15028=EDGE_CURVE('',#11798,#11799,#371,.T.);
#15029=EDGE_CURVE('',#11800,#11795,#6766,.T.);
#15030=EDGE_CURVE('',#11799,#11800,#372,.T.);
#15031=EDGE_CURVE('',#11801,#11802,#9863,.T.);
#15032=EDGE_CURVE('',#11801,#11803,#6767,.T.);
#15033=EDGE_CURVE('',#11803,#11802,#6768,.T.);
#15034=EDGE_CURVE('',#11802,#11804,#6769,.T.);
#15035=EDGE_CURVE('',#11803,#11805,#6770,.T.);
#15036=EDGE_CURVE('',#11804,#11805,#373,.T.);
#15037=EDGE_CURVE('',#11806,#11801,#6771,.T.);
#15038=EDGE_CURVE('',#11805,#11806,#374,.T.);
#15039=EDGE_CURVE('',#11807,#11808,#9864,.T.);
#15040=EDGE_CURVE('',#11807,#11809,#6772,.T.);
#15041=EDGE_CURVE('',#11809,#11808,#6773,.T.);
#15042=EDGE_CURVE('',#11808,#11810,#6774,.T.);
#15043=EDGE_CURVE('',#11809,#11811,#6775,.T.);
#15044=EDGE_CURVE('',#11810,#11811,#375,.T.);
#15045=EDGE_CURVE('',#11812,#11807,#6776,.T.);
#15046=EDGE_CURVE('',#11811,#11812,#376,.T.);
#15047=EDGE_CURVE('',#11813,#11814,#9865,.T.);
#15048=EDGE_CURVE('',#11813,#11815,#6777,.T.);
#15049=EDGE_CURVE('',#11815,#11814,#6778,.T.);
#15050=EDGE_CURVE('',#11814,#11816,#6779,.T.);
#15051=EDGE_CURVE('',#11815,#11817,#6780,.T.);
#15052=EDGE_CURVE('',#11816,#11817,#377,.T.);
#15053=EDGE_CURVE('',#11818,#11813,#6781,.T.);
#15054=EDGE_CURVE('',#11817,#11818,#378,.T.);
#15055=EDGE_CURVE('',#11819,#11820,#9866,.T.);
#15056=EDGE_CURVE('',#11819,#11821,#6782,.T.);
#15057=EDGE_CURVE('',#11821,#11820,#6783,.T.);
#15058=EDGE_CURVE('',#11820,#11822,#6784,.T.);
#15059=EDGE_CURVE('',#11821,#11823,#6785,.T.);
#15060=EDGE_CURVE('',#11822,#11823,#379,.T.);
#15061=EDGE_CURVE('',#11824,#11819,#6786,.T.);
#15062=EDGE_CURVE('',#11823,#11824,#380,.T.);
#15063=EDGE_CURVE('',#11825,#11826,#9867,.T.);
#15064=EDGE_CURVE('',#11825,#11827,#6787,.T.);
#15065=EDGE_CURVE('',#11827,#11826,#6788,.T.);
#15066=EDGE_CURVE('',#11826,#11828,#6789,.T.);
#15067=EDGE_CURVE('',#11827,#11829,#6790,.T.);
#15068=EDGE_CURVE('',#11828,#11829,#381,.T.);
#15069=EDGE_CURVE('',#11830,#11825,#6791,.T.);
#15070=EDGE_CURVE('',#11829,#11830,#382,.T.);
#15071=EDGE_CURVE('',#11831,#11832,#9868,.T.);
#15072=EDGE_CURVE('',#11831,#11833,#6792,.T.);
#15073=EDGE_CURVE('',#11833,#11832,#6793,.T.);
#15074=EDGE_CURVE('',#11832,#11834,#6794,.T.);
#15075=EDGE_CURVE('',#11833,#11835,#6795,.T.);
#15076=EDGE_CURVE('',#11834,#11835,#383,.T.);
#15077=EDGE_CURVE('',#11836,#11831,#6796,.T.);
#15078=EDGE_CURVE('',#11835,#11836,#384,.T.);
#15079=EDGE_CURVE('',#11837,#11838,#9869,.T.);
#15080=EDGE_CURVE('',#11837,#11839,#6797,.T.);
#15081=EDGE_CURVE('',#11839,#11838,#6798,.T.);
#15082=EDGE_CURVE('',#11838,#11840,#6799,.T.);
#15083=EDGE_CURVE('',#11839,#11841,#6800,.T.);
#15084=EDGE_CURVE('',#11840,#11841,#385,.T.);
#15085=EDGE_CURVE('',#11842,#11837,#6801,.T.);
#15086=EDGE_CURVE('',#11841,#11842,#386,.T.);
#15087=EDGE_CURVE('',#11843,#11844,#9870,.T.);
#15088=EDGE_CURVE('',#11843,#11845,#6802,.T.);
#15089=EDGE_CURVE('',#11845,#11844,#6803,.T.);
#15090=EDGE_CURVE('',#11844,#11846,#6804,.T.);
#15091=EDGE_CURVE('',#11845,#11847,#6805,.T.);
#15092=EDGE_CURVE('',#11846,#11847,#387,.T.);
#15093=EDGE_CURVE('',#11848,#11843,#6806,.T.);
#15094=EDGE_CURVE('',#11847,#11848,#388,.T.);
#15095=EDGE_CURVE('',#11849,#11850,#9871,.T.);
#15096=EDGE_CURVE('',#11849,#11851,#6807,.T.);
#15097=EDGE_CURVE('',#11851,#11850,#6808,.T.);
#15098=EDGE_CURVE('',#11850,#11852,#6809,.T.);
#15099=EDGE_CURVE('',#11851,#11853,#6810,.T.);
#15100=EDGE_CURVE('',#11852,#11853,#389,.T.);
#15101=EDGE_CURVE('',#11854,#11849,#6811,.T.);
#15102=EDGE_CURVE('',#11853,#11854,#390,.T.);
#15103=EDGE_CURVE('',#11855,#11856,#9872,.T.);
#15104=EDGE_CURVE('',#11855,#11857,#6812,.T.);
#15105=EDGE_CURVE('',#11857,#11856,#6813,.T.);
#15106=EDGE_CURVE('',#11856,#11858,#6814,.T.);
#15107=EDGE_CURVE('',#11857,#11859,#6815,.T.);
#15108=EDGE_CURVE('',#11858,#11859,#391,.T.);
#15109=EDGE_CURVE('',#11860,#11855,#6816,.T.);
#15110=EDGE_CURVE('',#11859,#11860,#392,.T.);
#15111=EDGE_CURVE('',#11661,#11653,#9873,.T.);
#15112=EDGE_CURVE('',#11667,#11659,#9874,.T.);
#15113=EDGE_CURVE('',#11673,#11665,#9875,.T.);
#15114=EDGE_CURVE('',#11679,#11671,#9876,.T.);
#15115=EDGE_CURVE('',#11685,#11677,#9877,.T.);
#15116=EDGE_CURVE('',#11691,#11683,#9878,.T.);
#15117=EDGE_CURVE('',#11697,#11689,#9879,.T.);
#15118=EDGE_CURVE('',#11703,#11695,#9880,.T.);
#15119=EDGE_CURVE('',#11709,#11701,#9881,.T.);
#15120=EDGE_CURVE('',#11715,#11707,#9882,.T.);
#15121=EDGE_CURVE('',#11721,#11713,#9883,.T.);
#15122=EDGE_CURVE('',#11727,#11719,#9884,.T.);
#15123=EDGE_CURVE('',#11733,#11725,#9885,.T.);
#15124=EDGE_CURVE('',#11739,#11731,#9886,.T.);
#15125=EDGE_CURVE('',#11745,#11737,#9887,.T.);
#15126=EDGE_CURVE('',#11751,#11743,#9888,.T.);
#15127=EDGE_CURVE('',#11758,#11749,#9889,.T.);
#15128=EDGE_CURVE('',#11753,#11861,#6817,.T.);
#15129=EDGE_CURVE('',#11861,#11861,#9890,.T.);
#15130=EDGE_CURVE('',#11764,#11756,#9891,.T.);
#15131=EDGE_CURVE('',#11770,#11762,#9892,.T.);
#15132=EDGE_CURVE('',#11776,#11768,#9893,.T.);
#15133=EDGE_CURVE('',#11782,#11774,#9894,.T.);
#15134=EDGE_CURVE('',#11788,#11780,#9895,.T.);
#15135=EDGE_CURVE('',#11794,#11786,#9896,.T.);
#15136=EDGE_CURVE('',#11800,#11792,#9897,.T.);
#15137=EDGE_CURVE('',#11806,#11798,#9898,.T.);
#15138=EDGE_CURVE('',#11812,#11804,#9899,.T.);
#15139=EDGE_CURVE('',#11818,#11810,#9900,.T.);
#15140=EDGE_CURVE('',#11824,#11816,#9901,.T.);
#15141=EDGE_CURVE('',#11830,#11822,#9902,.T.);
#15142=EDGE_CURVE('',#11836,#11828,#9903,.T.);
#15143=EDGE_CURVE('',#11842,#11834,#9904,.T.);
#15144=EDGE_CURVE('',#11848,#11840,#9905,.T.);
#15145=EDGE_CURVE('',#11854,#11846,#9906,.T.);
#15146=EDGE_CURVE('',#11860,#11852,#9907,.T.);
#15147=EDGE_CURVE('',#11862,#11858,#9908,.T.);
#15148=EDGE_CURVE('',#11862,#11863,#6818,.T.);
#15149=EDGE_CURVE('',#11863,#11864,#9909,.T.);
#15150=EDGE_CURVE('',#11864,#11865,#6819,.T.);
#15151=EDGE_CURVE('',#11655,#11865,#9910,.T.);
#15152=EDGE_CURVE('',#11866,#11864,#6820,.T.);
#15153=EDGE_CURVE('',#11866,#11867,#6821,.T.);
#15154=EDGE_CURVE('',#11865,#11867,#393,.T.);
#15155=EDGE_CURVE('',#11867,#11862,#394,.T.);
#15156=EDGE_CURVE('',#11863,#11866,#6822,.T.);
#15157=EDGE_CURVE('',#11868,#11868,#9911,.T.);
#15158=EDGE_CURVE('',#11868,#11757,#6823,.T.);
#15159=EDGE_CURVE('',#11869,#11870,#6824,.T.);
#15160=EDGE_CURVE('',#11870,#11870,#9912,.T.);
#15161=EDGE_CURVE('',#11871,#11872,#6825,.T.);
#15162=EDGE_CURVE('',#11871,#11873,#6826,.T.);
#15163=EDGE_CURVE('',#11873,#11874,#6827,.T.);
#15164=EDGE_CURVE('',#11872,#11874,#6828,.T.);
#15165=EDGE_CURVE('',#11875,#11871,#6829,.T.);
#15166=EDGE_CURVE('',#11875,#11876,#6830,.T.);
#15167=EDGE_CURVE('',#11876,#11873,#6831,.T.);
#15168=EDGE_CURVE('',#11877,#11875,#6832,.T.);
#15169=EDGE_CURVE('',#11877,#11878,#6833,.T.);
#15170=EDGE_CURVE('',#11878,#11876,#6834,.T.);
#15171=EDGE_CURVE('',#11879,#11877,#6835,.T.);
#15172=EDGE_CURVE('',#11879,#11880,#6836,.T.);
#15173=EDGE_CURVE('',#11880,#11878,#6837,.T.);
#15174=EDGE_CURVE('',#11881,#11879,#6838,.T.);
#15175=EDGE_CURVE('',#11881,#11882,#6839,.T.);
#15176=EDGE_CURVE('',#11882,#11880,#6840,.T.);
#15177=EDGE_CURVE('',#11872,#11881,#6841,.T.);
#15178=EDGE_CURVE('',#11874,#11882,#6842,.T.);
#15179=EDGE_CURVE('',#11883,#11883,#9913,.T.);
#15180=EDGE_CURVE('',#11549,#11883,#6843,.T.);
#15181=EDGE_CURVE('',#11646,#11648,#9914,.T.);
#15182=EDGE_CURVE('',#11884,#11884,#9915,.T.);
#15183=EDGE_CURVE('',#11884,#11647,#6844,.T.);
#15184=EDGE_CURVE('',#11885,#11886,#6845,.T.);
#15185=EDGE_CURVE('',#11885,#11887,#790,.T.);
#15186=EDGE_CURVE('',#11887,#11888,#9916,.T.);
#15187=EDGE_CURVE('',#11888,#11889,#6846,.T.);
#15188=EDGE_CURVE('',#11889,#11889,#9917,.T.);
#15189=EDGE_CURVE('',#11888,#11890,#9918,.T.);
#15190=EDGE_CURVE('',#11890,#11886,#791,.T.);
#15191=EDGE_CURVE('',#11891,#11892,#6847,.T.);
#15192=EDGE_CURVE('',#11891,#11885,#792,.T.);
#15193=EDGE_CURVE('',#11886,#11892,#793,.T.);
#15194=EDGE_CURVE('',#11893,#11894,#6848,.T.);
#15195=EDGE_CURVE('',#11893,#11891,#794,.T.);
#15196=EDGE_CURVE('',#11892,#11894,#795,.T.);
#15197=EDGE_CURVE('',#11895,#11896,#6849,.T.);
#15198=EDGE_CURVE('',#11895,#11893,#796,.T.);
#15199=EDGE_CURVE('',#11894,#11896,#797,.T.);
#15200=EDGE_CURVE('',#11897,#11898,#6850,.T.);
#15201=EDGE_CURVE('',#11897,#11895,#798,.T.);
#15202=EDGE_CURVE('',#11896,#11898,#799,.T.);
#15203=EDGE_CURVE('',#11899,#11900,#6851,.T.);
#15204=EDGE_CURVE('',#11899,#11897,#800,.T.);
#15205=EDGE_CURVE('',#11898,#11900,#801,.T.);
#15206=EDGE_CURVE('',#11901,#11902,#6852,.T.);
#15207=EDGE_CURVE('',#11901,#11899,#802,.T.);
#15208=EDGE_CURVE('',#11900,#11902,#803,.T.);
#15209=EDGE_CURVE('',#11903,#11904,#6853,.T.);
#15210=EDGE_CURVE('',#11903,#11901,#804,.T.);
#15211=EDGE_CURVE('',#11902,#11904,#805,.T.);
#15212=EDGE_CURVE('',#11905,#11906,#6854,.T.);
#15213=EDGE_CURVE('',#11905,#11903,#806,.T.);
#15214=EDGE_CURVE('',#11904,#11906,#807,.T.);
#15215=EDGE_CURVE('',#11907,#11908,#6855,.T.);
#15216=EDGE_CURVE('',#11907,#11905,#808,.T.);
#15217=EDGE_CURVE('',#11906,#11908,#809,.T.);
#15218=EDGE_CURVE('',#11909,#11910,#6856,.T.);
#15219=EDGE_CURVE('',#11909,#11907,#810,.T.);
#15220=EDGE_CURVE('',#11908,#11910,#811,.T.);
#15221=EDGE_CURVE('',#11911,#11912,#6857,.T.);
#15222=EDGE_CURVE('',#11911,#11909,#812,.T.);
#15223=EDGE_CURVE('',#11910,#11912,#813,.T.);
#15224=EDGE_CURVE('',#11913,#11914,#6858,.T.);
#15225=EDGE_CURVE('',#11913,#11915,#814,.T.);
#15226=EDGE_CURVE('',#11916,#11915,#9919,.T.);
#15227=EDGE_CURVE('',#11914,#11916,#815,.T.);
#15228=EDGE_CURVE('',#11917,#11918,#6859,.T.);
#15229=EDGE_CURVE('',#11917,#11913,#816,.T.);
#15230=EDGE_CURVE('',#11918,#11914,#817,.T.);
#15231=EDGE_CURVE('',#11919,#11920,#6860,.T.);
#15232=EDGE_CURVE('',#11919,#11917,#818,.T.);
#15233=EDGE_CURVE('',#11920,#11918,#819,.T.);
#15234=EDGE_CURVE('',#11921,#11922,#6861,.T.);
#15235=EDGE_CURVE('',#11921,#11919,#820,.T.);
#15236=EDGE_CURVE('',#11922,#11920,#821,.T.);
#15237=EDGE_CURVE('',#11923,#11924,#6862,.T.);
#15238=EDGE_CURVE('',#11923,#11921,#822,.T.);
#15239=EDGE_CURVE('',#11924,#11922,#823,.T.);
#15240=EDGE_CURVE('',#11925,#11926,#6863,.T.);
#15241=EDGE_CURVE('',#11925,#11923,#824,.T.);
#15242=EDGE_CURVE('',#11926,#11924,#825,.T.);
#15243=EDGE_CURVE('',#11927,#11928,#6864,.T.);
#15244=EDGE_CURVE('',#11927,#11925,#826,.T.);
#15245=EDGE_CURVE('',#11928,#11926,#827,.T.);
#15246=EDGE_CURVE('',#11929,#11930,#6865,.T.);
#15247=EDGE_CURVE('',#11929,#11927,#828,.T.);
#15248=EDGE_CURVE('',#11930,#11928,#829,.T.);
#15249=EDGE_CURVE('',#11931,#11932,#6866,.T.);
#15250=EDGE_CURVE('',#11931,#11929,#830,.T.);
#15251=EDGE_CURVE('',#11932,#11930,#831,.T.);
#15252=EDGE_CURVE('',#11933,#11934,#6867,.T.);
#15253=EDGE_CURVE('',#11933,#11931,#832,.T.);
#15254=EDGE_CURVE('',#11934,#11932,#833,.T.);
#15255=EDGE_CURVE('',#11935,#11936,#6868,.T.);
#15256=EDGE_CURVE('',#11935,#11933,#834,.T.);
#15257=EDGE_CURVE('',#11936,#11934,#835,.T.);
#15258=EDGE_CURVE('',#11937,#11938,#6869,.T.);
#15259=EDGE_CURVE('',#11939,#11937,#9920,.T.);
#15260=EDGE_CURVE('',#11939,#11935,#836,.T.);
#15261=EDGE_CURVE('',#11938,#11936,#837,.T.);
#15262=EDGE_CURVE('',#11915,#11940,#838,.T.);
#15263=EDGE_CURVE('',#11941,#11940,#9921,.T.);
#15264=EDGE_CURVE('',#11942,#11941,#9922,.T.);
#15265=EDGE_CURVE('',#11942,#11916,#839,.T.);
#15266=EDGE_CURVE('',#11912,#11942,#840,.T.);
#15267=EDGE_CURVE('',#11943,#11890,#841,.T.);
#15268=EDGE_CURVE('',#11943,#11938,#842,.T.);
#15269=EDGE_CURVE('',#11887,#11939,#843,.T.);
#15270=EDGE_CURVE('',#11937,#11943,#9923,.T.);
#15271=EDGE_CURVE('',#11940,#11911,#844,.T.);
#15272=EDGE_CURVE('',#11940,#11942,#9924,.T.);
#15273=EDGE_CURVE('',#11944,#11945,#9925,.T.);
#15274=EDGE_CURVE('',#11944,#11946,#6870,.T.);
#15275=EDGE_CURVE('',#11946,#11945,#6871,.T.);
#15276=EDGE_CURVE('',#11945,#11947,#6872,.T.);
#15277=EDGE_CURVE('',#11946,#11948,#6873,.T.);
#15278=EDGE_CURVE('',#11947,#11948,#395,.T.);
#15279=EDGE_CURVE('',#11949,#11944,#6874,.T.);
#15280=EDGE_CURVE('',#11948,#11949,#396,.T.);
#15281=EDGE_CURVE('',#11950,#11951,#9926,.T.);
#15282=EDGE_CURVE('',#11950,#11952,#6875,.T.);
#15283=EDGE_CURVE('',#11952,#11951,#6876,.T.);
#15284=EDGE_CURVE('',#11951,#11953,#6877,.T.);
#15285=EDGE_CURVE('',#11952,#11954,#6878,.T.);
#15286=EDGE_CURVE('',#11953,#11954,#397,.T.);
#15287=EDGE_CURVE('',#11955,#11950,#6879,.T.);
#15288=EDGE_CURVE('',#11954,#11955,#398,.T.);
#15289=EDGE_CURVE('',#11956,#11957,#9927,.T.);
#15290=EDGE_CURVE('',#11956,#11958,#6880,.T.);
#15291=EDGE_CURVE('',#11958,#11957,#6881,.T.);
#15292=EDGE_CURVE('',#11957,#11959,#6882,.T.);
#15293=EDGE_CURVE('',#11958,#11960,#6883,.T.);
#15294=EDGE_CURVE('',#11959,#11960,#399,.T.);
#15295=EDGE_CURVE('',#11961,#11956,#6884,.T.);
#15296=EDGE_CURVE('',#11960,#11961,#400,.T.);
#15297=EDGE_CURVE('',#11962,#11963,#9928,.T.);
#15298=EDGE_CURVE('',#11962,#11964,#6885,.T.);
#15299=EDGE_CURVE('',#11964,#11963,#6886,.T.);
#15300=EDGE_CURVE('',#11963,#11965,#6887,.T.);
#15301=EDGE_CURVE('',#11964,#11966,#6888,.T.);
#15302=EDGE_CURVE('',#11965,#11966,#401,.T.);
#15303=EDGE_CURVE('',#11967,#11962,#6889,.T.);
#15304=EDGE_CURVE('',#11966,#11967,#402,.T.);
#15305=EDGE_CURVE('',#11968,#11969,#9929,.T.);
#15306=EDGE_CURVE('',#11968,#11970,#6890,.T.);
#15307=EDGE_CURVE('',#11970,#11969,#6891,.T.);
#15308=EDGE_CURVE('',#11969,#11971,#6892,.T.);
#15309=EDGE_CURVE('',#11970,#11972,#6893,.T.);
#15310=EDGE_CURVE('',#11971,#11972,#403,.T.);
#15311=EDGE_CURVE('',#11973,#11968,#6894,.T.);
#15312=EDGE_CURVE('',#11972,#11973,#404,.T.);
#15313=EDGE_CURVE('',#11974,#11975,#9930,.T.);
#15314=EDGE_CURVE('',#11974,#11976,#6895,.T.);
#15315=EDGE_CURVE('',#11976,#11975,#6896,.T.);
#15316=EDGE_CURVE('',#11975,#11977,#6897,.T.);
#15317=EDGE_CURVE('',#11976,#11978,#6898,.T.);
#15318=EDGE_CURVE('',#11977,#11978,#405,.T.);
#15319=EDGE_CURVE('',#11979,#11974,#6899,.T.);
#15320=EDGE_CURVE('',#11978,#11979,#406,.T.);
#15321=EDGE_CURVE('',#11980,#11981,#9931,.T.);
#15322=EDGE_CURVE('',#11980,#11982,#6900,.T.);
#15323=EDGE_CURVE('',#11982,#11981,#6901,.T.);
#15324=EDGE_CURVE('',#11981,#11983,#6902,.T.);
#15325=EDGE_CURVE('',#11982,#11984,#6903,.T.);
#15326=EDGE_CURVE('',#11983,#11984,#407,.T.);
#15327=EDGE_CURVE('',#11985,#11980,#6904,.T.);
#15328=EDGE_CURVE('',#11984,#11985,#408,.T.);
#15329=EDGE_CURVE('',#11986,#11987,#9932,.T.);
#15330=EDGE_CURVE('',#11986,#11988,#6905,.T.);
#15331=EDGE_CURVE('',#11988,#11987,#6906,.T.);
#15332=EDGE_CURVE('',#11987,#11989,#6907,.T.);
#15333=EDGE_CURVE('',#11988,#11990,#6908,.T.);
#15334=EDGE_CURVE('',#11989,#11990,#409,.T.);
#15335=EDGE_CURVE('',#11991,#11986,#6909,.T.);
#15336=EDGE_CURVE('',#11990,#11991,#410,.T.);
#15337=EDGE_CURVE('',#11992,#11993,#9933,.T.);
#15338=EDGE_CURVE('',#11992,#11994,#6910,.T.);
#15339=EDGE_CURVE('',#11994,#11993,#6911,.T.);
#15340=EDGE_CURVE('',#11993,#11995,#6912,.T.);
#15341=EDGE_CURVE('',#11994,#11996,#6913,.T.);
#15342=EDGE_CURVE('',#11995,#11996,#411,.T.);
#15343=EDGE_CURVE('',#11997,#11992,#6914,.T.);
#15344=EDGE_CURVE('',#11996,#11997,#412,.T.);
#15345=EDGE_CURVE('',#11998,#11999,#9934,.T.);
#15346=EDGE_CURVE('',#11998,#12000,#6915,.T.);
#15347=EDGE_CURVE('',#12000,#11999,#6916,.T.);
#15348=EDGE_CURVE('',#11999,#12001,#6917,.T.);
#15349=EDGE_CURVE('',#12000,#12002,#6918,.T.);
#15350=EDGE_CURVE('',#12001,#12002,#413,.T.);
#15351=EDGE_CURVE('',#12003,#11998,#6919,.T.);
#15352=EDGE_CURVE('',#12002,#12003,#414,.T.);
#15353=EDGE_CURVE('',#12004,#12005,#9935,.T.);
#15354=EDGE_CURVE('',#12004,#12006,#6920,.T.);
#15355=EDGE_CURVE('',#12006,#12005,#6921,.T.);
#15356=EDGE_CURVE('',#12005,#12007,#6922,.T.);
#15357=EDGE_CURVE('',#12006,#12008,#6923,.T.);
#15358=EDGE_CURVE('',#12007,#12008,#415,.T.);
#15359=EDGE_CURVE('',#12009,#12004,#6924,.T.);
#15360=EDGE_CURVE('',#12008,#12009,#416,.T.);
#15361=EDGE_CURVE('',#12010,#12011,#9936,.T.);
#15362=EDGE_CURVE('',#12010,#12012,#6925,.T.);
#15363=EDGE_CURVE('',#12012,#12011,#6926,.T.);
#15364=EDGE_CURVE('',#12011,#12013,#6927,.T.);
#15365=EDGE_CURVE('',#12012,#12014,#6928,.T.);
#15366=EDGE_CURVE('',#12013,#12014,#417,.T.);
#15367=EDGE_CURVE('',#12015,#12010,#6929,.T.);
#15368=EDGE_CURVE('',#12014,#12015,#418,.T.);
#15369=EDGE_CURVE('',#12016,#12017,#9937,.T.);
#15370=EDGE_CURVE('',#12016,#12018,#6930,.T.);
#15371=EDGE_CURVE('',#12018,#12017,#6931,.T.);
#15372=EDGE_CURVE('',#12017,#12019,#6932,.T.);
#15373=EDGE_CURVE('',#12018,#12020,#6933,.T.);
#15374=EDGE_CURVE('',#12019,#12020,#419,.T.);
#15375=EDGE_CURVE('',#12021,#12016,#6934,.T.);
#15376=EDGE_CURVE('',#12020,#12021,#420,.T.);
#15377=EDGE_CURVE('',#12022,#12023,#9938,.T.);
#15378=EDGE_CURVE('',#12022,#12024,#6935,.T.);
#15379=EDGE_CURVE('',#12024,#12023,#6936,.T.);
#15380=EDGE_CURVE('',#12023,#12025,#6937,.T.);
#15381=EDGE_CURVE('',#12024,#12026,#6938,.T.);
#15382=EDGE_CURVE('',#12025,#12026,#421,.T.);
#15383=EDGE_CURVE('',#12027,#12022,#6939,.T.);
#15384=EDGE_CURVE('',#12026,#12027,#422,.T.);
#15385=EDGE_CURVE('',#12028,#12029,#9939,.T.);
#15386=EDGE_CURVE('',#12028,#12030,#6940,.T.);
#15387=EDGE_CURVE('',#12030,#12029,#6941,.T.);
#15388=EDGE_CURVE('',#12029,#12031,#6942,.T.);
#15389=EDGE_CURVE('',#12030,#12032,#6943,.T.);
#15390=EDGE_CURVE('',#12031,#12032,#423,.T.);
#15391=EDGE_CURVE('',#12033,#12028,#6944,.T.);
#15392=EDGE_CURVE('',#12032,#12033,#424,.T.);
#15393=EDGE_CURVE('',#12034,#12035,#9940,.T.);
#15394=EDGE_CURVE('',#12034,#12036,#6945,.T.);
#15395=EDGE_CURVE('',#12036,#12035,#6946,.T.);
#15396=EDGE_CURVE('',#12035,#12037,#6947,.T.);
#15397=EDGE_CURVE('',#12036,#12038,#6948,.T.);
#15398=EDGE_CURVE('',#12037,#12038,#425,.T.);
#15399=EDGE_CURVE('',#12039,#12034,#6949,.T.);
#15400=EDGE_CURVE('',#12038,#12039,#426,.T.);
#15401=EDGE_CURVE('',#12040,#12041,#9941,.T.);
#15402=EDGE_CURVE('',#12040,#12042,#6950,.T.);
#15403=EDGE_CURVE('',#12042,#12041,#6951,.T.);
#15404=EDGE_CURVE('',#12041,#12043,#6952,.T.);
#15405=EDGE_CURVE('',#12042,#12044,#6953,.T.);
#15406=EDGE_CURVE('',#12043,#12044,#427,.T.);
#15407=EDGE_CURVE('',#12045,#12040,#6954,.T.);
#15408=EDGE_CURVE('',#12044,#12045,#428,.T.);
#15409=EDGE_CURVE('',#12046,#12047,#9942,.T.);
#15410=EDGE_CURVE('',#12046,#12048,#6955,.T.);
#15411=EDGE_CURVE('',#12048,#12049,#6956,.T.);
#15412=EDGE_CURVE('',#12047,#12049,#9943,.T.);
#15413=EDGE_CURVE('',#12049,#12050,#6957,.T.);
#15414=EDGE_CURVE('',#12048,#12051,#6958,.T.);
#15415=EDGE_CURVE('',#12050,#12051,#429,.T.);
#15416=EDGE_CURVE('',#12052,#12046,#6959,.T.);
#15417=EDGE_CURVE('',#12051,#12052,#430,.T.);
#15418=EDGE_CURVE('',#12053,#12054,#9944,.T.);
#15419=EDGE_CURVE('',#12053,#12055,#6960,.T.);
#15420=EDGE_CURVE('',#12055,#12054,#6961,.T.);
#15421=EDGE_CURVE('',#12054,#12056,#6962,.T.);
#15422=EDGE_CURVE('',#12055,#12057,#6963,.T.);
#15423=EDGE_CURVE('',#12056,#12057,#431,.T.);
#15424=EDGE_CURVE('',#12058,#12053,#6964,.T.);
#15425=EDGE_CURVE('',#12057,#12058,#432,.T.);
#15426=EDGE_CURVE('',#12059,#12060,#9945,.T.);
#15427=EDGE_CURVE('',#12059,#12061,#6965,.T.);
#15428=EDGE_CURVE('',#12061,#12060,#6966,.T.);
#15429=EDGE_CURVE('',#12060,#12062,#6967,.T.);
#15430=EDGE_CURVE('',#12061,#12063,#6968,.T.);
#15431=EDGE_CURVE('',#12062,#12063,#433,.T.);
#15432=EDGE_CURVE('',#12064,#12059,#6969,.T.);
#15433=EDGE_CURVE('',#12063,#12064,#434,.T.);
#15434=EDGE_CURVE('',#12065,#12066,#9946,.T.);
#15435=EDGE_CURVE('',#12065,#12067,#6970,.T.);
#15436=EDGE_CURVE('',#12067,#12066,#6971,.T.);
#15437=EDGE_CURVE('',#12066,#12068,#6972,.T.);
#15438=EDGE_CURVE('',#12067,#12069,#6973,.T.);
#15439=EDGE_CURVE('',#12068,#12069,#435,.T.);
#15440=EDGE_CURVE('',#12070,#12065,#6974,.T.);
#15441=EDGE_CURVE('',#12069,#12070,#436,.T.);
#15442=EDGE_CURVE('',#12071,#12072,#9947,.T.);
#15443=EDGE_CURVE('',#12071,#12073,#6975,.T.);
#15444=EDGE_CURVE('',#12073,#12072,#6976,.T.);
#15445=EDGE_CURVE('',#12072,#12074,#6977,.T.);
#15446=EDGE_CURVE('',#12073,#12075,#6978,.T.);
#15447=EDGE_CURVE('',#12074,#12075,#437,.T.);
#15448=EDGE_CURVE('',#12076,#12071,#6979,.T.);
#15449=EDGE_CURVE('',#12075,#12076,#438,.T.);
#15450=EDGE_CURVE('',#12077,#12078,#9948,.T.);
#15451=EDGE_CURVE('',#12077,#12079,#6980,.T.);
#15452=EDGE_CURVE('',#12079,#12078,#6981,.T.);
#15453=EDGE_CURVE('',#12078,#12080,#6982,.T.);
#15454=EDGE_CURVE('',#12079,#12081,#6983,.T.);
#15455=EDGE_CURVE('',#12080,#12081,#439,.T.);
#15456=EDGE_CURVE('',#12082,#12077,#6984,.T.);
#15457=EDGE_CURVE('',#12081,#12082,#440,.T.);
#15458=EDGE_CURVE('',#12083,#12084,#9949,.T.);
#15459=EDGE_CURVE('',#12083,#12085,#6985,.T.);
#15460=EDGE_CURVE('',#12085,#12084,#6986,.T.);
#15461=EDGE_CURVE('',#12084,#12086,#6987,.T.);
#15462=EDGE_CURVE('',#12085,#12087,#6988,.T.);
#15463=EDGE_CURVE('',#12086,#12087,#441,.T.);
#15464=EDGE_CURVE('',#12088,#12083,#6989,.T.);
#15465=EDGE_CURVE('',#12087,#12088,#442,.T.);
#15466=EDGE_CURVE('',#12089,#12090,#9950,.T.);
#15467=EDGE_CURVE('',#12089,#12091,#6990,.T.);
#15468=EDGE_CURVE('',#12091,#12090,#6991,.T.);
#15469=EDGE_CURVE('',#12090,#12092,#6992,.T.);
#15470=EDGE_CURVE('',#12091,#12093,#6993,.T.);
#15471=EDGE_CURVE('',#12092,#12093,#443,.T.);
#15472=EDGE_CURVE('',#12094,#12089,#6994,.T.);
#15473=EDGE_CURVE('',#12093,#12094,#444,.T.);
#15474=EDGE_CURVE('',#12095,#12096,#9951,.T.);
#15475=EDGE_CURVE('',#12095,#12097,#6995,.T.);
#15476=EDGE_CURVE('',#12097,#12096,#6996,.T.);
#15477=EDGE_CURVE('',#12096,#12098,#6997,.T.);
#15478=EDGE_CURVE('',#12097,#12099,#6998,.T.);
#15479=EDGE_CURVE('',#12098,#12099,#445,.T.);
#15480=EDGE_CURVE('',#12100,#12095,#6999,.T.);
#15481=EDGE_CURVE('',#12099,#12100,#446,.T.);
#15482=EDGE_CURVE('',#12101,#12102,#9952,.T.);
#15483=EDGE_CURVE('',#12101,#12103,#7000,.T.);
#15484=EDGE_CURVE('',#12103,#12102,#7001,.T.);
#15485=EDGE_CURVE('',#12102,#12104,#7002,.T.);
#15486=EDGE_CURVE('',#12103,#12105,#7003,.T.);
#15487=EDGE_CURVE('',#12104,#12105,#447,.T.);
#15488=EDGE_CURVE('',#12106,#12101,#7004,.T.);
#15489=EDGE_CURVE('',#12105,#12106,#448,.T.);
#15490=EDGE_CURVE('',#12107,#12108,#9953,.T.);
#15491=EDGE_CURVE('',#12107,#12109,#7005,.T.);
#15492=EDGE_CURVE('',#12109,#12108,#7006,.T.);
#15493=EDGE_CURVE('',#12108,#12110,#7007,.T.);
#15494=EDGE_CURVE('',#12109,#12111,#7008,.T.);
#15495=EDGE_CURVE('',#12110,#12111,#449,.T.);
#15496=EDGE_CURVE('',#12112,#12107,#7009,.T.);
#15497=EDGE_CURVE('',#12111,#12112,#450,.T.);
#15498=EDGE_CURVE('',#12113,#12114,#9954,.T.);
#15499=EDGE_CURVE('',#12113,#12115,#7010,.T.);
#15500=EDGE_CURVE('',#12115,#12114,#7011,.T.);
#15501=EDGE_CURVE('',#12114,#12116,#7012,.T.);
#15502=EDGE_CURVE('',#12115,#12117,#7013,.T.);
#15503=EDGE_CURVE('',#12116,#12117,#451,.T.);
#15504=EDGE_CURVE('',#12118,#12113,#7014,.T.);
#15505=EDGE_CURVE('',#12117,#12118,#452,.T.);
#15506=EDGE_CURVE('',#12119,#12120,#9955,.T.);
#15507=EDGE_CURVE('',#12119,#12121,#7015,.T.);
#15508=EDGE_CURVE('',#12121,#12120,#7016,.T.);
#15509=EDGE_CURVE('',#12120,#12122,#7017,.T.);
#15510=EDGE_CURVE('',#12121,#12123,#7018,.T.);
#15511=EDGE_CURVE('',#12122,#12123,#453,.T.);
#15512=EDGE_CURVE('',#12124,#12119,#7019,.T.);
#15513=EDGE_CURVE('',#12123,#12124,#454,.T.);
#15514=EDGE_CURVE('',#12125,#12126,#9956,.T.);
#15515=EDGE_CURVE('',#12125,#12127,#7020,.T.);
#15516=EDGE_CURVE('',#12127,#12126,#7021,.T.);
#15517=EDGE_CURVE('',#12126,#12128,#7022,.T.);
#15518=EDGE_CURVE('',#12127,#12129,#7023,.T.);
#15519=EDGE_CURVE('',#12128,#12129,#455,.T.);
#15520=EDGE_CURVE('',#12130,#12125,#7024,.T.);
#15521=EDGE_CURVE('',#12129,#12130,#456,.T.);
#15522=EDGE_CURVE('',#12131,#12132,#9957,.T.);
#15523=EDGE_CURVE('',#12131,#12133,#7025,.T.);
#15524=EDGE_CURVE('',#12133,#12132,#7026,.T.);
#15525=EDGE_CURVE('',#12132,#12134,#7027,.T.);
#15526=EDGE_CURVE('',#12133,#12135,#7028,.T.);
#15527=EDGE_CURVE('',#12134,#12135,#457,.T.);
#15528=EDGE_CURVE('',#12136,#12131,#7029,.T.);
#15529=EDGE_CURVE('',#12135,#12136,#458,.T.);
#15530=EDGE_CURVE('',#12137,#12138,#9958,.T.);
#15531=EDGE_CURVE('',#12137,#12139,#7030,.T.);
#15532=EDGE_CURVE('',#12139,#12138,#7031,.T.);
#15533=EDGE_CURVE('',#12138,#12140,#7032,.T.);
#15534=EDGE_CURVE('',#12139,#12141,#7033,.T.);
#15535=EDGE_CURVE('',#12140,#12141,#459,.T.);
#15536=EDGE_CURVE('',#12142,#12137,#7034,.T.);
#15537=EDGE_CURVE('',#12141,#12142,#460,.T.);
#15538=EDGE_CURVE('',#12143,#12144,#9959,.T.);
#15539=EDGE_CURVE('',#12143,#12145,#7035,.T.);
#15540=EDGE_CURVE('',#12145,#12144,#7036,.T.);
#15541=EDGE_CURVE('',#12144,#12146,#7037,.T.);
#15542=EDGE_CURVE('',#12145,#12147,#7038,.T.);
#15543=EDGE_CURVE('',#12146,#12147,#461,.T.);
#15544=EDGE_CURVE('',#12148,#12143,#7039,.T.);
#15545=EDGE_CURVE('',#12147,#12148,#462,.T.);
#15546=EDGE_CURVE('',#12149,#12150,#9960,.T.);
#15547=EDGE_CURVE('',#12149,#12151,#7040,.T.);
#15548=EDGE_CURVE('',#12151,#12150,#7041,.T.);
#15549=EDGE_CURVE('',#12150,#12152,#7042,.T.);
#15550=EDGE_CURVE('',#12151,#12153,#7043,.T.);
#15551=EDGE_CURVE('',#12152,#12153,#463,.T.);
#15552=EDGE_CURVE('',#12154,#12149,#7044,.T.);
#15553=EDGE_CURVE('',#12153,#12154,#464,.T.);
#15554=EDGE_CURVE('',#11955,#11947,#9961,.T.);
#15555=EDGE_CURVE('',#11961,#11953,#9962,.T.);
#15556=EDGE_CURVE('',#11967,#11959,#9963,.T.);
#15557=EDGE_CURVE('',#11973,#11965,#9964,.T.);
#15558=EDGE_CURVE('',#11979,#11971,#9965,.T.);
#15559=EDGE_CURVE('',#11985,#11977,#9966,.T.);
#15560=EDGE_CURVE('',#11991,#11983,#9967,.T.);
#15561=EDGE_CURVE('',#11997,#11989,#9968,.T.);
#15562=EDGE_CURVE('',#12003,#11995,#9969,.T.);
#15563=EDGE_CURVE('',#12009,#12001,#9970,.T.);
#15564=EDGE_CURVE('',#12015,#12007,#9971,.T.);
#15565=EDGE_CURVE('',#12021,#12013,#9972,.T.);
#15566=EDGE_CURVE('',#12027,#12019,#9973,.T.);
#15567=EDGE_CURVE('',#12033,#12025,#9974,.T.);
#15568=EDGE_CURVE('',#12039,#12031,#9975,.T.);
#15569=EDGE_CURVE('',#12045,#12037,#9976,.T.);
#15570=EDGE_CURVE('',#12052,#12043,#9977,.T.);
#15571=EDGE_CURVE('',#12047,#12155,#7045,.T.);
#15572=EDGE_CURVE('',#12155,#12155,#9978,.T.);
#15573=EDGE_CURVE('',#12058,#12050,#9979,.T.);
#15574=EDGE_CURVE('',#12064,#12056,#9980,.T.);
#15575=EDGE_CURVE('',#12070,#12062,#9981,.T.);
#15576=EDGE_CURVE('',#12076,#12068,#9982,.T.);
#15577=EDGE_CURVE('',#12082,#12074,#9983,.T.);
#15578=EDGE_CURVE('',#12088,#12080,#9984,.T.);
#15579=EDGE_CURVE('',#12094,#12086,#9985,.T.);
#15580=EDGE_CURVE('',#12100,#12092,#9986,.T.);
#15581=EDGE_CURVE('',#12106,#12098,#9987,.T.);
#15582=EDGE_CURVE('',#12112,#12104,#9988,.T.);
#15583=EDGE_CURVE('',#12118,#12110,#9989,.T.);
#15584=EDGE_CURVE('',#12124,#12116,#9990,.T.);
#15585=EDGE_CURVE('',#12130,#12122,#9991,.T.);
#15586=EDGE_CURVE('',#12136,#12128,#9992,.T.);
#15587=EDGE_CURVE('',#12142,#12134,#9993,.T.);
#15588=EDGE_CURVE('',#12148,#12140,#9994,.T.);
#15589=EDGE_CURVE('',#12154,#12146,#9995,.T.);
#15590=EDGE_CURVE('',#12156,#12152,#9996,.T.);
#15591=EDGE_CURVE('',#12156,#12157,#7046,.T.);
#15592=EDGE_CURVE('',#12157,#12158,#9997,.T.);
#15593=EDGE_CURVE('',#12158,#12159,#7047,.T.);
#15594=EDGE_CURVE('',#11949,#12159,#9998,.T.);
#15595=EDGE_CURVE('',#12160,#12158,#7048,.T.);
#15596=EDGE_CURVE('',#12160,#12161,#7049,.T.);
#15597=EDGE_CURVE('',#12159,#12161,#465,.T.);
#15598=EDGE_CURVE('',#12161,#12156,#466,.T.);
#15599=EDGE_CURVE('',#12157,#12160,#7050,.T.);
#15600=EDGE_CURVE('',#12162,#12162,#9999,.T.);
#15601=EDGE_CURVE('',#12162,#12051,#7051,.T.);
#15602=EDGE_CURVE('',#12163,#12164,#7052,.T.);
#15603=EDGE_CURVE('',#12164,#12164,#10000,.T.);
#15604=EDGE_CURVE('',#12165,#12166,#7053,.T.);
#15605=EDGE_CURVE('',#12165,#12167,#7054,.T.);
#15606=EDGE_CURVE('',#12167,#12168,#7055,.T.);
#15607=EDGE_CURVE('',#12166,#12168,#7056,.T.);
#15608=EDGE_CURVE('',#12169,#12165,#7057,.T.);
#15609=EDGE_CURVE('',#12169,#12170,#7058,.T.);
#15610=EDGE_CURVE('',#12170,#12167,#7059,.T.);
#15611=EDGE_CURVE('',#12171,#12169,#7060,.T.);
#15612=EDGE_CURVE('',#12171,#12172,#7061,.T.);
#15613=EDGE_CURVE('',#12172,#12170,#7062,.T.);
#15614=EDGE_CURVE('',#12173,#12171,#7063,.T.);
#15615=EDGE_CURVE('',#12173,#12174,#7064,.T.);
#15616=EDGE_CURVE('',#12174,#12172,#7065,.T.);
#15617=EDGE_CURVE('',#12175,#12173,#7066,.T.);
#15618=EDGE_CURVE('',#12175,#12176,#7067,.T.);
#15619=EDGE_CURVE('',#12176,#12174,#7068,.T.);
#15620=EDGE_CURVE('',#12166,#12175,#7069,.T.);
#15621=EDGE_CURVE('',#12168,#12176,#7070,.T.);
#15622=EDGE_CURVE('',#12177,#12177,#10001,.T.);
#15623=EDGE_CURVE('',#11889,#12177,#7071,.T.);
#15624=EDGE_CURVE('',#12178,#12178,#10002,.T.);
#15625=EDGE_CURVE('',#12178,#11941,#7072,.T.);
#15626=EDGE_CURVE('',#12179,#12180,#7073,.T.);
#15627=EDGE_CURVE('',#12179,#12181,#845,.T.);
#15628=EDGE_CURVE('',#12181,#12182,#10003,.T.);
#15629=EDGE_CURVE('',#12182,#12183,#7074,.T.);
#15630=EDGE_CURVE('',#12183,#12183,#10004,.T.);
#15631=EDGE_CURVE('',#12182,#12184,#10005,.T.);
#15632=EDGE_CURVE('',#12184,#12180,#846,.T.);
#15633=EDGE_CURVE('',#12185,#12186,#7075,.T.);
#15634=EDGE_CURVE('',#12185,#12179,#847,.T.);
#15635=EDGE_CURVE('',#12180,#12186,#848,.T.);
#15636=EDGE_CURVE('',#12187,#12188,#7076,.T.);
#15637=EDGE_CURVE('',#12187,#12185,#849,.T.);
#15638=EDGE_CURVE('',#12186,#12188,#850,.T.);
#15639=EDGE_CURVE('',#12189,#12190,#7077,.T.);
#15640=EDGE_CURVE('',#12189,#12187,#851,.T.);
#15641=EDGE_CURVE('',#12188,#12190,#852,.T.);
#15642=EDGE_CURVE('',#12191,#12192,#7078,.T.);
#15643=EDGE_CURVE('',#12191,#12189,#853,.T.);
#15644=EDGE_CURVE('',#12190,#12192,#854,.T.);
#15645=EDGE_CURVE('',#12193,#12194,#7079,.T.);
#15646=EDGE_CURVE('',#12193,#12191,#855,.T.);
#15647=EDGE_CURVE('',#12192,#12194,#856,.T.);
#15648=EDGE_CURVE('',#12195,#12196,#7080,.T.);
#15649=EDGE_CURVE('',#12195,#12193,#857,.T.);
#15650=EDGE_CURVE('',#12194,#12196,#858,.T.);
#15651=EDGE_CURVE('',#12197,#12198,#7081,.T.);
#15652=EDGE_CURVE('',#12197,#12199,#859,.T.);
#15653=EDGE_CURVE('',#12200,#12199,#10006,.T.);
#15654=EDGE_CURVE('',#12198,#12200,#860,.T.);
#15655=EDGE_CURVE('',#12201,#12202,#7082,.T.);
#15656=EDGE_CURVE('',#12201,#12197,#861,.T.);
#15657=EDGE_CURVE('',#12202,#12198,#862,.T.);
#15658=EDGE_CURVE('',#12203,#12204,#7083,.T.);
#15659=EDGE_CURVE('',#12203,#12201,#863,.T.);
#15660=EDGE_CURVE('',#12204,#12202,#864,.T.);
#15661=EDGE_CURVE('',#12205,#12206,#7084,.T.);
#15662=EDGE_CURVE('',#12205,#12203,#865,.T.);
#15663=EDGE_CURVE('',#12206,#12204,#866,.T.);
#15664=EDGE_CURVE('',#12207,#12208,#7085,.T.);
#15665=EDGE_CURVE('',#12207,#12205,#867,.T.);
#15666=EDGE_CURVE('',#12208,#12206,#868,.T.);
#15667=EDGE_CURVE('',#12209,#12210,#7086,.T.);
#15668=EDGE_CURVE('',#12209,#12207,#869,.T.);
#15669=EDGE_CURVE('',#12210,#12208,#870,.T.);
#15670=EDGE_CURVE('',#12211,#12212,#7087,.T.);
#15671=EDGE_CURVE('',#12211,#12209,#871,.T.);
#15672=EDGE_CURVE('',#12212,#12210,#872,.T.);
#15673=EDGE_CURVE('',#12213,#12214,#7088,.T.);
#15674=EDGE_CURVE('',#12215,#12213,#10007,.T.);
#15675=EDGE_CURVE('',#12215,#12211,#873,.T.);
#15676=EDGE_CURVE('',#12214,#12212,#874,.T.);
#15677=EDGE_CURVE('',#12216,#12200,#875,.T.);
#15678=EDGE_CURVE('',#12196,#12216,#876,.T.);
#15679=EDGE_CURVE('',#12217,#12184,#877,.T.);
#15680=EDGE_CURVE('',#12217,#12214,#878,.T.);
#15681=EDGE_CURVE('',#12181,#12215,#879,.T.);
#15682=EDGE_CURVE('',#12213,#12217,#10008,.T.);
#15683=EDGE_CURVE('',#12199,#12218,#880,.T.);
#15684=EDGE_CURVE('',#12218,#12195,#881,.T.);
#15685=EDGE_CURVE('',#12219,#12220,#7089,.T.);
#15686=EDGE_CURVE('',#12221,#12219,#7090,.T.);
#15687=EDGE_CURVE('',#12222,#12221,#7091,.T.);
#15688=EDGE_CURVE('',#12222,#12220,#7092,.T.);
#15689=EDGE_CURVE('',#12223,#12224,#7093,.T.);
#15690=EDGE_CURVE('',#12225,#12223,#7094,.T.);
#15691=EDGE_CURVE('',#12226,#12225,#7095,.T.);
#15692=EDGE_CURVE('',#12224,#12226,#7096,.T.);
#15693=EDGE_CURVE('',#12227,#12228,#7097,.T.);
#15694=EDGE_CURVE('',#12229,#12227,#7098,.T.);
#15695=EDGE_CURVE('',#12230,#12229,#7099,.T.);
#15696=EDGE_CURVE('',#12230,#12228,#7100,.T.);
#15697=EDGE_CURVE('',#12220,#12231,#7101,.T.);
#15698=EDGE_CURVE('',#12232,#12222,#7102,.T.);
#15699=EDGE_CURVE('',#12231,#12232,#7103,.T.);
#15700=EDGE_CURVE('',#12228,#12223,#7104,.T.);
#15701=EDGE_CURVE('',#12225,#12230,#7105,.T.);
#15702=EDGE_CURVE('',#12233,#12219,#7106,.T.);
#15703=EDGE_CURVE('',#12234,#12233,#7107,.T.);
#15704=EDGE_CURVE('',#12221,#12234,#7108,.T.);
#15705=EDGE_CURVE('',#12235,#12235,#10009,.T.);
#15706=EDGE_CURVE('',#12231,#12236,#7109,.T.);
#15707=EDGE_CURVE('',#12236,#12237,#7110,.T.);
#15708=EDGE_CURVE('',#12237,#12227,#7111,.T.);
#15709=EDGE_CURVE('',#12224,#12238,#7112,.T.);
#15710=EDGE_CURVE('',#12238,#12239,#7113,.T.);
#15711=EDGE_CURVE('',#12239,#12233,#7114,.T.);
#15712=EDGE_CURVE('',#12240,#12232,#7115,.T.);
#15713=EDGE_CURVE('',#12240,#12236,#7116,.T.);
#15714=EDGE_CURVE('',#12241,#12237,#7117,.T.);
#15715=EDGE_CURVE('',#12229,#12241,#7118,.T.);
#15716=EDGE_CURVE('',#12242,#12226,#7119,.T.);
#15717=EDGE_CURVE('',#12242,#12238,#7120,.T.);
#15718=EDGE_CURVE('',#12243,#12239,#7121,.T.);
#15719=EDGE_CURVE('',#12234,#12243,#7122,.T.);
#15720=EDGE_CURVE('',#12241,#12240,#7123,.T.);
#15721=EDGE_CURVE('',#12243,#12242,#7124,.T.);
#15722=EDGE_CURVE('',#12244,#12244,#10010,.T.);
#15723=EDGE_CURVE('',#12183,#12244,#7125,.T.);
#15724=EDGE_CURVE('',#12218,#12216,#10011,.T.);
#15725=EDGE_CURVE('',#12245,#12245,#10012,.T.);
#15726=EDGE_CURVE('',#12246,#12246,#10013,.T.);
#15727=EDGE_CURVE('',#12246,#12245,#7126,.T.);
#15728=EDGE_CURVE('',#12235,#12246,#7127,.T.);
#15729=EDGE_CURVE('',#12247,#12248,#7128,.T.);
#15730=EDGE_CURVE('',#12247,#12249,#882,.T.);
#15731=EDGE_CURVE('',#12249,#12250,#10014,.T.);
#15732=EDGE_CURVE('',#12250,#12251,#7129,.T.);
#15733=EDGE_CURVE('',#12251,#12251,#10015,.T.);
#15734=EDGE_CURVE('',#12250,#12252,#10016,.T.);
#15735=EDGE_CURVE('',#12252,#12248,#883,.T.);
#15736=EDGE_CURVE('',#12253,#12254,#7130,.T.);
#15737=EDGE_CURVE('',#12253,#12247,#884,.T.);
#15738=EDGE_CURVE('',#12248,#12254,#885,.T.);
#15739=EDGE_CURVE('',#12255,#12256,#7131,.T.);
#15740=EDGE_CURVE('',#12255,#12253,#886,.T.);
#15741=EDGE_CURVE('',#12254,#12256,#887,.T.);
#15742=EDGE_CURVE('',#12257,#12258,#7132,.T.);
#15743=EDGE_CURVE('',#12257,#12255,#888,.T.);
#15744=EDGE_CURVE('',#12256,#12258,#889,.T.);
#15745=EDGE_CURVE('',#12259,#12260,#7133,.T.);
#15746=EDGE_CURVE('',#12259,#12257,#890,.T.);
#15747=EDGE_CURVE('',#12258,#12260,#891,.T.);
#15748=EDGE_CURVE('',#12261,#12262,#7134,.T.);
#15749=EDGE_CURVE('',#12261,#12259,#892,.T.);
#15750=EDGE_CURVE('',#12260,#12262,#893,.T.);
#15751=EDGE_CURVE('',#12263,#12264,#7135,.T.);
#15752=EDGE_CURVE('',#12263,#12261,#894,.T.);
#15753=EDGE_CURVE('',#12262,#12264,#895,.T.);
#15754=EDGE_CURVE('',#12265,#12266,#7136,.T.);
#15755=EDGE_CURVE('',#12265,#12263,#896,.T.);
#15756=EDGE_CURVE('',#12264,#12266,#897,.T.);
#15757=EDGE_CURVE('',#12267,#12268,#7137,.T.);
#15758=EDGE_CURVE('',#12267,#12265,#898,.T.);
#15759=EDGE_CURVE('',#12266,#12268,#899,.T.);
#15760=EDGE_CURVE('',#12269,#12270,#7138,.T.);
#15761=EDGE_CURVE('',#12269,#12267,#900,.T.);
#15762=EDGE_CURVE('',#12268,#12270,#901,.T.);
#15763=EDGE_CURVE('',#12271,#12272,#7139,.T.);
#15764=EDGE_CURVE('',#12271,#12269,#902,.T.);
#15765=EDGE_CURVE('',#12270,#12272,#903,.T.);
#15766=EDGE_CURVE('',#12273,#12274,#7140,.T.);
#15767=EDGE_CURVE('',#12273,#12271,#904,.T.);
#15768=EDGE_CURVE('',#12272,#12274,#905,.T.);
#15769=EDGE_CURVE('',#12275,#12276,#7141,.T.);
#15770=EDGE_CURVE('',#12275,#12273,#906,.T.);
#15771=EDGE_CURVE('',#12274,#12276,#907,.T.);
#15772=EDGE_CURVE('',#12277,#12278,#7142,.T.);
#15773=EDGE_CURVE('',#12277,#12275,#908,.T.);
#15774=EDGE_CURVE('',#12276,#12278,#909,.T.);
#15775=EDGE_CURVE('',#12279,#12280,#7143,.T.);
#15776=EDGE_CURVE('',#12279,#12277,#910,.T.);
#15777=EDGE_CURVE('',#12278,#12280,#911,.T.);
#15778=EDGE_CURVE('',#12281,#12282,#7144,.T.);
#15779=EDGE_CURVE('',#12281,#12279,#912,.T.);
#15780=EDGE_CURVE('',#12280,#12282,#913,.T.);
#15781=EDGE_CURVE('',#12283,#12284,#7145,.T.);
#15782=EDGE_CURVE('',#12283,#12285,#914,.T.);
#15783=EDGE_CURVE('',#12284,#12285,#10017,.T.);
#15784=EDGE_CURVE('',#12286,#12287,#7146,.T.);
#15785=EDGE_CURVE('',#12286,#12283,#915,.T.);
#15786=EDGE_CURVE('',#12288,#12284,#10018,.T.);
#15787=EDGE_CURVE('',#12287,#12288,#916,.T.);
#15788=EDGE_CURVE('',#12289,#12290,#7147,.T.);
#15789=EDGE_CURVE('',#12289,#12286,#917,.T.);
#15790=EDGE_CURVE('',#12290,#12287,#918,.T.);
#15791=EDGE_CURVE('',#12291,#12292,#7148,.T.);
#15792=EDGE_CURVE('',#12291,#12289,#919,.T.);
#15793=EDGE_CURVE('',#12292,#12290,#920,.T.);
#15794=EDGE_CURVE('',#12293,#12294,#7149,.T.);
#15795=EDGE_CURVE('',#12293,#12291,#921,.T.);
#15796=EDGE_CURVE('',#12294,#12292,#922,.T.);
#15797=EDGE_CURVE('',#12295,#12296,#7150,.T.);
#15798=EDGE_CURVE('',#12295,#12293,#923,.T.);
#15799=EDGE_CURVE('',#12296,#12294,#924,.T.);
#15800=EDGE_CURVE('',#12297,#12298,#7151,.T.);
#15801=EDGE_CURVE('',#12297,#12295,#925,.T.);
#15802=EDGE_CURVE('',#12298,#12296,#926,.T.);
#15803=EDGE_CURVE('',#12299,#12300,#7152,.T.);
#15804=EDGE_CURVE('',#12299,#12297,#927,.T.);
#15805=EDGE_CURVE('',#12300,#12298,#928,.T.);
#15806=EDGE_CURVE('',#12301,#12302,#7153,.T.);
#15807=EDGE_CURVE('',#12301,#12299,#929,.T.);
#15808=EDGE_CURVE('',#12302,#12300,#930,.T.);
#15809=EDGE_CURVE('',#12303,#12304,#7154,.T.);
#15810=EDGE_CURVE('',#12303,#12301,#931,.T.);
#15811=EDGE_CURVE('',#12304,#12302,#932,.T.);
#15812=EDGE_CURVE('',#12305,#12306,#7155,.T.);
#15813=EDGE_CURVE('',#12305,#12303,#933,.T.);
#15814=EDGE_CURVE('',#12306,#12304,#934,.T.);
#15815=EDGE_CURVE('',#12307,#12308,#7156,.T.);
#15816=EDGE_CURVE('',#12307,#12305,#935,.T.);
#15817=EDGE_CURVE('',#12308,#12306,#936,.T.);
#15818=EDGE_CURVE('',#12309,#12310,#7157,.T.);
#15819=EDGE_CURVE('',#12309,#12307,#937,.T.);
#15820=EDGE_CURVE('',#12310,#12308,#938,.T.);
#15821=EDGE_CURVE('',#12311,#12312,#7158,.T.);
#15822=EDGE_CURVE('',#12311,#12309,#939,.T.);
#15823=EDGE_CURVE('',#12312,#12310,#940,.T.);
#15824=EDGE_CURVE('',#12313,#12314,#7159,.T.);
#15825=EDGE_CURVE('',#12313,#12311,#941,.T.);
#15826=EDGE_CURVE('',#12314,#12312,#942,.T.);
#15827=EDGE_CURVE('',#12315,#12316,#7160,.T.);
#15828=EDGE_CURVE('',#12315,#12313,#943,.T.);
#15829=EDGE_CURVE('',#12316,#12314,#944,.T.);
#15830=EDGE_CURVE('',#12317,#12318,#7161,.T.);
#15831=EDGE_CURVE('',#12319,#12317,#10019,.T.);
#15832=EDGE_CURVE('',#12319,#12315,#945,.T.);
#15833=EDGE_CURVE('',#12318,#12316,#946,.T.);
#15834=EDGE_CURVE('',#12320,#12288,#947,.T.);
#15835=EDGE_CURVE('',#12282,#12320,#948,.T.);
#15836=EDGE_CURVE('',#12321,#12252,#949,.T.);
#15837=EDGE_CURVE('',#12321,#12318,#950,.T.);
#15838=EDGE_CURVE('',#12249,#12319,#951,.T.);
#15839=EDGE_CURVE('',#12317,#12321,#10020,.T.);
#15840=EDGE_CURVE('',#12285,#12322,#952,.T.);
#15841=EDGE_CURVE('',#12322,#12281,#953,.T.);
#15842=EDGE_CURVE('',#12322,#12320,#10021,.T.);
#15843=EDGE_CURVE('',#12323,#12324,#7162,.T.);
#15844=EDGE_CURVE('',#12325,#12323,#7163,.T.);
#15845=EDGE_CURVE('',#12326,#12325,#7164,.T.);
#15846=EDGE_CURVE('',#12326,#12324,#7165,.T.);
#15847=EDGE_CURVE('',#12327,#12328,#7166,.T.);
#15848=EDGE_CURVE('',#12329,#12327,#7167,.T.);
#15849=EDGE_CURVE('',#12330,#12329,#7168,.T.);
#15850=EDGE_CURVE('',#12328,#12330,#7169,.T.);
#15851=EDGE_CURVE('',#12331,#12332,#7170,.T.);
#15852=EDGE_CURVE('',#12333,#12331,#7171,.T.);
#15853=EDGE_CURVE('',#12334,#12333,#7172,.T.);
#15854=EDGE_CURVE('',#12334,#12332,#7173,.T.);
#15855=EDGE_CURVE('',#12324,#12335,#7174,.T.);
#15856=EDGE_CURVE('',#12336,#12326,#7175,.T.);
#15857=EDGE_CURVE('',#12335,#12336,#7176,.T.);
#15858=EDGE_CURVE('',#12332,#12327,#7177,.T.);
#15859=EDGE_CURVE('',#12329,#12334,#7178,.T.);
#15860=EDGE_CURVE('',#12337,#12323,#7179,.T.);
#15861=EDGE_CURVE('',#12338,#12337,#7180,.T.);
#15862=EDGE_CURVE('',#12325,#12338,#7181,.T.);
#15863=EDGE_CURVE('',#12339,#12339,#10022,.T.);
#15864=EDGE_CURVE('',#12335,#12340,#7182,.T.);
#15865=EDGE_CURVE('',#12340,#12341,#7183,.T.);
#15866=EDGE_CURVE('',#12341,#12331,#7184,.T.);
#15867=EDGE_CURVE('',#12328,#12342,#7185,.T.);
#15868=EDGE_CURVE('',#12342,#12343,#7186,.T.);
#15869=EDGE_CURVE('',#12343,#12337,#7187,.T.);
#15870=EDGE_CURVE('',#12344,#12336,#7188,.T.);
#15871=EDGE_CURVE('',#12344,#12340,#7189,.T.);
#15872=EDGE_CURVE('',#12345,#12341,#7190,.T.);
#15873=EDGE_CURVE('',#12333,#12345,#7191,.T.);
#15874=EDGE_CURVE('',#12346,#12330,#7192,.T.);
#15875=EDGE_CURVE('',#12346,#12342,#7193,.T.);
#15876=EDGE_CURVE('',#12347,#12343,#7194,.T.);
#15877=EDGE_CURVE('',#12338,#12347,#7195,.T.);
#15878=EDGE_CURVE('',#12345,#12344,#7196,.T.);
#15879=EDGE_CURVE('',#12347,#12346,#7197,.T.);
#15880=EDGE_CURVE('',#12348,#12348,#10023,.T.);
#15881=EDGE_CURVE('',#12251,#12348,#7198,.T.);
#15882=EDGE_CURVE('',#12349,#12349,#10024,.T.);
#15883=EDGE_CURVE('',#12350,#12350,#10025,.T.);
#15884=EDGE_CURVE('',#12350,#12349,#7199,.T.);
#15885=EDGE_CURVE('',#12339,#12350,#7200,.T.);
#15886=ORIENTED_EDGE('',*,*,#12351,.T.);
#15887=ORIENTED_EDGE('',*,*,#12352,.T.);
#15888=ORIENTED_EDGE('',*,*,#12353,.T.);
#15889=ORIENTED_EDGE('',*,*,#12354,.T.);
#15890=ORIENTED_EDGE('',*,*,#12352,.F.);
#15891=ORIENTED_EDGE('',*,*,#12351,.F.);
#15892=ORIENTED_EDGE('',*,*,#12355,.T.);
#15893=ORIENTED_EDGE('',*,*,#12356,.F.);
#15894=ORIENTED_EDGE('',*,*,#12355,.F.);
#15895=ORIENTED_EDGE('',*,*,#12357,.F.);
#15896=ORIENTED_EDGE('',*,*,#12358,.T.);
#15897=ORIENTED_EDGE('',*,*,#12353,.F.);
#15898=ORIENTED_EDGE('',*,*,#12354,.F.);
#15899=ORIENTED_EDGE('',*,*,#12358,.F.);
#15900=ORIENTED_EDGE('',*,*,#12359,.T.);
#15901=ORIENTED_EDGE('',*,*,#12360,.T.);
#15902=ORIENTED_EDGE('',*,*,#12361,.T.);
#15903=ORIENTED_EDGE('',*,*,#12360,.F.);
#15904=ORIENTED_EDGE('',*,*,#12359,.F.);
#15905=ORIENTED_EDGE('',*,*,#12362,.T.);
#15906=ORIENTED_EDGE('',*,*,#12363,.F.);
#15907=ORIENTED_EDGE('',*,*,#12362,.F.);
#15908=ORIENTED_EDGE('',*,*,#12361,.F.);
#15909=ORIENTED_EDGE('',*,*,#12364,.F.);
#15910=ORIENTED_EDGE('',*,*,#12365,.T.);
#15911=ORIENTED_EDGE('',*,*,#12366,.T.);
#15912=ORIENTED_EDGE('',*,*,#12367,.T.);
#15913=ORIENTED_EDGE('',*,*,#12368,.T.);
#15914=ORIENTED_EDGE('',*,*,#12369,.T.);
#15915=ORIENTED_EDGE('',*,*,#12370,.T.);
#15916=ORIENTED_EDGE('',*,*,#12356,.T.);
#15917=ORIENTED_EDGE('',*,*,#12371,.T.);
#15918=ORIENTED_EDGE('',*,*,#12372,.T.);
#15919=ORIENTED_EDGE('',*,*,#12371,.F.);
#15920=ORIENTED_EDGE('',*,*,#12372,.F.);
#15921=ORIENTED_EDGE('',*,*,#12373,.F.);
#15922=ORIENTED_EDGE('',*,*,#12374,.F.);
#15923=ORIENTED_EDGE('',*,*,#12375,.F.);
#15924=ORIENTED_EDGE('',*,*,#12376,.F.);
#15925=ORIENTED_EDGE('',*,*,#12377,.F.);
#15926=ORIENTED_EDGE('',*,*,#12378,.F.);
#15927=ORIENTED_EDGE('',*,*,#12379,.F.);
#15928=ORIENTED_EDGE('',*,*,#12380,.T.);
#15929=ORIENTED_EDGE('',*,*,#12381,.T.);
#15930=ORIENTED_EDGE('',*,*,#12373,.T.);
#15931=ORIENTED_EDGE('',*,*,#12381,.F.);
#15932=ORIENTED_EDGE('',*,*,#12380,.F.);
#15933=ORIENTED_EDGE('',*,*,#12382,.T.);
#15934=ORIENTED_EDGE('',*,*,#12383,.F.);
#15935=ORIENTED_EDGE('',*,*,#12382,.F.);
#15936=ORIENTED_EDGE('',*,*,#12383,.T.);
#15937=ORIENTED_EDGE('',*,*,#12384,.T.);
#15938=ORIENTED_EDGE('',*,*,#12385,.T.);
#15939=ORIENTED_EDGE('',*,*,#12386,.T.);
#15940=ORIENTED_EDGE('',*,*,#12384,.F.);
#15941=ORIENTED_EDGE('',*,*,#12387,.F.);
#15942=ORIENTED_EDGE('',*,*,#12388,.F.);
#15943=ORIENTED_EDGE('',*,*,#12389,.T.);
#15944=ORIENTED_EDGE('',*,*,#12385,.F.);
#15945=ORIENTED_EDGE('',*,*,#12386,.F.);
#15946=ORIENTED_EDGE('',*,*,#12389,.F.);
#15947=ORIENTED_EDGE('',*,*,#12390,.T.);
#15948=ORIENTED_EDGE('',*,*,#12391,.T.);
#15949=ORIENTED_EDGE('',*,*,#12387,.T.);
#15950=ORIENTED_EDGE('',*,*,#12388,.T.);
#15951=ORIENTED_EDGE('',*,*,#12391,.F.);
#15952=ORIENTED_EDGE('',*,*,#12390,.F.);
#15953=ORIENTED_EDGE('',*,*,#12392,.T.);
#15954=ORIENTED_EDGE('',*,*,#12393,.F.);
#15955=ORIENTED_EDGE('',*,*,#12392,.F.);
#15956=ORIENTED_EDGE('',*,*,#12393,.T.);
#15957=ORIENTED_EDGE('',*,*,#12394,.T.);
#15958=ORIENTED_EDGE('',*,*,#12395,.T.);
#15959=ORIENTED_EDGE('',*,*,#12394,.F.);
#15960=ORIENTED_EDGE('',*,*,#12396,.F.);
#15961=ORIENTED_EDGE('',*,*,#12397,.T.);
#15962=ORIENTED_EDGE('',*,*,#12398,.T.);
#15963=ORIENTED_EDGE('',*,*,#12399,.T.);
#15964=ORIENTED_EDGE('',*,*,#12395,.F.);
#15965=ORIENTED_EDGE('',*,*,#12379,.T.);
#15966=ORIENTED_EDGE('',*,*,#12400,.T.);
#15967=ORIENTED_EDGE('',*,*,#12401,.T.);
#15968=ORIENTED_EDGE('',*,*,#12402,.T.);
#15969=ORIENTED_EDGE('',*,*,#12400,.F.);
#15970=ORIENTED_EDGE('',*,*,#12403,.F.);
#15971=ORIENTED_EDGE('',*,*,#12404,.T.);
#15972=ORIENTED_EDGE('',*,*,#12401,.F.);
#15973=ORIENTED_EDGE('',*,*,#12402,.F.);
#15974=ORIENTED_EDGE('',*,*,#12404,.F.);
#15975=ORIENTED_EDGE('',*,*,#12374,.T.);
#15976=ORIENTED_EDGE('',*,*,#12405,.T.);
#15977=ORIENTED_EDGE('',*,*,#12406,.T.);
#15978=ORIENTED_EDGE('',*,*,#12407,.T.);
#15979=ORIENTED_EDGE('',*,*,#12405,.F.);
#15980=ORIENTED_EDGE('',*,*,#12408,.F.);
#15981=ORIENTED_EDGE('',*,*,#12409,.T.);
#15982=ORIENTED_EDGE('',*,*,#12406,.F.);
#15983=ORIENTED_EDGE('',*,*,#12407,.F.);
#15984=ORIENTED_EDGE('',*,*,#12409,.F.);
#15985=ORIENTED_EDGE('',*,*,#12378,.T.);
#15986=ORIENTED_EDGE('',*,*,#12410,.T.);
#15987=ORIENTED_EDGE('',*,*,#12411,.T.);
#15988=ORIENTED_EDGE('',*,*,#12412,.T.);
#15989=ORIENTED_EDGE('',*,*,#12410,.F.);
#15990=ORIENTED_EDGE('',*,*,#12413,.F.);
#15991=ORIENTED_EDGE('',*,*,#12414,.T.);
#15992=ORIENTED_EDGE('',*,*,#12411,.F.);
#15993=ORIENTED_EDGE('',*,*,#12412,.F.);
#15994=ORIENTED_EDGE('',*,*,#12414,.F.);
#15995=ORIENTED_EDGE('',*,*,#12375,.T.);
#15996=ORIENTED_EDGE('',*,*,#12415,.T.);
#15997=ORIENTED_EDGE('',*,*,#12416,.T.);
#15998=ORIENTED_EDGE('',*,*,#12417,.T.);
#15999=ORIENTED_EDGE('',*,*,#12415,.F.);
#16000=ORIENTED_EDGE('',*,*,#12418,.F.);
#16001=ORIENTED_EDGE('',*,*,#12419,.T.);
#16002=ORIENTED_EDGE('',*,*,#12416,.F.);
#16003=ORIENTED_EDGE('',*,*,#12417,.F.);
#16004=ORIENTED_EDGE('',*,*,#12419,.F.);
#16005=ORIENTED_EDGE('',*,*,#12377,.T.);
#16006=ORIENTED_EDGE('',*,*,#12420,.T.);
#16007=ORIENTED_EDGE('',*,*,#12421,.T.);
#16008=ORIENTED_EDGE('',*,*,#12422,.T.);
#16009=ORIENTED_EDGE('',*,*,#12420,.F.);
#16010=ORIENTED_EDGE('',*,*,#12423,.F.);
#16011=ORIENTED_EDGE('',*,*,#12424,.T.);
#16012=ORIENTED_EDGE('',*,*,#12421,.F.);
#16013=ORIENTED_EDGE('',*,*,#12422,.F.);
#16014=ORIENTED_EDGE('',*,*,#12424,.F.);
#16015=ORIENTED_EDGE('',*,*,#12376,.T.);
#16016=ORIENTED_EDGE('',*,*,#12425,.T.);
#16017=ORIENTED_EDGE('',*,*,#12426,.T.);
#16018=ORIENTED_EDGE('',*,*,#12427,.T.);
#16019=ORIENTED_EDGE('',*,*,#12425,.F.);
#16020=ORIENTED_EDGE('',*,*,#12428,.F.);
#16021=ORIENTED_EDGE('',*,*,#12429,.T.);
#16022=ORIENTED_EDGE('',*,*,#12426,.F.);
#16023=ORIENTED_EDGE('',*,*,#12427,.F.);
#16024=ORIENTED_EDGE('',*,*,#12429,.F.);
#16025=ORIENTED_EDGE('',*,*,#12363,.T.);
#16026=ORIENTED_EDGE('',*,*,#12430,.T.);
#16027=ORIENTED_EDGE('',*,*,#12431,.T.);
#16028=ORIENTED_EDGE('',*,*,#12432,.T.);
#16029=ORIENTED_EDGE('',*,*,#12430,.F.);
#16030=ORIENTED_EDGE('',*,*,#12431,.F.);
#16031=ORIENTED_EDGE('',*,*,#12432,.F.);
#16032=ORIENTED_EDGE('',*,*,#12433,.T.);
#16033=ORIENTED_EDGE('',*,*,#12434,.F.);
#16034=ORIENTED_EDGE('',*,*,#12433,.F.);
#16035=ORIENTED_EDGE('',*,*,#12434,.T.);
#16036=ORIENTED_EDGE('',*,*,#12435,.T.);
#16037=ORIENTED_EDGE('',*,*,#12436,.T.);
#16038=ORIENTED_EDGE('',*,*,#12435,.F.);
#16039=ORIENTED_EDGE('',*,*,#12436,.F.);
#16040=ORIENTED_EDGE('',*,*,#12437,.T.);
#16041=ORIENTED_EDGE('',*,*,#12357,.T.);
#16042=ORIENTED_EDGE('',*,*,#12438,.T.);
#16043=ORIENTED_EDGE('',*,*,#12439,.T.);
#16044=ORIENTED_EDGE('',*,*,#12438,.F.);
#16045=ORIENTED_EDGE('',*,*,#12439,.F.);
#16046=ORIENTED_EDGE('',*,*,#12440,.F.);
#16047=ORIENTED_EDGE('',*,*,#12440,.T.);
#16048=ORIENTED_EDGE('',*,*,#12441,.T.);
#16049=ORIENTED_EDGE('',*,*,#12437,.F.);
#16050=ORIENTED_EDGE('',*,*,#12441,.F.);
#16051=ORIENTED_EDGE('',*,*,#12442,.T.);
#16052=ORIENTED_EDGE('',*,*,#12443,.T.);
#16053=ORIENTED_EDGE('',*,*,#12442,.F.);
#16054=ORIENTED_EDGE('',*,*,#12443,.F.);
#16055=ORIENTED_EDGE('',*,*,#12444,.T.);
#16056=ORIENTED_EDGE('',*,*,#12445,.T.);
#16057=ORIENTED_EDGE('',*,*,#12444,.F.);
#16058=ORIENTED_EDGE('',*,*,#12445,.F.);
#16059=ORIENTED_EDGE('',*,*,#12446,.T.);
#16060=ORIENTED_EDGE('',*,*,#12399,.F.);
#16061=ORIENTED_EDGE('',*,*,#12446,.F.);
#16062=ORIENTED_EDGE('',*,*,#12447,.T.);
#16063=ORIENTED_EDGE('',*,*,#12448,.T.);
#16064=ORIENTED_EDGE('',*,*,#12447,.F.);
#16065=ORIENTED_EDGE('',*,*,#12448,.F.);
#16066=ORIENTED_EDGE('',*,*,#12449,.T.);
#16067=ORIENTED_EDGE('',*,*,#12450,.T.);
#16068=ORIENTED_EDGE('',*,*,#12449,.F.);
#16069=ORIENTED_EDGE('',*,*,#12450,.F.);
#16070=ORIENTED_EDGE('',*,*,#12451,.T.);
#16071=ORIENTED_EDGE('',*,*,#12398,.F.);
#16072=ORIENTED_EDGE('',*,*,#12451,.F.);
#16073=ORIENTED_EDGE('',*,*,#12452,.T.);
#16074=ORIENTED_EDGE('',*,*,#12453,.T.);
#16075=ORIENTED_EDGE('',*,*,#12452,.F.);
#16076=ORIENTED_EDGE('',*,*,#12453,.F.);
#16077=ORIENTED_EDGE('',*,*,#12454,.T.);
#16078=ORIENTED_EDGE('',*,*,#12455,.T.);
#16079=ORIENTED_EDGE('',*,*,#12454,.F.);
#16080=ORIENTED_EDGE('',*,*,#12455,.F.);
#16081=ORIENTED_EDGE('',*,*,#12456,.T.);
#16082=ORIENTED_EDGE('',*,*,#12397,.F.);
#16083=ORIENTED_EDGE('',*,*,#12456,.F.);
#16084=ORIENTED_EDGE('',*,*,#12370,.F.);
#16085=ORIENTED_EDGE('',*,*,#12457,.T.);
#16086=ORIENTED_EDGE('',*,*,#12458,.T.);
#16087=ORIENTED_EDGE('',*,*,#12457,.F.);
#16088=ORIENTED_EDGE('',*,*,#12458,.F.);
#16089=ORIENTED_EDGE('',*,*,#12459,.T.);
#16090=ORIENTED_EDGE('',*,*,#12460,.T.);
#16091=ORIENTED_EDGE('',*,*,#12459,.F.);
#16092=ORIENTED_EDGE('',*,*,#12460,.F.);
#16093=ORIENTED_EDGE('',*,*,#12461,.T.);
#16094=ORIENTED_EDGE('',*,*,#12462,.T.);
#16095=ORIENTED_EDGE('',*,*,#12461,.F.);
#16096=ORIENTED_EDGE('',*,*,#12428,.T.);
#16097=ORIENTED_EDGE('',*,*,#12462,.F.);
#16098=ORIENTED_EDGE('',*,*,#12369,.F.);
#16099=ORIENTED_EDGE('',*,*,#12463,.T.);
#16100=ORIENTED_EDGE('',*,*,#12464,.T.);
#16101=ORIENTED_EDGE('',*,*,#12463,.F.);
#16102=ORIENTED_EDGE('',*,*,#12464,.F.);
#16103=ORIENTED_EDGE('',*,*,#12465,.T.);
#16104=ORIENTED_EDGE('',*,*,#12466,.T.);
#16105=ORIENTED_EDGE('',*,*,#12465,.F.);
#16106=ORIENTED_EDGE('',*,*,#12466,.F.);
#16107=ORIENTED_EDGE('',*,*,#12467,.T.);
#16108=ORIENTED_EDGE('',*,*,#12468,.T.);
#16109=ORIENTED_EDGE('',*,*,#12467,.F.);
#16110=ORIENTED_EDGE('',*,*,#12423,.T.);
#16111=ORIENTED_EDGE('',*,*,#12468,.F.);
#16112=ORIENTED_EDGE('',*,*,#12368,.F.);
#16113=ORIENTED_EDGE('',*,*,#12469,.T.);
#16114=ORIENTED_EDGE('',*,*,#12470,.T.);
#16115=ORIENTED_EDGE('',*,*,#12469,.F.);
#16116=ORIENTED_EDGE('',*,*,#12470,.F.);
#16117=ORIENTED_EDGE('',*,*,#12471,.T.);
#16118=ORIENTED_EDGE('',*,*,#12472,.T.);
#16119=ORIENTED_EDGE('',*,*,#12471,.F.);
#16120=ORIENTED_EDGE('',*,*,#12472,.F.);
#16121=ORIENTED_EDGE('',*,*,#12473,.T.);
#16122=ORIENTED_EDGE('',*,*,#12474,.T.);
#16123=ORIENTED_EDGE('',*,*,#12473,.F.);
#16124=ORIENTED_EDGE('',*,*,#12418,.T.);
#16125=ORIENTED_EDGE('',*,*,#12474,.F.);
#16126=ORIENTED_EDGE('',*,*,#12367,.F.);
#16127=ORIENTED_EDGE('',*,*,#12475,.T.);
#16128=ORIENTED_EDGE('',*,*,#12476,.T.);
#16129=ORIENTED_EDGE('',*,*,#12475,.F.);
#16130=ORIENTED_EDGE('',*,*,#12476,.F.);
#16131=ORIENTED_EDGE('',*,*,#12477,.T.);
#16132=ORIENTED_EDGE('',*,*,#12478,.T.);
#16133=ORIENTED_EDGE('',*,*,#12477,.F.);
#16134=ORIENTED_EDGE('',*,*,#12478,.F.);
#16135=ORIENTED_EDGE('',*,*,#12479,.T.);
#16136=ORIENTED_EDGE('',*,*,#12480,.T.);
#16137=ORIENTED_EDGE('',*,*,#12479,.F.);
#16138=ORIENTED_EDGE('',*,*,#12413,.T.);
#16139=ORIENTED_EDGE('',*,*,#12480,.F.);
#16140=ORIENTED_EDGE('',*,*,#12366,.F.);
#16141=ORIENTED_EDGE('',*,*,#12481,.T.);
#16142=ORIENTED_EDGE('',*,*,#12482,.T.);
#16143=ORIENTED_EDGE('',*,*,#12481,.F.);
#16144=ORIENTED_EDGE('',*,*,#12482,.F.);
#16145=ORIENTED_EDGE('',*,*,#12483,.T.);
#16146=ORIENTED_EDGE('',*,*,#12484,.T.);
#16147=ORIENTED_EDGE('',*,*,#12483,.F.);
#16148=ORIENTED_EDGE('',*,*,#12484,.F.);
#16149=ORIENTED_EDGE('',*,*,#12485,.T.);
#16150=ORIENTED_EDGE('',*,*,#12486,.T.);
#16151=ORIENTED_EDGE('',*,*,#12485,.F.);
#16152=ORIENTED_EDGE('',*,*,#12408,.T.);
#16153=ORIENTED_EDGE('',*,*,#12486,.F.);
#16154=ORIENTED_EDGE('',*,*,#12365,.F.);
#16155=ORIENTED_EDGE('',*,*,#12487,.T.);
#16156=ORIENTED_EDGE('',*,*,#12488,.T.);
#16157=ORIENTED_EDGE('',*,*,#12487,.F.);
#16158=ORIENTED_EDGE('',*,*,#12488,.F.);
#16159=ORIENTED_EDGE('',*,*,#12489,.T.);
#16160=ORIENTED_EDGE('',*,*,#12490,.T.);
#16161=ORIENTED_EDGE('',*,*,#12489,.F.);
#16162=ORIENTED_EDGE('',*,*,#12490,.F.);
#16163=ORIENTED_EDGE('',*,*,#12491,.T.);
#16164=ORIENTED_EDGE('',*,*,#12492,.T.);
#16165=ORIENTED_EDGE('',*,*,#12491,.F.);
#16166=ORIENTED_EDGE('',*,*,#12403,.T.);
#16167=ORIENTED_EDGE('',*,*,#12492,.F.);
#16168=ORIENTED_EDGE('',*,*,#12396,.T.);
#16169=ORIENTED_EDGE('',*,*,#12493,.T.);
#16170=ORIENTED_EDGE('',*,*,#12494,.T.);
#16171=ORIENTED_EDGE('',*,*,#12495,.T.);
#16172=ORIENTED_EDGE('',*,*,#12493,.F.);
#16173=ORIENTED_EDGE('',*,*,#12494,.F.);
#16174=ORIENTED_EDGE('',*,*,#12495,.F.);
#16175=ORIENTED_EDGE('',*,*,#12496,.T.);
#16176=ORIENTED_EDGE('',*,*,#12364,.T.);
#16177=ORIENTED_EDGE('',*,*,#12496,.F.);
#16178=ORIENTED_EDGE('',*,*,#12497,.T.);
#16179=ORIENTED_EDGE('',*,*,#12498,.T.);
#16180=ORIENTED_EDGE('',*,*,#12497,.F.);
#16181=ORIENTED_EDGE('',*,*,#12498,.F.);
#16182=ORIENTED_EDGE('',*,*,#12499,.T.);
#16183=ORIENTED_EDGE('',*,*,#12500,.T.);
#16184=ORIENTED_EDGE('',*,*,#12499,.F.);
#16185=ORIENTED_EDGE('',*,*,#12500,.F.);
#16186=ORIENTED_EDGE('',*,*,#12501,.T.);
#16187=ORIENTED_EDGE('',*,*,#12502,.F.);
#16188=ORIENTED_EDGE('',*,*,#12501,.F.);
#16189=ORIENTED_EDGE('',*,*,#12503,.T.);
#16190=ORIENTED_EDGE('',*,*,#12504,.T.);
#16191=ORIENTED_EDGE('',*,*,#12503,.F.);
#16192=ORIENTED_EDGE('',*,*,#12504,.F.);
#16193=ORIENTED_EDGE('',*,*,#12505,.T.);
#16194=ORIENTED_EDGE('',*,*,#12506,.T.);
#16195=ORIENTED_EDGE('',*,*,#12505,.F.);
#16196=ORIENTED_EDGE('',*,*,#12506,.F.);
#16197=ORIENTED_EDGE('',*,*,#12507,.T.);
#16198=ORIENTED_EDGE('',*,*,#12508,.F.);
#16199=ORIENTED_EDGE('',*,*,#12507,.F.);
#16200=ORIENTED_EDGE('',*,*,#12509,.T.);
#16201=ORIENTED_EDGE('',*,*,#12510,.T.);
#16202=ORIENTED_EDGE('',*,*,#12509,.F.);
#16203=ORIENTED_EDGE('',*,*,#12510,.F.);
#16204=ORIENTED_EDGE('',*,*,#12511,.T.);
#16205=ORIENTED_EDGE('',*,*,#12512,.T.);
#16206=ORIENTED_EDGE('',*,*,#12511,.F.);
#16207=ORIENTED_EDGE('',*,*,#12512,.F.);
#16208=ORIENTED_EDGE('',*,*,#12513,.T.);
#16209=ORIENTED_EDGE('',*,*,#12514,.F.);
#16210=ORIENTED_EDGE('',*,*,#12513,.F.);
#16211=ORIENTED_EDGE('',*,*,#12515,.T.);
#16212=ORIENTED_EDGE('',*,*,#12516,.T.);
#16213=ORIENTED_EDGE('',*,*,#12515,.F.);
#16214=ORIENTED_EDGE('',*,*,#12516,.F.);
#16215=ORIENTED_EDGE('',*,*,#12517,.T.);
#16216=ORIENTED_EDGE('',*,*,#12518,.T.);
#16217=ORIENTED_EDGE('',*,*,#12517,.F.);
#16218=ORIENTED_EDGE('',*,*,#12518,.F.);
#16219=ORIENTED_EDGE('',*,*,#12519,.T.);
#16220=ORIENTED_EDGE('',*,*,#12520,.F.);
#16221=ORIENTED_EDGE('',*,*,#12519,.F.);
#16222=ORIENTED_EDGE('',*,*,#12521,.T.);
#16223=ORIENTED_EDGE('',*,*,#12522,.T.);
#16224=ORIENTED_EDGE('',*,*,#12521,.F.);
#16225=ORIENTED_EDGE('',*,*,#12522,.F.);
#16226=ORIENTED_EDGE('',*,*,#12523,.T.);
#16227=ORIENTED_EDGE('',*,*,#12524,.T.);
#16228=ORIENTED_EDGE('',*,*,#12523,.F.);
#16229=ORIENTED_EDGE('',*,*,#12524,.F.);
#16230=ORIENTED_EDGE('',*,*,#12525,.T.);
#16231=ORIENTED_EDGE('',*,*,#12526,.F.);
#16232=ORIENTED_EDGE('',*,*,#12525,.F.);
#16233=ORIENTED_EDGE('',*,*,#12527,.T.);
#16234=ORIENTED_EDGE('',*,*,#12528,.T.);
#16235=ORIENTED_EDGE('',*,*,#12527,.F.);
#16236=ORIENTED_EDGE('',*,*,#12528,.F.);
#16237=ORIENTED_EDGE('',*,*,#12529,.T.);
#16238=ORIENTED_EDGE('',*,*,#12530,.T.);
#16239=ORIENTED_EDGE('',*,*,#12529,.F.);
#16240=ORIENTED_EDGE('',*,*,#12530,.F.);
#16241=ORIENTED_EDGE('',*,*,#12531,.T.);
#16242=ORIENTED_EDGE('',*,*,#12532,.F.);
#16243=ORIENTED_EDGE('',*,*,#12531,.F.);
#16244=ORIENTED_EDGE('',*,*,#12533,.T.);
#16245=ORIENTED_EDGE('',*,*,#12534,.T.);
#16246=ORIENTED_EDGE('',*,*,#12533,.F.);
#16247=ORIENTED_EDGE('',*,*,#12534,.F.);
#16248=ORIENTED_EDGE('',*,*,#12535,.T.);
#16249=ORIENTED_EDGE('',*,*,#12536,.T.);
#16250=ORIENTED_EDGE('',*,*,#12535,.F.);
#16251=ORIENTED_EDGE('',*,*,#12536,.F.);
#16252=ORIENTED_EDGE('',*,*,#12537,.T.);
#16253=ORIENTED_EDGE('',*,*,#12538,.F.);
#16254=ORIENTED_EDGE('',*,*,#12537,.F.);
#16255=ORIENTED_EDGE('',*,*,#12539,.T.);
#16256=ORIENTED_EDGE('',*,*,#12540,.T.);
#16257=ORIENTED_EDGE('',*,*,#12539,.F.);
#16258=ORIENTED_EDGE('',*,*,#12540,.F.);
#16259=ORIENTED_EDGE('',*,*,#12541,.T.);
#16260=ORIENTED_EDGE('',*,*,#12542,.T.);
#16261=ORIENTED_EDGE('',*,*,#12541,.F.);
#16262=ORIENTED_EDGE('',*,*,#12542,.F.);
#16263=ORIENTED_EDGE('',*,*,#12543,.T.);
#16264=ORIENTED_EDGE('',*,*,#12544,.F.);
#16265=ORIENTED_EDGE('',*,*,#12543,.F.);
#16266=ORIENTED_EDGE('',*,*,#12545,.T.);
#16267=ORIENTED_EDGE('',*,*,#12546,.T.);
#16268=ORIENTED_EDGE('',*,*,#12545,.F.);
#16269=ORIENTED_EDGE('',*,*,#12546,.F.);
#16270=ORIENTED_EDGE('',*,*,#12547,.T.);
#16271=ORIENTED_EDGE('',*,*,#12548,.T.);
#16272=ORIENTED_EDGE('',*,*,#12547,.F.);
#16273=ORIENTED_EDGE('',*,*,#12548,.F.);
#16274=ORIENTED_EDGE('',*,*,#12549,.T.);
#16275=ORIENTED_EDGE('',*,*,#12550,.F.);
#16276=ORIENTED_EDGE('',*,*,#12549,.F.);
#16277=ORIENTED_EDGE('',*,*,#12551,.T.);
#16278=ORIENTED_EDGE('',*,*,#12552,.T.);
#16279=ORIENTED_EDGE('',*,*,#12551,.F.);
#16280=ORIENTED_EDGE('',*,*,#12552,.F.);
#16281=ORIENTED_EDGE('',*,*,#12553,.T.);
#16282=ORIENTED_EDGE('',*,*,#12554,.T.);
#16283=ORIENTED_EDGE('',*,*,#12553,.F.);
#16284=ORIENTED_EDGE('',*,*,#12554,.F.);
#16285=ORIENTED_EDGE('',*,*,#12555,.T.);
#16286=ORIENTED_EDGE('',*,*,#12556,.F.);
#16287=ORIENTED_EDGE('',*,*,#12555,.F.);
#16288=ORIENTED_EDGE('',*,*,#12557,.T.);
#16289=ORIENTED_EDGE('',*,*,#12558,.T.);
#16290=ORIENTED_EDGE('',*,*,#12557,.F.);
#16291=ORIENTED_EDGE('',*,*,#12558,.F.);
#16292=ORIENTED_EDGE('',*,*,#12559,.T.);
#16293=ORIENTED_EDGE('',*,*,#12560,.T.);
#16294=ORIENTED_EDGE('',*,*,#12559,.F.);
#16295=ORIENTED_EDGE('',*,*,#12560,.F.);
#16296=ORIENTED_EDGE('',*,*,#12561,.T.);
#16297=ORIENTED_EDGE('',*,*,#12562,.F.);
#16298=ORIENTED_EDGE('',*,*,#12561,.F.);
#16299=ORIENTED_EDGE('',*,*,#12563,.T.);
#16300=ORIENTED_EDGE('',*,*,#12564,.T.);
#16301=ORIENTED_EDGE('',*,*,#12563,.F.);
#16302=ORIENTED_EDGE('',*,*,#12564,.F.);
#16303=ORIENTED_EDGE('',*,*,#12565,.T.);
#16304=ORIENTED_EDGE('',*,*,#12566,.T.);
#16305=ORIENTED_EDGE('',*,*,#12565,.F.);
#16306=ORIENTED_EDGE('',*,*,#12566,.F.);
#16307=ORIENTED_EDGE('',*,*,#12567,.T.);
#16308=ORIENTED_EDGE('',*,*,#12568,.F.);
#16309=ORIENTED_EDGE('',*,*,#12567,.F.);
#16310=ORIENTED_EDGE('',*,*,#12569,.T.);
#16311=ORIENTED_EDGE('',*,*,#12570,.T.);
#16312=ORIENTED_EDGE('',*,*,#12569,.F.);
#16313=ORIENTED_EDGE('',*,*,#12570,.F.);
#16314=ORIENTED_EDGE('',*,*,#12571,.T.);
#16315=ORIENTED_EDGE('',*,*,#12572,.T.);
#16316=ORIENTED_EDGE('',*,*,#12571,.F.);
#16317=ORIENTED_EDGE('',*,*,#12572,.F.);
#16318=ORIENTED_EDGE('',*,*,#12573,.T.);
#16319=ORIENTED_EDGE('',*,*,#12574,.F.);
#16320=ORIENTED_EDGE('',*,*,#12573,.F.);
#16321=ORIENTED_EDGE('',*,*,#12575,.T.);
#16322=ORIENTED_EDGE('',*,*,#12576,.T.);
#16323=ORIENTED_EDGE('',*,*,#12575,.F.);
#16324=ORIENTED_EDGE('',*,*,#12576,.F.);
#16325=ORIENTED_EDGE('',*,*,#12577,.T.);
#16326=ORIENTED_EDGE('',*,*,#12578,.T.);
#16327=ORIENTED_EDGE('',*,*,#12577,.F.);
#16328=ORIENTED_EDGE('',*,*,#12578,.F.);
#16329=ORIENTED_EDGE('',*,*,#12579,.T.);
#16330=ORIENTED_EDGE('',*,*,#12580,.F.);
#16331=ORIENTED_EDGE('',*,*,#12579,.F.);
#16332=ORIENTED_EDGE('',*,*,#12581,.T.);
#16333=ORIENTED_EDGE('',*,*,#12582,.T.);
#16334=ORIENTED_EDGE('',*,*,#12581,.F.);
#16335=ORIENTED_EDGE('',*,*,#12582,.F.);
#16336=ORIENTED_EDGE('',*,*,#12583,.T.);
#16337=ORIENTED_EDGE('',*,*,#12584,.T.);
#16338=ORIENTED_EDGE('',*,*,#12583,.F.);
#16339=ORIENTED_EDGE('',*,*,#12584,.F.);
#16340=ORIENTED_EDGE('',*,*,#12585,.T.);
#16341=ORIENTED_EDGE('',*,*,#12586,.F.);
#16342=ORIENTED_EDGE('',*,*,#12585,.F.);
#16343=ORIENTED_EDGE('',*,*,#12587,.T.);
#16344=ORIENTED_EDGE('',*,*,#12588,.T.);
#16345=ORIENTED_EDGE('',*,*,#12587,.F.);
#16346=ORIENTED_EDGE('',*,*,#12588,.F.);
#16347=ORIENTED_EDGE('',*,*,#12589,.T.);
#16348=ORIENTED_EDGE('',*,*,#12590,.T.);
#16349=ORIENTED_EDGE('',*,*,#12589,.F.);
#16350=ORIENTED_EDGE('',*,*,#12590,.F.);
#16351=ORIENTED_EDGE('',*,*,#12591,.T.);
#16352=ORIENTED_EDGE('',*,*,#12592,.F.);
#16353=ORIENTED_EDGE('',*,*,#12591,.F.);
#16354=ORIENTED_EDGE('',*,*,#12593,.T.);
#16355=ORIENTED_EDGE('',*,*,#12594,.T.);
#16356=ORIENTED_EDGE('',*,*,#12593,.F.);
#16357=ORIENTED_EDGE('',*,*,#12594,.F.);
#16358=ORIENTED_EDGE('',*,*,#12595,.T.);
#16359=ORIENTED_EDGE('',*,*,#12596,.T.);
#16360=ORIENTED_EDGE('',*,*,#12595,.F.);
#16361=ORIENTED_EDGE('',*,*,#12596,.F.);
#16362=ORIENTED_EDGE('',*,*,#12597,.T.);
#16363=ORIENTED_EDGE('',*,*,#12598,.F.);
#16364=ORIENTED_EDGE('',*,*,#12597,.F.);
#16365=ORIENTED_EDGE('',*,*,#12599,.T.);
#16366=ORIENTED_EDGE('',*,*,#12600,.T.);
#16367=ORIENTED_EDGE('',*,*,#12599,.F.);
#16368=ORIENTED_EDGE('',*,*,#12600,.F.);
#16369=ORIENTED_EDGE('',*,*,#12601,.T.);
#16370=ORIENTED_EDGE('',*,*,#12602,.T.);
#16371=ORIENTED_EDGE('',*,*,#12601,.F.);
#16372=ORIENTED_EDGE('',*,*,#12602,.F.);
#16373=ORIENTED_EDGE('',*,*,#12603,.T.);
#16374=ORIENTED_EDGE('',*,*,#12604,.F.);
#16375=ORIENTED_EDGE('',*,*,#12603,.F.);
#16376=ORIENTED_EDGE('',*,*,#12605,.T.);
#16377=ORIENTED_EDGE('',*,*,#12606,.T.);
#16378=ORIENTED_EDGE('',*,*,#12607,.T.);
#16379=ORIENTED_EDGE('',*,*,#12608,.T.);
#16380=ORIENTED_EDGE('',*,*,#12606,.F.);
#16381=ORIENTED_EDGE('',*,*,#12609,.F.);
#16382=ORIENTED_EDGE('',*,*,#12610,.F.);
#16383=ORIENTED_EDGE('',*,*,#12611,.T.);
#16384=ORIENTED_EDGE('',*,*,#12607,.F.);
#16385=ORIENTED_EDGE('',*,*,#12608,.F.);
#16386=ORIENTED_EDGE('',*,*,#12611,.F.);
#16387=ORIENTED_EDGE('',*,*,#12612,.F.);
#16388=ORIENTED_EDGE('',*,*,#12502,.T.);
#16389=ORIENTED_EDGE('',*,*,#12508,.T.);
#16390=ORIENTED_EDGE('',*,*,#12514,.T.);
#16391=ORIENTED_EDGE('',*,*,#12520,.T.);
#16392=ORIENTED_EDGE('',*,*,#12526,.T.);
#16393=ORIENTED_EDGE('',*,*,#12532,.T.);
#16394=ORIENTED_EDGE('',*,*,#12605,.F.);
#16395=ORIENTED_EDGE('',*,*,#12609,.T.);
#16396=ORIENTED_EDGE('',*,*,#12610,.T.);
#16397=ORIENTED_EDGE('',*,*,#12613,.T.);
#16398=ORIENTED_EDGE('',*,*,#12614,.T.);
#16399=ORIENTED_EDGE('',*,*,#12613,.F.);
#16400=ORIENTED_EDGE('',*,*,#12615,.F.);
#16401=ORIENTED_EDGE('',*,*,#12544,.T.);
#16402=ORIENTED_EDGE('',*,*,#12556,.T.);
#16403=ORIENTED_EDGE('',*,*,#12568,.T.);
#16404=ORIENTED_EDGE('',*,*,#12574,.T.);
#16405=ORIENTED_EDGE('',*,*,#12580,.T.);
#16406=ORIENTED_EDGE('',*,*,#12586,.T.);
#16407=ORIENTED_EDGE('',*,*,#12592,.T.);
#16408=ORIENTED_EDGE('',*,*,#12598,.T.);
#16409=ORIENTED_EDGE('',*,*,#12604,.T.);
#16410=ORIENTED_EDGE('',*,*,#12614,.F.);
#16411=ORIENTED_EDGE('',*,*,#12562,.T.);
#16412=ORIENTED_EDGE('',*,*,#12550,.T.);
#16413=ORIENTED_EDGE('',*,*,#12538,.T.);
#16414=ORIENTED_EDGE('',*,*,#12615,.T.);
#16415=ORIENTED_EDGE('',*,*,#12616,.T.);
#16416=ORIENTED_EDGE('',*,*,#12617,.T.);
#16417=ORIENTED_EDGE('',*,*,#12618,.T.);
#16418=ORIENTED_EDGE('',*,*,#12616,.F.);
#16419=ORIENTED_EDGE('',*,*,#12617,.F.);
#16420=ORIENTED_EDGE('',*,*,#12618,.F.);
#16421=ORIENTED_EDGE('',*,*,#12619,.T.);
#16422=ORIENTED_EDGE('',*,*,#12620,.F.);
#16423=ORIENTED_EDGE('',*,*,#12621,.F.);
#16424=ORIENTED_EDGE('',*,*,#12619,.F.);
#16425=ORIENTED_EDGE('',*,*,#12620,.T.);
#16426=ORIENTED_EDGE('',*,*,#12621,.T.);
#16427=ORIENTED_EDGE('',*,*,#12622,.T.);
#16428=ORIENTED_EDGE('',*,*,#12612,.T.);
#16429=ORIENTED_EDGE('',*,*,#12622,.F.);
#16430=ORIENTED_EDGE('',*,*,#12623,.T.);
#16431=ORIENTED_EDGE('',*,*,#12624,.T.);
#16432=ORIENTED_EDGE('',*,*,#12623,.F.);
#16433=ORIENTED_EDGE('',*,*,#12624,.F.);
#16434=ORIENTED_EDGE('',*,*,#12625,.T.);
#16435=ORIENTED_EDGE('',*,*,#12626,.T.);
#16436=ORIENTED_EDGE('',*,*,#12625,.F.);
#16437=ORIENTED_EDGE('',*,*,#12626,.F.);
#16438=ORIENTED_EDGE('',*,*,#12627,.T.);
#16439=ORIENTED_EDGE('',*,*,#12628,.F.);
#16440=ORIENTED_EDGE('',*,*,#12627,.F.);
#16441=ORIENTED_EDGE('',*,*,#12629,.T.);
#16442=ORIENTED_EDGE('',*,*,#12630,.T.);
#16443=ORIENTED_EDGE('',*,*,#12629,.F.);
#16444=ORIENTED_EDGE('',*,*,#12630,.F.);
#16445=ORIENTED_EDGE('',*,*,#12631,.T.);
#16446=ORIENTED_EDGE('',*,*,#12632,.T.);
#16447=ORIENTED_EDGE('',*,*,#12631,.F.);
#16448=ORIENTED_EDGE('',*,*,#12632,.F.);
#16449=ORIENTED_EDGE('',*,*,#12633,.T.);
#16450=ORIENTED_EDGE('',*,*,#12634,.F.);
#16451=ORIENTED_EDGE('',*,*,#12633,.F.);
#16452=ORIENTED_EDGE('',*,*,#12635,.T.);
#16453=ORIENTED_EDGE('',*,*,#12636,.T.);
#16454=ORIENTED_EDGE('',*,*,#12635,.F.);
#16455=ORIENTED_EDGE('',*,*,#12636,.F.);
#16456=ORIENTED_EDGE('',*,*,#12637,.T.);
#16457=ORIENTED_EDGE('',*,*,#12638,.T.);
#16458=ORIENTED_EDGE('',*,*,#12637,.F.);
#16459=ORIENTED_EDGE('',*,*,#12638,.F.);
#16460=ORIENTED_EDGE('',*,*,#12639,.T.);
#16461=ORIENTED_EDGE('',*,*,#12640,.F.);
#16462=ORIENTED_EDGE('',*,*,#12639,.F.);
#16463=ORIENTED_EDGE('',*,*,#12641,.T.);
#16464=ORIENTED_EDGE('',*,*,#12642,.T.);
#16465=ORIENTED_EDGE('',*,*,#12641,.F.);
#16466=ORIENTED_EDGE('',*,*,#12642,.F.);
#16467=ORIENTED_EDGE('',*,*,#12643,.T.);
#16468=ORIENTED_EDGE('',*,*,#12644,.T.);
#16469=ORIENTED_EDGE('',*,*,#12643,.F.);
#16470=ORIENTED_EDGE('',*,*,#12644,.F.);
#16471=ORIENTED_EDGE('',*,*,#12645,.T.);
#16472=ORIENTED_EDGE('',*,*,#12646,.F.);
#16473=ORIENTED_EDGE('',*,*,#12645,.F.);
#16474=ORIENTED_EDGE('',*,*,#12647,.T.);
#16475=ORIENTED_EDGE('',*,*,#12648,.T.);
#16476=ORIENTED_EDGE('',*,*,#12647,.F.);
#16477=ORIENTED_EDGE('',*,*,#12648,.F.);
#16478=ORIENTED_EDGE('',*,*,#12649,.T.);
#16479=ORIENTED_EDGE('',*,*,#12650,.T.);
#16480=ORIENTED_EDGE('',*,*,#12649,.F.);
#16481=ORIENTED_EDGE('',*,*,#12650,.F.);
#16482=ORIENTED_EDGE('',*,*,#12651,.T.);
#16483=ORIENTED_EDGE('',*,*,#12652,.F.);
#16484=ORIENTED_EDGE('',*,*,#12651,.F.);
#16485=ORIENTED_EDGE('',*,*,#12653,.F.);
#16486=ORIENTED_EDGE('',*,*,#12654,.T.);
#16487=ORIENTED_EDGE('',*,*,#12655,.T.);
#16488=ORIENTED_EDGE('',*,*,#12654,.F.);
#16489=ORIENTED_EDGE('',*,*,#12655,.F.);
#16490=ORIENTED_EDGE('',*,*,#12656,.T.);
#16491=ORIENTED_EDGE('',*,*,#12657,.T.);
#16492=ORIENTED_EDGE('',*,*,#12656,.F.);
#16493=ORIENTED_EDGE('',*,*,#12657,.F.);
#16494=ORIENTED_EDGE('',*,*,#12658,.T.);
#16495=ORIENTED_EDGE('',*,*,#12659,.T.);
#16496=ORIENTED_EDGE('',*,*,#12658,.F.);
#16497=ORIENTED_EDGE('',*,*,#12660,.T.);
#16498=ORIENTED_EDGE('',*,*,#12659,.F.);
#16499=ORIENTED_EDGE('',*,*,#12660,.F.);
#16500=ORIENTED_EDGE('',*,*,#12661,.T.);
#16501=ORIENTED_EDGE('',*,*,#12662,.F.);
#16502=ORIENTED_EDGE('',*,*,#12661,.F.);
#16503=ORIENTED_EDGE('',*,*,#12663,.F.);
#16504=ORIENTED_EDGE('',*,*,#12664,.T.);
#16505=ORIENTED_EDGE('',*,*,#12665,.T.);
#16506=ORIENTED_EDGE('',*,*,#12664,.F.);
#16507=ORIENTED_EDGE('',*,*,#12665,.F.);
#16508=ORIENTED_EDGE('',*,*,#12666,.T.);
#16509=ORIENTED_EDGE('',*,*,#12667,.T.);
#16510=ORIENTED_EDGE('',*,*,#12666,.F.);
#16511=ORIENTED_EDGE('',*,*,#12667,.F.);
#16512=ORIENTED_EDGE('',*,*,#12668,.T.);
#16513=ORIENTED_EDGE('',*,*,#12669,.T.);
#16514=ORIENTED_EDGE('',*,*,#12668,.F.);
#16515=ORIENTED_EDGE('',*,*,#12670,.T.);
#16516=ORIENTED_EDGE('',*,*,#12669,.F.);
#16517=ORIENTED_EDGE('',*,*,#12670,.F.);
#16518=ORIENTED_EDGE('',*,*,#12671,.T.);
#16519=ORIENTED_EDGE('',*,*,#12672,.F.);
#16520=ORIENTED_EDGE('',*,*,#12671,.F.);
#16521=ORIENTED_EDGE('',*,*,#12673,.F.);
#16522=ORIENTED_EDGE('',*,*,#12674,.T.);
#16523=ORIENTED_EDGE('',*,*,#12675,.T.);
#16524=ORIENTED_EDGE('',*,*,#12674,.F.);
#16525=ORIENTED_EDGE('',*,*,#12675,.F.);
#16526=ORIENTED_EDGE('',*,*,#12676,.T.);
#16527=ORIENTED_EDGE('',*,*,#12677,.T.);
#16528=ORIENTED_EDGE('',*,*,#12676,.F.);
#16529=ORIENTED_EDGE('',*,*,#12677,.F.);
#16530=ORIENTED_EDGE('',*,*,#12678,.T.);
#16531=ORIENTED_EDGE('',*,*,#12679,.T.);
#16532=ORIENTED_EDGE('',*,*,#12678,.F.);
#16533=ORIENTED_EDGE('',*,*,#12680,.T.);
#16534=ORIENTED_EDGE('',*,*,#12679,.F.);
#16535=ORIENTED_EDGE('',*,*,#12680,.F.);
#16536=ORIENTED_EDGE('',*,*,#12681,.T.);
#16537=ORIENTED_EDGE('',*,*,#12682,.F.);
#16538=ORIENTED_EDGE('',*,*,#12681,.F.);
#16539=ORIENTED_EDGE('',*,*,#12683,.F.);
#16540=ORIENTED_EDGE('',*,*,#12684,.T.);
#16541=ORIENTED_EDGE('',*,*,#12685,.T.);
#16542=ORIENTED_EDGE('',*,*,#12684,.F.);
#16543=ORIENTED_EDGE('',*,*,#12685,.F.);
#16544=ORIENTED_EDGE('',*,*,#12686,.T.);
#16545=ORIENTED_EDGE('',*,*,#12687,.T.);
#16546=ORIENTED_EDGE('',*,*,#12686,.F.);
#16547=ORIENTED_EDGE('',*,*,#12687,.F.);
#16548=ORIENTED_EDGE('',*,*,#12688,.T.);
#16549=ORIENTED_EDGE('',*,*,#12689,.T.);
#16550=ORIENTED_EDGE('',*,*,#12688,.F.);
#16551=ORIENTED_EDGE('',*,*,#12690,.T.);
#16552=ORIENTED_EDGE('',*,*,#12689,.F.);
#16553=ORIENTED_EDGE('',*,*,#12690,.F.);
#16554=ORIENTED_EDGE('',*,*,#12691,.T.);
#16555=ORIENTED_EDGE('',*,*,#12692,.F.);
#16556=ORIENTED_EDGE('',*,*,#12691,.F.);
#16557=ORIENTED_EDGE('',*,*,#12693,.F.);
#16558=ORIENTED_EDGE('',*,*,#12694,.T.);
#16559=ORIENTED_EDGE('',*,*,#12695,.T.);
#16560=ORIENTED_EDGE('',*,*,#12694,.F.);
#16561=ORIENTED_EDGE('',*,*,#12695,.F.);
#16562=ORIENTED_EDGE('',*,*,#12696,.T.);
#16563=ORIENTED_EDGE('',*,*,#12697,.T.);
#16564=ORIENTED_EDGE('',*,*,#12696,.F.);
#16565=ORIENTED_EDGE('',*,*,#12697,.F.);
#16566=ORIENTED_EDGE('',*,*,#12698,.T.);
#16567=ORIENTED_EDGE('',*,*,#12699,.T.);
#16568=ORIENTED_EDGE('',*,*,#12698,.F.);
#16569=ORIENTED_EDGE('',*,*,#12700,.T.);
#16570=ORIENTED_EDGE('',*,*,#12699,.F.);
#16571=ORIENTED_EDGE('',*,*,#12700,.F.);
#16572=ORIENTED_EDGE('',*,*,#12701,.T.);
#16573=ORIENTED_EDGE('',*,*,#12702,.F.);
#16574=ORIENTED_EDGE('',*,*,#12701,.F.);
#16575=ORIENTED_EDGE('',*,*,#12703,.F.);
#16576=ORIENTED_EDGE('',*,*,#12704,.T.);
#16577=ORIENTED_EDGE('',*,*,#12705,.T.);
#16578=ORIENTED_EDGE('',*,*,#12704,.F.);
#16579=ORIENTED_EDGE('',*,*,#12705,.F.);
#16580=ORIENTED_EDGE('',*,*,#12706,.T.);
#16581=ORIENTED_EDGE('',*,*,#12707,.T.);
#16582=ORIENTED_EDGE('',*,*,#12706,.F.);
#16583=ORIENTED_EDGE('',*,*,#12707,.F.);
#16584=ORIENTED_EDGE('',*,*,#12708,.T.);
#16585=ORIENTED_EDGE('',*,*,#12709,.T.);
#16586=ORIENTED_EDGE('',*,*,#12708,.F.);
#16587=ORIENTED_EDGE('',*,*,#12710,.T.);
#16588=ORIENTED_EDGE('',*,*,#12709,.F.);
#16589=ORIENTED_EDGE('',*,*,#12710,.F.);
#16590=ORIENTED_EDGE('',*,*,#12711,.T.);
#16591=ORIENTED_EDGE('',*,*,#12712,.F.);
#16592=ORIENTED_EDGE('',*,*,#12711,.F.);
#16593=ORIENTED_EDGE('',*,*,#12713,.F.);
#16594=ORIENTED_EDGE('',*,*,#12714,.T.);
#16595=ORIENTED_EDGE('',*,*,#12715,.T.);
#16596=ORIENTED_EDGE('',*,*,#12714,.F.);
#16597=ORIENTED_EDGE('',*,*,#12715,.F.);
#16598=ORIENTED_EDGE('',*,*,#12716,.T.);
#16599=ORIENTED_EDGE('',*,*,#12717,.T.);
#16600=ORIENTED_EDGE('',*,*,#12716,.F.);
#16601=ORIENTED_EDGE('',*,*,#12717,.F.);
#16602=ORIENTED_EDGE('',*,*,#12718,.T.);
#16603=ORIENTED_EDGE('',*,*,#12719,.T.);
#16604=ORIENTED_EDGE('',*,*,#12718,.F.);
#16605=ORIENTED_EDGE('',*,*,#12720,.T.);
#16606=ORIENTED_EDGE('',*,*,#12719,.F.);
#16607=ORIENTED_EDGE('',*,*,#12720,.F.);
#16608=ORIENTED_EDGE('',*,*,#12721,.T.);
#16609=ORIENTED_EDGE('',*,*,#12722,.F.);
#16610=ORIENTED_EDGE('',*,*,#12721,.F.);
#16611=ORIENTED_EDGE('',*,*,#12723,.F.);
#16612=ORIENTED_EDGE('',*,*,#12724,.T.);
#16613=ORIENTED_EDGE('',*,*,#12725,.T.);
#16614=ORIENTED_EDGE('',*,*,#12724,.F.);
#16615=ORIENTED_EDGE('',*,*,#12725,.F.);
#16616=ORIENTED_EDGE('',*,*,#12726,.T.);
#16617=ORIENTED_EDGE('',*,*,#12727,.T.);
#16618=ORIENTED_EDGE('',*,*,#12726,.F.);
#16619=ORIENTED_EDGE('',*,*,#12727,.F.);
#16620=ORIENTED_EDGE('',*,*,#12728,.T.);
#16621=ORIENTED_EDGE('',*,*,#12729,.T.);
#16622=ORIENTED_EDGE('',*,*,#12728,.F.);
#16623=ORIENTED_EDGE('',*,*,#12730,.T.);
#16624=ORIENTED_EDGE('',*,*,#12729,.F.);
#16625=ORIENTED_EDGE('',*,*,#12730,.F.);
#16626=ORIENTED_EDGE('',*,*,#12731,.T.);
#16627=ORIENTED_EDGE('',*,*,#12732,.F.);
#16628=ORIENTED_EDGE('',*,*,#12731,.F.);
#16629=ORIENTED_EDGE('',*,*,#12733,.F.);
#16630=ORIENTED_EDGE('',*,*,#12734,.T.);
#16631=ORIENTED_EDGE('',*,*,#12735,.T.);
#16632=ORIENTED_EDGE('',*,*,#12734,.F.);
#16633=ORIENTED_EDGE('',*,*,#12735,.F.);
#16634=ORIENTED_EDGE('',*,*,#12736,.T.);
#16635=ORIENTED_EDGE('',*,*,#12737,.T.);
#16636=ORIENTED_EDGE('',*,*,#12736,.F.);
#16637=ORIENTED_EDGE('',*,*,#12737,.F.);
#16638=ORIENTED_EDGE('',*,*,#12738,.T.);
#16639=ORIENTED_EDGE('',*,*,#12739,.T.);
#16640=ORIENTED_EDGE('',*,*,#12738,.F.);
#16641=ORIENTED_EDGE('',*,*,#12740,.T.);
#16642=ORIENTED_EDGE('',*,*,#12739,.F.);
#16643=ORIENTED_EDGE('',*,*,#12740,.F.);
#16644=ORIENTED_EDGE('',*,*,#12741,.T.);
#16645=ORIENTED_EDGE('',*,*,#12742,.F.);
#16646=ORIENTED_EDGE('',*,*,#12741,.F.);
#16647=ORIENTED_EDGE('',*,*,#12743,.F.);
#16648=ORIENTED_EDGE('',*,*,#12744,.T.);
#16649=ORIENTED_EDGE('',*,*,#12745,.T.);
#16650=ORIENTED_EDGE('',*,*,#12744,.F.);
#16651=ORIENTED_EDGE('',*,*,#12745,.F.);
#16652=ORIENTED_EDGE('',*,*,#12746,.T.);
#16653=ORIENTED_EDGE('',*,*,#12747,.T.);
#16654=ORIENTED_EDGE('',*,*,#12746,.F.);
#16655=ORIENTED_EDGE('',*,*,#12747,.F.);
#16656=ORIENTED_EDGE('',*,*,#12748,.T.);
#16657=ORIENTED_EDGE('',*,*,#12749,.T.);
#16658=ORIENTED_EDGE('',*,*,#12748,.F.);
#16659=ORIENTED_EDGE('',*,*,#12750,.T.);
#16660=ORIENTED_EDGE('',*,*,#12749,.F.);
#16661=ORIENTED_EDGE('',*,*,#12750,.F.);
#16662=ORIENTED_EDGE('',*,*,#12751,.T.);
#16663=ORIENTED_EDGE('',*,*,#12752,.F.);
#16664=ORIENTED_EDGE('',*,*,#12751,.F.);
#16665=ORIENTED_EDGE('',*,*,#12753,.F.);
#16666=ORIENTED_EDGE('',*,*,#12754,.T.);
#16667=ORIENTED_EDGE('',*,*,#12755,.T.);
#16668=ORIENTED_EDGE('',*,*,#12754,.F.);
#16669=ORIENTED_EDGE('',*,*,#12755,.F.);
#16670=ORIENTED_EDGE('',*,*,#12756,.T.);
#16671=ORIENTED_EDGE('',*,*,#12757,.T.);
#16672=ORIENTED_EDGE('',*,*,#12756,.F.);
#16673=ORIENTED_EDGE('',*,*,#12757,.F.);
#16674=ORIENTED_EDGE('',*,*,#12758,.T.);
#16675=ORIENTED_EDGE('',*,*,#12759,.T.);
#16676=ORIENTED_EDGE('',*,*,#12758,.F.);
#16677=ORIENTED_EDGE('',*,*,#12760,.T.);
#16678=ORIENTED_EDGE('',*,*,#12759,.F.);
#16679=ORIENTED_EDGE('',*,*,#12760,.F.);
#16680=ORIENTED_EDGE('',*,*,#12761,.T.);
#16681=ORIENTED_EDGE('',*,*,#12762,.F.);
#16682=ORIENTED_EDGE('',*,*,#12761,.F.);
#16683=ORIENTED_EDGE('',*,*,#12763,.F.);
#16684=ORIENTED_EDGE('',*,*,#12764,.T.);
#16685=ORIENTED_EDGE('',*,*,#12765,.T.);
#16686=ORIENTED_EDGE('',*,*,#12764,.F.);
#16687=ORIENTED_EDGE('',*,*,#12765,.F.);
#16688=ORIENTED_EDGE('',*,*,#12766,.T.);
#16689=ORIENTED_EDGE('',*,*,#12767,.T.);
#16690=ORIENTED_EDGE('',*,*,#12766,.F.);
#16691=ORIENTED_EDGE('',*,*,#12767,.F.);
#16692=ORIENTED_EDGE('',*,*,#12768,.T.);
#16693=ORIENTED_EDGE('',*,*,#12769,.T.);
#16694=ORIENTED_EDGE('',*,*,#12768,.F.);
#16695=ORIENTED_EDGE('',*,*,#12770,.T.);
#16696=ORIENTED_EDGE('',*,*,#12769,.F.);
#16697=ORIENTED_EDGE('',*,*,#12770,.F.);
#16698=ORIENTED_EDGE('',*,*,#12771,.T.);
#16699=ORIENTED_EDGE('',*,*,#12772,.F.);
#16700=ORIENTED_EDGE('',*,*,#12771,.F.);
#16701=ORIENTED_EDGE('',*,*,#12773,.T.);
#16702=ORIENTED_EDGE('',*,*,#12774,.T.);
#16703=ORIENTED_EDGE('',*,*,#12775,.T.);
#16704=ORIENTED_EDGE('',*,*,#12776,.T.);
#16705=ORIENTED_EDGE('',*,*,#12774,.F.);
#16706=ORIENTED_EDGE('',*,*,#12777,.F.);
#16707=ORIENTED_EDGE('',*,*,#12778,.F.);
#16708=ORIENTED_EDGE('',*,*,#12779,.T.);
#16709=ORIENTED_EDGE('',*,*,#12775,.F.);
#16710=ORIENTED_EDGE('',*,*,#12776,.F.);
#16711=ORIENTED_EDGE('',*,*,#12779,.F.);
#16712=ORIENTED_EDGE('',*,*,#12780,.F.);
#16713=ORIENTED_EDGE('',*,*,#12640,.T.);
#16714=ORIENTED_EDGE('',*,*,#12646,.T.);
#16715=ORIENTED_EDGE('',*,*,#12652,.T.);
#16716=ORIENTED_EDGE('',*,*,#12773,.F.);
#16717=ORIENTED_EDGE('',*,*,#12777,.T.);
#16718=ORIENTED_EDGE('',*,*,#12778,.T.);
#16719=ORIENTED_EDGE('',*,*,#12781,.T.);
#16720=ORIENTED_EDGE('',*,*,#12782,.T.);
#16721=ORIENTED_EDGE('',*,*,#12781,.F.);
#16722=ORIENTED_EDGE('',*,*,#12783,.T.);
#16723=ORIENTED_EDGE('',*,*,#12782,.F.);
#16724=ORIENTED_EDGE('',*,*,#12784,.T.);
#16725=ORIENTED_EDGE('',*,*,#12785,.T.);
#16726=ORIENTED_EDGE('',*,*,#12786,.T.);
#16727=ORIENTED_EDGE('',*,*,#12787,.T.);
#16728=ORIENTED_EDGE('',*,*,#12786,.F.);
#16729=ORIENTED_EDGE('',*,*,#12788,.F.);
#16730=ORIENTED_EDGE('',*,*,#12789,.F.);
#16731=ORIENTED_EDGE('',*,*,#12790,.T.);
#16732=ORIENTED_EDGE('',*,*,#12784,.F.);
#16733=ORIENTED_EDGE('',*,*,#12785,.F.);
#16734=ORIENTED_EDGE('',*,*,#12790,.F.);
#16735=ORIENTED_EDGE('',*,*,#12787,.F.);
#16736=ORIENTED_EDGE('',*,*,#12663,.T.);
#16737=ORIENTED_EDGE('',*,*,#12683,.T.);
#16738=ORIENTED_EDGE('',*,*,#12703,.T.);
#16739=ORIENTED_EDGE('',*,*,#12713,.T.);
#16740=ORIENTED_EDGE('',*,*,#12723,.T.);
#16741=ORIENTED_EDGE('',*,*,#12733,.T.);
#16742=ORIENTED_EDGE('',*,*,#12743,.T.);
#16743=ORIENTED_EDGE('',*,*,#12753,.T.);
#16744=ORIENTED_EDGE('',*,*,#12763,.T.);
#16745=ORIENTED_EDGE('',*,*,#12791,.T.);
#16746=ORIENTED_EDGE('',*,*,#12693,.T.);
#16747=ORIENTED_EDGE('',*,*,#12673,.T.);
#16748=ORIENTED_EDGE('',*,*,#12653,.T.);
#16749=ORIENTED_EDGE('',*,*,#12792,.T.);
#16750=ORIENTED_EDGE('',*,*,#12793,.T.);
#16751=ORIENTED_EDGE('',*,*,#12788,.T.);
#16752=ORIENTED_EDGE('',*,*,#12789,.T.);
#16753=ORIENTED_EDGE('',*,*,#12793,.F.);
#16754=ORIENTED_EDGE('',*,*,#12792,.F.);
#16755=ORIENTED_EDGE('',*,*,#12634,.T.);
#16756=ORIENTED_EDGE('',*,*,#12672,.T.);
#16757=ORIENTED_EDGE('',*,*,#12692,.T.);
#16758=ORIENTED_EDGE('',*,*,#12712,.T.);
#16759=ORIENTED_EDGE('',*,*,#12732,.T.);
#16760=ORIENTED_EDGE('',*,*,#12752,.T.);
#16761=ORIENTED_EDGE('',*,*,#12772,.T.);
#16762=ORIENTED_EDGE('',*,*,#12794,.T.);
#16763=ORIENTED_EDGE('',*,*,#12795,.F.);
#16764=ORIENTED_EDGE('',*,*,#12796,.T.);
#16765=ORIENTED_EDGE('',*,*,#12797,.F.);
#16766=ORIENTED_EDGE('',*,*,#12798,.T.);
#16767=ORIENTED_EDGE('',*,*,#12799,.F.);
#16768=ORIENTED_EDGE('',*,*,#12800,.T.);
#16769=ORIENTED_EDGE('',*,*,#12801,.F.);
#16770=ORIENTED_EDGE('',*,*,#12802,.T.);
#16771=ORIENTED_EDGE('',*,*,#12803,.T.);
#16772=ORIENTED_EDGE('',*,*,#12804,.T.);
#16773=ORIENTED_EDGE('',*,*,#12805,.F.);
#16774=ORIENTED_EDGE('',*,*,#12806,.T.);
#16775=ORIENTED_EDGE('',*,*,#12807,.T.);
#16776=ORIENTED_EDGE('',*,*,#12808,.F.);
#16777=ORIENTED_EDGE('',*,*,#12809,.F.);
#16778=ORIENTED_EDGE('',*,*,#12810,.T.);
#16779=ORIENTED_EDGE('',*,*,#12811,.T.);
#16780=ORIENTED_EDGE('',*,*,#12812,.F.);
#16781=ORIENTED_EDGE('',*,*,#12813,.T.);
#16782=ORIENTED_EDGE('',*,*,#12814,.T.);
#16783=ORIENTED_EDGE('',*,*,#12815,.F.);
#16784=ORIENTED_EDGE('',*,*,#12816,.T.);
#16785=ORIENTED_EDGE('',*,*,#12817,.F.);
#16786=ORIENTED_EDGE('',*,*,#12818,.T.);
#16787=ORIENTED_EDGE('',*,*,#12819,.F.);
#16788=ORIENTED_EDGE('',*,*,#12820,.T.);
#16789=ORIENTED_EDGE('',*,*,#12821,.F.);
#16790=ORIENTED_EDGE('',*,*,#12822,.T.);
#16791=ORIENTED_EDGE('',*,*,#12823,.T.);
#16792=ORIENTED_EDGE('',*,*,#12824,.T.);
#16793=ORIENTED_EDGE('',*,*,#12825,.F.);
#16794=ORIENTED_EDGE('',*,*,#12826,.T.);
#16795=ORIENTED_EDGE('',*,*,#12827,.T.);
#16796=ORIENTED_EDGE('',*,*,#12828,.F.);
#16797=ORIENTED_EDGE('',*,*,#12829,.F.);
#16798=ORIENTED_EDGE('',*,*,#12830,.T.);
#16799=ORIENTED_EDGE('',*,*,#12831,.T.);
#16800=ORIENTED_EDGE('',*,*,#12832,.F.);
#16801=ORIENTED_EDGE('',*,*,#12833,.T.);
#16802=ORIENTED_EDGE('',*,*,#12834,.T.);
#16803=ORIENTED_EDGE('',*,*,#12835,.F.);
#16804=ORIENTED_EDGE('',*,*,#12836,.T.);
#16805=ORIENTED_EDGE('',*,*,#12837,.F.);
#16806=ORIENTED_EDGE('',*,*,#12838,.T.);
#16807=ORIENTED_EDGE('',*,*,#12839,.F.);
#16808=ORIENTED_EDGE('',*,*,#12840,.T.);
#16809=ORIENTED_EDGE('',*,*,#12841,.F.);
#16810=ORIENTED_EDGE('',*,*,#12842,.T.);
#16811=ORIENTED_EDGE('',*,*,#12843,.T.);
#16812=ORIENTED_EDGE('',*,*,#12844,.T.);
#16813=ORIENTED_EDGE('',*,*,#12845,.F.);
#16814=ORIENTED_EDGE('',*,*,#12846,.T.);
#16815=ORIENTED_EDGE('',*,*,#12847,.T.);
#16816=ORIENTED_EDGE('',*,*,#12848,.F.);
#16817=ORIENTED_EDGE('',*,*,#12849,.F.);
#16818=ORIENTED_EDGE('',*,*,#12850,.T.);
#16819=ORIENTED_EDGE('',*,*,#12851,.T.);
#16820=ORIENTED_EDGE('',*,*,#12852,.F.);
#16821=ORIENTED_EDGE('',*,*,#12853,.T.);
#16822=ORIENTED_EDGE('',*,*,#12854,.T.);
#16823=ORIENTED_EDGE('',*,*,#12855,.F.);
#16824=ORIENTED_EDGE('',*,*,#12856,.T.);
#16825=ORIENTED_EDGE('',*,*,#12857,.F.);
#16826=ORIENTED_EDGE('',*,*,#12858,.T.);
#16827=ORIENTED_EDGE('',*,*,#12859,.F.);
#16828=ORIENTED_EDGE('',*,*,#12860,.T.);
#16829=ORIENTED_EDGE('',*,*,#12861,.F.);
#16830=ORIENTED_EDGE('',*,*,#12862,.T.);
#16831=ORIENTED_EDGE('',*,*,#12863,.F.);
#16832=ORIENTED_EDGE('',*,*,#12864,.T.);
#16833=ORIENTED_EDGE('',*,*,#12865,.F.);
#16834=ORIENTED_EDGE('',*,*,#12866,.T.);
#16835=ORIENTED_EDGE('',*,*,#12867,.F.);
#16836=ORIENTED_EDGE('',*,*,#12868,.T.);
#16837=ORIENTED_EDGE('',*,*,#12869,.F.);
#16838=ORIENTED_EDGE('',*,*,#12870,.T.);
#16839=ORIENTED_EDGE('',*,*,#12871,.F.);
#16840=ORIENTED_EDGE('',*,*,#12872,.T.);
#16841=ORIENTED_EDGE('',*,*,#12873,.F.);
#16842=ORIENTED_EDGE('',*,*,#12874,.T.);
#16843=ORIENTED_EDGE('',*,*,#12875,.F.);
#16844=ORIENTED_EDGE('',*,*,#12876,.T.);
#16845=ORIENTED_EDGE('',*,*,#12877,.F.);
#16846=ORIENTED_EDGE('',*,*,#12878,.T.);
#16847=ORIENTED_EDGE('',*,*,#12879,.F.);
#16848=ORIENTED_EDGE('',*,*,#12880,.T.);
#16849=ORIENTED_EDGE('',*,*,#12881,.F.);
#16850=ORIENTED_EDGE('',*,*,#12882,.T.);
#16851=ORIENTED_EDGE('',*,*,#12883,.F.);
#16852=ORIENTED_EDGE('',*,*,#12884,.T.);
#16853=ORIENTED_EDGE('',*,*,#12885,.F.);
#16854=ORIENTED_EDGE('',*,*,#12886,.T.);
#16855=ORIENTED_EDGE('',*,*,#12887,.F.);
#16856=ORIENTED_EDGE('',*,*,#12888,.T.);
#16857=ORIENTED_EDGE('',*,*,#12889,.F.);
#16858=ORIENTED_EDGE('',*,*,#12890,.T.);
#16859=ORIENTED_EDGE('',*,*,#12891,.F.);
#16860=ORIENTED_EDGE('',*,*,#12892,.T.);
#16861=ORIENTED_EDGE('',*,*,#12893,.F.);
#16862=ORIENTED_EDGE('',*,*,#12894,.T.);
#16863=ORIENTED_EDGE('',*,*,#12895,.F.);
#16864=ORIENTED_EDGE('',*,*,#12896,.T.);
#16865=ORIENTED_EDGE('',*,*,#12897,.F.);
#16866=ORIENTED_EDGE('',*,*,#12898,.T.);
#16867=ORIENTED_EDGE('',*,*,#12899,.F.);
#16868=ORIENTED_EDGE('',*,*,#12900,.T.);
#16869=ORIENTED_EDGE('',*,*,#12901,.F.);
#16870=ORIENTED_EDGE('',*,*,#12902,.T.);
#16871=ORIENTED_EDGE('',*,*,#12903,.F.);
#16872=ORIENTED_EDGE('',*,*,#12904,.T.);
#16873=ORIENTED_EDGE('',*,*,#12905,.F.);
#16874=ORIENTED_EDGE('',*,*,#12906,.T.);
#16875=ORIENTED_EDGE('',*,*,#12907,.F.);
#16876=ORIENTED_EDGE('',*,*,#12908,.T.);
#16877=ORIENTED_EDGE('',*,*,#12909,.F.);
#16878=ORIENTED_EDGE('',*,*,#12910,.T.);
#16879=ORIENTED_EDGE('',*,*,#12911,.F.);
#16880=ORIENTED_EDGE('',*,*,#12912,.T.);
#16881=ORIENTED_EDGE('',*,*,#12913,.F.);
#16882=ORIENTED_EDGE('',*,*,#12914,.T.);
#16883=ORIENTED_EDGE('',*,*,#12915,.F.);
#16884=ORIENTED_EDGE('',*,*,#12916,.T.);
#16885=ORIENTED_EDGE('',*,*,#12917,.F.);
#16886=ORIENTED_EDGE('',*,*,#12918,.T.);
#16887=ORIENTED_EDGE('',*,*,#12919,.F.);
#16888=ORIENTED_EDGE('',*,*,#12920,.T.);
#16889=ORIENTED_EDGE('',*,*,#12921,.F.);
#16890=ORIENTED_EDGE('',*,*,#12922,.T.);
#16891=ORIENTED_EDGE('',*,*,#12923,.F.);
#16892=ORIENTED_EDGE('',*,*,#12924,.T.);
#16893=ORIENTED_EDGE('',*,*,#12925,.F.);
#16894=ORIENTED_EDGE('',*,*,#12926,.T.);
#16895=ORIENTED_EDGE('',*,*,#12927,.F.);
#16896=ORIENTED_EDGE('',*,*,#12928,.T.);
#16897=ORIENTED_EDGE('',*,*,#12929,.F.);
#16898=ORIENTED_EDGE('',*,*,#12930,.T.);
#16899=ORIENTED_EDGE('',*,*,#12931,.F.);
#16900=ORIENTED_EDGE('',*,*,#12932,.T.);
#16901=ORIENTED_EDGE('',*,*,#12933,.F.);
#16902=ORIENTED_EDGE('',*,*,#12934,.T.);
#16903=ORIENTED_EDGE('',*,*,#12935,.F.);
#16904=ORIENTED_EDGE('',*,*,#12936,.T.);
#16905=ORIENTED_EDGE('',*,*,#12937,.F.);
#16906=ORIENTED_EDGE('',*,*,#12938,.T.);
#16907=ORIENTED_EDGE('',*,*,#12939,.F.);
#16908=ORIENTED_EDGE('',*,*,#12940,.T.);
#16909=ORIENTED_EDGE('',*,*,#12941,.F.);
#16910=ORIENTED_EDGE('',*,*,#12942,.T.);
#16911=ORIENTED_EDGE('',*,*,#12943,.F.);
#16912=ORIENTED_EDGE('',*,*,#12944,.T.);
#16913=ORIENTED_EDGE('',*,*,#12945,.F.);
#16914=ORIENTED_EDGE('',*,*,#12946,.T.);
#16915=ORIENTED_EDGE('',*,*,#12947,.F.);
#16916=ORIENTED_EDGE('',*,*,#12948,.T.);
#16917=ORIENTED_EDGE('',*,*,#12949,.F.);
#16918=ORIENTED_EDGE('',*,*,#12950,.T.);
#16919=ORIENTED_EDGE('',*,*,#12951,.F.);
#16920=ORIENTED_EDGE('',*,*,#12952,.T.);
#16921=ORIENTED_EDGE('',*,*,#12953,.F.);
#16922=ORIENTED_EDGE('',*,*,#12954,.T.);
#16923=ORIENTED_EDGE('',*,*,#12955,.F.);
#16924=ORIENTED_EDGE('',*,*,#12956,.T.);
#16925=ORIENTED_EDGE('',*,*,#12957,.F.);
#16926=ORIENTED_EDGE('',*,*,#12958,.T.);
#16927=ORIENTED_EDGE('',*,*,#12959,.F.);
#16928=ORIENTED_EDGE('',*,*,#12960,.T.);
#16929=ORIENTED_EDGE('',*,*,#12961,.F.);
#16930=ORIENTED_EDGE('',*,*,#12962,.F.);
#16931=ORIENTED_EDGE('',*,*,#12762,.T.);
#16932=ORIENTED_EDGE('',*,*,#12742,.T.);
#16933=ORIENTED_EDGE('',*,*,#12722,.T.);
#16934=ORIENTED_EDGE('',*,*,#12702,.T.);
#16935=ORIENTED_EDGE('',*,*,#12682,.T.);
#16936=ORIENTED_EDGE('',*,*,#12662,.T.);
#16937=ORIENTED_EDGE('',*,*,#12628,.T.);
#16938=ORIENTED_EDGE('',*,*,#12847,.F.);
#16939=ORIENTED_EDGE('',*,*,#12963,.T.);
#16940=ORIENTED_EDGE('',*,*,#12964,.F.);
#16941=ORIENTED_EDGE('',*,*,#12965,.T.);
#16942=ORIENTED_EDGE('',*,*,#12966,.F.);
#16943=ORIENTED_EDGE('',*,*,#12967,.T.);
#16944=ORIENTED_EDGE('',*,*,#12852,.T.);
#16945=ORIENTED_EDGE('',*,*,#12968,.T.);
#16946=ORIENTED_EDGE('',*,*,#12967,.F.);
#16947=ORIENTED_EDGE('',*,*,#12969,.T.);
#16948=ORIENTED_EDGE('',*,*,#12970,.T.);
#16949=ORIENTED_EDGE('',*,*,#12853,.F.);
#16950=ORIENTED_EDGE('',*,*,#12971,.F.);
#16951=ORIENTED_EDGE('',*,*,#12972,.T.);
#16952=ORIENTED_EDGE('',*,*,#12850,.F.);
#16953=ORIENTED_EDGE('',*,*,#12973,.T.);
#16954=ORIENTED_EDGE('',*,*,#12966,.T.);
#16955=ORIENTED_EDGE('',*,*,#12974,.F.);
#16956=ORIENTED_EDGE('',*,*,#12971,.T.);
#16957=ORIENTED_EDGE('',*,*,#12975,.T.);
#16958=ORIENTED_EDGE('',*,*,#12969,.F.);
#16959=ORIENTED_EDGE('',*,*,#12976,.F.);
#16960=ORIENTED_EDGE('',*,*,#12977,.T.);
#16961=ORIENTED_EDGE('',*,*,#12959,.T.);
#16962=ORIENTED_EDGE('',*,*,#12978,.T.);
#16963=ORIENTED_EDGE('',*,*,#12977,.F.);
#16964=ORIENTED_EDGE('',*,*,#12979,.T.);
#16965=ORIENTED_EDGE('',*,*,#12980,.F.);
#16966=ORIENTED_EDGE('',*,*,#12960,.F.);
#16967=ORIENTED_EDGE('',*,*,#12981,.F.);
#16968=ORIENTED_EDGE('',*,*,#12982,.T.);
#16969=ORIENTED_EDGE('',*,*,#12957,.T.);
#16970=ORIENTED_EDGE('',*,*,#12983,.T.);
#16971=ORIENTED_EDGE('',*,*,#12976,.T.);
#16972=ORIENTED_EDGE('',*,*,#12984,.F.);
#16973=ORIENTED_EDGE('',*,*,#12981,.T.);
#16974=ORIENTED_EDGE('',*,*,#12985,.F.);
#16975=ORIENTED_EDGE('',*,*,#12986,.T.);
#16976=ORIENTED_EDGE('',*,*,#12979,.F.);
#16977=ORIENTED_EDGE('',*,*,#12983,.F.);
#16978=ORIENTED_EDGE('',*,*,#12956,.F.);
#16979=ORIENTED_EDGE('',*,*,#12987,.F.);
#16980=ORIENTED_EDGE('',*,*,#12985,.T.);
#16981=ORIENTED_EDGE('',*,*,#12986,.F.);
#16982=ORIENTED_EDGE('',*,*,#12987,.T.);
#16983=ORIENTED_EDGE('',*,*,#12961,.T.);
#16984=ORIENTED_EDGE('',*,*,#12980,.T.);
#16985=ORIENTED_EDGE('',*,*,#12988,.F.);
#16986=ORIENTED_EDGE('',*,*,#12989,.T.);
#16987=ORIENTED_EDGE('',*,*,#12953,.T.);
#16988=ORIENTED_EDGE('',*,*,#12990,.T.);
#16989=ORIENTED_EDGE('',*,*,#12989,.F.);
#16990=ORIENTED_EDGE('',*,*,#12991,.T.);
#16991=ORIENTED_EDGE('',*,*,#12992,.F.);
#16992=ORIENTED_EDGE('',*,*,#12954,.F.);
#16993=ORIENTED_EDGE('',*,*,#12993,.F.);
#16994=ORIENTED_EDGE('',*,*,#12994,.T.);
#16995=ORIENTED_EDGE('',*,*,#12951,.T.);
#16996=ORIENTED_EDGE('',*,*,#12995,.T.);
#16997=ORIENTED_EDGE('',*,*,#12988,.T.);
#16998=ORIENTED_EDGE('',*,*,#12996,.F.);
#16999=ORIENTED_EDGE('',*,*,#12993,.T.);
#17000=ORIENTED_EDGE('',*,*,#12997,.F.);
#17001=ORIENTED_EDGE('',*,*,#12998,.T.);
#17002=ORIENTED_EDGE('',*,*,#12991,.F.);
#17003=ORIENTED_EDGE('',*,*,#12995,.F.);
#17004=ORIENTED_EDGE('',*,*,#12950,.F.);
#17005=ORIENTED_EDGE('',*,*,#12999,.F.);
#17006=ORIENTED_EDGE('',*,*,#12997,.T.);
#17007=ORIENTED_EDGE('',*,*,#12998,.F.);
#17008=ORIENTED_EDGE('',*,*,#12999,.T.);
#17009=ORIENTED_EDGE('',*,*,#12955,.T.);
#17010=ORIENTED_EDGE('',*,*,#12992,.T.);
#17011=ORIENTED_EDGE('',*,*,#12827,.F.);
#17012=ORIENTED_EDGE('',*,*,#13000,.T.);
#17013=ORIENTED_EDGE('',*,*,#13001,.F.);
#17014=ORIENTED_EDGE('',*,*,#13002,.T.);
#17015=ORIENTED_EDGE('',*,*,#13003,.F.);
#17016=ORIENTED_EDGE('',*,*,#13004,.T.);
#17017=ORIENTED_EDGE('',*,*,#12947,.T.);
#17018=ORIENTED_EDGE('',*,*,#13005,.T.);
#17019=ORIENTED_EDGE('',*,*,#13004,.F.);
#17020=ORIENTED_EDGE('',*,*,#13006,.T.);
#17021=ORIENTED_EDGE('',*,*,#13007,.F.);
#17022=ORIENTED_EDGE('',*,*,#12948,.F.);
#17023=ORIENTED_EDGE('',*,*,#13008,.F.);
#17024=ORIENTED_EDGE('',*,*,#13009,.T.);
#17025=ORIENTED_EDGE('',*,*,#12945,.T.);
#17026=ORIENTED_EDGE('',*,*,#13010,.T.);
#17027=ORIENTED_EDGE('',*,*,#13003,.T.);
#17028=ORIENTED_EDGE('',*,*,#13011,.F.);
#17029=ORIENTED_EDGE('',*,*,#13008,.T.);
#17030=ORIENTED_EDGE('',*,*,#13012,.F.);
#17031=ORIENTED_EDGE('',*,*,#13013,.T.);
#17032=ORIENTED_EDGE('',*,*,#13006,.F.);
#17033=ORIENTED_EDGE('',*,*,#13010,.F.);
#17034=ORIENTED_EDGE('',*,*,#12944,.F.);
#17035=ORIENTED_EDGE('',*,*,#13014,.F.);
#17036=ORIENTED_EDGE('',*,*,#13012,.T.);
#17037=ORIENTED_EDGE('',*,*,#13013,.F.);
#17038=ORIENTED_EDGE('',*,*,#13014,.T.);
#17039=ORIENTED_EDGE('',*,*,#12949,.T.);
#17040=ORIENTED_EDGE('',*,*,#13007,.T.);
#17041=ORIENTED_EDGE('',*,*,#13015,.F.);
#17042=ORIENTED_EDGE('',*,*,#13016,.T.);
#17043=ORIENTED_EDGE('',*,*,#12941,.T.);
#17044=ORIENTED_EDGE('',*,*,#13017,.T.);
#17045=ORIENTED_EDGE('',*,*,#13016,.F.);
#17046=ORIENTED_EDGE('',*,*,#13018,.T.);
#17047=ORIENTED_EDGE('',*,*,#13019,.F.);
#17048=ORIENTED_EDGE('',*,*,#12942,.F.);
#17049=ORIENTED_EDGE('',*,*,#13020,.F.);
#17050=ORIENTED_EDGE('',*,*,#13021,.T.);
#17051=ORIENTED_EDGE('',*,*,#12939,.T.);
#17052=ORIENTED_EDGE('',*,*,#13022,.T.);
#17053=ORIENTED_EDGE('',*,*,#13015,.T.);
#17054=ORIENTED_EDGE('',*,*,#13023,.F.);
#17055=ORIENTED_EDGE('',*,*,#13020,.T.);
#17056=ORIENTED_EDGE('',*,*,#13024,.F.);
#17057=ORIENTED_EDGE('',*,*,#13025,.T.);
#17058=ORIENTED_EDGE('',*,*,#13018,.F.);
#17059=ORIENTED_EDGE('',*,*,#13022,.F.);
#17060=ORIENTED_EDGE('',*,*,#12938,.F.);
#17061=ORIENTED_EDGE('',*,*,#13026,.F.);
#17062=ORIENTED_EDGE('',*,*,#13024,.T.);
#17063=ORIENTED_EDGE('',*,*,#13025,.F.);
#17064=ORIENTED_EDGE('',*,*,#13026,.T.);
#17065=ORIENTED_EDGE('',*,*,#12943,.T.);
#17066=ORIENTED_EDGE('',*,*,#13019,.T.);
#17067=ORIENTED_EDGE('',*,*,#13027,.F.);
#17068=ORIENTED_EDGE('',*,*,#13028,.T.);
#17069=ORIENTED_EDGE('',*,*,#12815,.T.);
#17070=ORIENTED_EDGE('',*,*,#13029,.T.);
#17071=ORIENTED_EDGE('',*,*,#13028,.F.);
#17072=ORIENTED_EDGE('',*,*,#13030,.T.);
#17073=ORIENTED_EDGE('',*,*,#13031,.T.);
#17074=ORIENTED_EDGE('',*,*,#12816,.F.);
#17075=ORIENTED_EDGE('',*,*,#13032,.F.);
#17076=ORIENTED_EDGE('',*,*,#13033,.T.);
#17077=ORIENTED_EDGE('',*,*,#12832,.T.);
#17078=ORIENTED_EDGE('',*,*,#13034,.T.);
#17079=ORIENTED_EDGE('',*,*,#13032,.T.);
#17080=ORIENTED_EDGE('',*,*,#13035,.F.);
#17081=ORIENTED_EDGE('',*,*,#13036,.T.);
#17082=ORIENTED_EDGE('',*,*,#13037,.T.);
#17083=ORIENTED_EDGE('',*,*,#13038,.F.);
#17084=ORIENTED_EDGE('',*,*,#13034,.F.);
#17085=ORIENTED_EDGE('',*,*,#12831,.F.);
#17086=ORIENTED_EDGE('',*,*,#13039,.F.);
#17087=ORIENTED_EDGE('',*,*,#13035,.T.);
#17088=ORIENTED_EDGE('',*,*,#13036,.F.);
#17089=ORIENTED_EDGE('',*,*,#13039,.T.);
#17090=ORIENTED_EDGE('',*,*,#12830,.F.);
#17091=ORIENTED_EDGE('',*,*,#13040,.T.);
#17092=ORIENTED_EDGE('',*,*,#13041,.F.);
#17093=ORIENTED_EDGE('',*,*,#13042,.T.);
#17094=ORIENTED_EDGE('',*,*,#12935,.T.);
#17095=ORIENTED_EDGE('',*,*,#13043,.T.);
#17096=ORIENTED_EDGE('',*,*,#13042,.F.);
#17097=ORIENTED_EDGE('',*,*,#13044,.T.);
#17098=ORIENTED_EDGE('',*,*,#13045,.F.);
#17099=ORIENTED_EDGE('',*,*,#12936,.F.);
#17100=ORIENTED_EDGE('',*,*,#13046,.F.);
#17101=ORIENTED_EDGE('',*,*,#13047,.T.);
#17102=ORIENTED_EDGE('',*,*,#12933,.T.);
#17103=ORIENTED_EDGE('',*,*,#13048,.T.);
#17104=ORIENTED_EDGE('',*,*,#13041,.T.);
#17105=ORIENTED_EDGE('',*,*,#13049,.F.);
#17106=ORIENTED_EDGE('',*,*,#13046,.T.);
#17107=ORIENTED_EDGE('',*,*,#13050,.F.);
#17108=ORIENTED_EDGE('',*,*,#13051,.T.);
#17109=ORIENTED_EDGE('',*,*,#13044,.F.);
#17110=ORIENTED_EDGE('',*,*,#13048,.F.);
#17111=ORIENTED_EDGE('',*,*,#12932,.F.);
#17112=ORIENTED_EDGE('',*,*,#13052,.F.);
#17113=ORIENTED_EDGE('',*,*,#13050,.T.);
#17114=ORIENTED_EDGE('',*,*,#13051,.F.);
#17115=ORIENTED_EDGE('',*,*,#13052,.T.);
#17116=ORIENTED_EDGE('',*,*,#12937,.T.);
#17117=ORIENTED_EDGE('',*,*,#13045,.T.);
#17118=ORIENTED_EDGE('',*,*,#13053,.F.);
#17119=ORIENTED_EDGE('',*,*,#13054,.T.);
#17120=ORIENTED_EDGE('',*,*,#12929,.T.);
#17121=ORIENTED_EDGE('',*,*,#13055,.T.);
#17122=ORIENTED_EDGE('',*,*,#13054,.F.);
#17123=ORIENTED_EDGE('',*,*,#13056,.T.);
#17124=ORIENTED_EDGE('',*,*,#13057,.F.);
#17125=ORIENTED_EDGE('',*,*,#12930,.F.);
#17126=ORIENTED_EDGE('',*,*,#13058,.F.);
#17127=ORIENTED_EDGE('',*,*,#13059,.T.);
#17128=ORIENTED_EDGE('',*,*,#12927,.T.);
#17129=ORIENTED_EDGE('',*,*,#13060,.T.);
#17130=ORIENTED_EDGE('',*,*,#13053,.T.);
#17131=ORIENTED_EDGE('',*,*,#13061,.F.);
#17132=ORIENTED_EDGE('',*,*,#13058,.T.);
#17133=ORIENTED_EDGE('',*,*,#13062,.F.);
#17134=ORIENTED_EDGE('',*,*,#13063,.T.);
#17135=ORIENTED_EDGE('',*,*,#13056,.F.);
#17136=ORIENTED_EDGE('',*,*,#13060,.F.);
#17137=ORIENTED_EDGE('',*,*,#12926,.F.);
#17138=ORIENTED_EDGE('',*,*,#13064,.F.);
#17139=ORIENTED_EDGE('',*,*,#13062,.T.);
#17140=ORIENTED_EDGE('',*,*,#13063,.F.);
#17141=ORIENTED_EDGE('',*,*,#13064,.T.);
#17142=ORIENTED_EDGE('',*,*,#12931,.T.);
#17143=ORIENTED_EDGE('',*,*,#13057,.T.);
#17144=ORIENTED_EDGE('',*,*,#12823,.F.);
#17145=ORIENTED_EDGE('',*,*,#13065,.T.);
#17146=ORIENTED_EDGE('',*,*,#13066,.F.);
#17147=ORIENTED_EDGE('',*,*,#13067,.T.);
#17148=ORIENTED_EDGE('',*,*,#13066,.T.);
#17149=ORIENTED_EDGE('',*,*,#13068,.F.);
#17150=ORIENTED_EDGE('',*,*,#13069,.T.);
#17151=ORIENTED_EDGE('',*,*,#13070,.F.);
#17152=ORIENTED_EDGE('',*,*,#13071,.T.);
#17153=ORIENTED_EDGE('',*,*,#13065,.F.);
#17154=ORIENTED_EDGE('',*,*,#12822,.F.);
#17155=ORIENTED_EDGE('',*,*,#13072,.F.);
#17156=ORIENTED_EDGE('',*,*,#13068,.T.);
#17157=ORIENTED_EDGE('',*,*,#13069,.F.);
#17158=ORIENTED_EDGE('',*,*,#13072,.T.);
#17159=ORIENTED_EDGE('',*,*,#12821,.T.);
#17160=ORIENTED_EDGE('',*,*,#13073,.T.);
#17161=ORIENTED_EDGE('',*,*,#13073,.F.);
#17162=ORIENTED_EDGE('',*,*,#12820,.F.);
#17163=ORIENTED_EDGE('',*,*,#13074,.T.);
#17164=ORIENTED_EDGE('',*,*,#13070,.T.);
#17165=ORIENTED_EDGE('',*,*,#13075,.F.);
#17166=ORIENTED_EDGE('',*,*,#13076,.T.);
#17167=ORIENTED_EDGE('',*,*,#12923,.T.);
#17168=ORIENTED_EDGE('',*,*,#13077,.T.);
#17169=ORIENTED_EDGE('',*,*,#13076,.F.);
#17170=ORIENTED_EDGE('',*,*,#13078,.T.);
#17171=ORIENTED_EDGE('',*,*,#13079,.F.);
#17172=ORIENTED_EDGE('',*,*,#12924,.F.);
#17173=ORIENTED_EDGE('',*,*,#13080,.F.);
#17174=ORIENTED_EDGE('',*,*,#13081,.T.);
#17175=ORIENTED_EDGE('',*,*,#12921,.T.);
#17176=ORIENTED_EDGE('',*,*,#13082,.T.);
#17177=ORIENTED_EDGE('',*,*,#13075,.T.);
#17178=ORIENTED_EDGE('',*,*,#13083,.F.);
#17179=ORIENTED_EDGE('',*,*,#13080,.T.);
#17180=ORIENTED_EDGE('',*,*,#13084,.F.);
#17181=ORIENTED_EDGE('',*,*,#13085,.T.);
#17182=ORIENTED_EDGE('',*,*,#13078,.F.);
#17183=ORIENTED_EDGE('',*,*,#13082,.F.);
#17184=ORIENTED_EDGE('',*,*,#12920,.F.);
#17185=ORIENTED_EDGE('',*,*,#13086,.F.);
#17186=ORIENTED_EDGE('',*,*,#13084,.T.);
#17187=ORIENTED_EDGE('',*,*,#13085,.F.);
#17188=ORIENTED_EDGE('',*,*,#13086,.T.);
#17189=ORIENTED_EDGE('',*,*,#12925,.T.);
#17190=ORIENTED_EDGE('',*,*,#13079,.T.);
#17191=ORIENTED_EDGE('',*,*,#13087,.F.);
#17192=ORIENTED_EDGE('',*,*,#13088,.T.);
#17193=ORIENTED_EDGE('',*,*,#12917,.T.);
#17194=ORIENTED_EDGE('',*,*,#13089,.T.);
#17195=ORIENTED_EDGE('',*,*,#13088,.F.);
#17196=ORIENTED_EDGE('',*,*,#13090,.T.);
#17197=ORIENTED_EDGE('',*,*,#13091,.F.);
#17198=ORIENTED_EDGE('',*,*,#12918,.F.);
#17199=ORIENTED_EDGE('',*,*,#13092,.F.);
#17200=ORIENTED_EDGE('',*,*,#13093,.T.);
#17201=ORIENTED_EDGE('',*,*,#12915,.T.);
#17202=ORIENTED_EDGE('',*,*,#13094,.T.);
#17203=ORIENTED_EDGE('',*,*,#13087,.T.);
#17204=ORIENTED_EDGE('',*,*,#13095,.F.);
#17205=ORIENTED_EDGE('',*,*,#13092,.T.);
#17206=ORIENTED_EDGE('',*,*,#13096,.F.);
#17207=ORIENTED_EDGE('',*,*,#13097,.T.);
#17208=ORIENTED_EDGE('',*,*,#13090,.F.);
#17209=ORIENTED_EDGE('',*,*,#13094,.F.);
#17210=ORIENTED_EDGE('',*,*,#12914,.F.);
#17211=ORIENTED_EDGE('',*,*,#13098,.F.);
#17212=ORIENTED_EDGE('',*,*,#13096,.T.);
#17213=ORIENTED_EDGE('',*,*,#13097,.F.);
#17214=ORIENTED_EDGE('',*,*,#13098,.T.);
#17215=ORIENTED_EDGE('',*,*,#12919,.T.);
#17216=ORIENTED_EDGE('',*,*,#13091,.T.);
#17217=ORIENTED_EDGE('',*,*,#13099,.F.);
#17218=ORIENTED_EDGE('',*,*,#13100,.T.);
#17219=ORIENTED_EDGE('',*,*,#12795,.T.);
#17220=ORIENTED_EDGE('',*,*,#13101,.T.);
#17221=ORIENTED_EDGE('',*,*,#13100,.F.);
#17222=ORIENTED_EDGE('',*,*,#13102,.T.);
#17223=ORIENTED_EDGE('',*,*,#13103,.T.);
#17224=ORIENTED_EDGE('',*,*,#12796,.F.);
#17225=ORIENTED_EDGE('',*,*,#13104,.F.);
#17226=ORIENTED_EDGE('',*,*,#13105,.T.);
#17227=ORIENTED_EDGE('',*,*,#12812,.T.);
#17228=ORIENTED_EDGE('',*,*,#13106,.T.);
#17229=ORIENTED_EDGE('',*,*,#13104,.T.);
#17230=ORIENTED_EDGE('',*,*,#13107,.F.);
#17231=ORIENTED_EDGE('',*,*,#13108,.T.);
#17232=ORIENTED_EDGE('',*,*,#13109,.T.);
#17233=ORIENTED_EDGE('',*,*,#13110,.F.);
#17234=ORIENTED_EDGE('',*,*,#13106,.F.);
#17235=ORIENTED_EDGE('',*,*,#12811,.F.);
#17236=ORIENTED_EDGE('',*,*,#13111,.F.);
#17237=ORIENTED_EDGE('',*,*,#13107,.T.);
#17238=ORIENTED_EDGE('',*,*,#13108,.F.);
#17239=ORIENTED_EDGE('',*,*,#13111,.T.);
#17240=ORIENTED_EDGE('',*,*,#12810,.F.);
#17241=ORIENTED_EDGE('',*,*,#13112,.T.);
#17242=ORIENTED_EDGE('',*,*,#13113,.F.);
#17243=ORIENTED_EDGE('',*,*,#13114,.T.);
#17244=ORIENTED_EDGE('',*,*,#12911,.T.);
#17245=ORIENTED_EDGE('',*,*,#13115,.T.);
#17246=ORIENTED_EDGE('',*,*,#13114,.F.);
#17247=ORIENTED_EDGE('',*,*,#13116,.T.);
#17248=ORIENTED_EDGE('',*,*,#13117,.F.);
#17249=ORIENTED_EDGE('',*,*,#12912,.F.);
#17250=ORIENTED_EDGE('',*,*,#13118,.F.);
#17251=ORIENTED_EDGE('',*,*,#13119,.T.);
#17252=ORIENTED_EDGE('',*,*,#12909,.T.);
#17253=ORIENTED_EDGE('',*,*,#13120,.T.);
#17254=ORIENTED_EDGE('',*,*,#13113,.T.);
#17255=ORIENTED_EDGE('',*,*,#13121,.F.);
#17256=ORIENTED_EDGE('',*,*,#13118,.T.);
#17257=ORIENTED_EDGE('',*,*,#13122,.F.);
#17258=ORIENTED_EDGE('',*,*,#13123,.T.);
#17259=ORIENTED_EDGE('',*,*,#13116,.F.);
#17260=ORIENTED_EDGE('',*,*,#13120,.F.);
#17261=ORIENTED_EDGE('',*,*,#12908,.F.);
#17262=ORIENTED_EDGE('',*,*,#13124,.F.);
#17263=ORIENTED_EDGE('',*,*,#13122,.T.);
#17264=ORIENTED_EDGE('',*,*,#13123,.F.);
#17265=ORIENTED_EDGE('',*,*,#13124,.T.);
#17266=ORIENTED_EDGE('',*,*,#12913,.T.);
#17267=ORIENTED_EDGE('',*,*,#13117,.T.);
#17268=ORIENTED_EDGE('',*,*,#13125,.F.);
#17269=ORIENTED_EDGE('',*,*,#13126,.T.);
#17270=ORIENTED_EDGE('',*,*,#12905,.T.);
#17271=ORIENTED_EDGE('',*,*,#13127,.T.);
#17272=ORIENTED_EDGE('',*,*,#13126,.F.);
#17273=ORIENTED_EDGE('',*,*,#13128,.T.);
#17274=ORIENTED_EDGE('',*,*,#13129,.F.);
#17275=ORIENTED_EDGE('',*,*,#12906,.F.);
#17276=ORIENTED_EDGE('',*,*,#13130,.F.);
#17277=ORIENTED_EDGE('',*,*,#13131,.T.);
#17278=ORIENTED_EDGE('',*,*,#12903,.T.);
#17279=ORIENTED_EDGE('',*,*,#13132,.T.);
#17280=ORIENTED_EDGE('',*,*,#13125,.T.);
#17281=ORIENTED_EDGE('',*,*,#13133,.F.);
#17282=ORIENTED_EDGE('',*,*,#13130,.T.);
#17283=ORIENTED_EDGE('',*,*,#13134,.F.);
#17284=ORIENTED_EDGE('',*,*,#13135,.T.);
#17285=ORIENTED_EDGE('',*,*,#13128,.F.);
#17286=ORIENTED_EDGE('',*,*,#13132,.F.);
#17287=ORIENTED_EDGE('',*,*,#12902,.F.);
#17288=ORIENTED_EDGE('',*,*,#13136,.F.);
#17289=ORIENTED_EDGE('',*,*,#13134,.T.);
#17290=ORIENTED_EDGE('',*,*,#13135,.F.);
#17291=ORIENTED_EDGE('',*,*,#13136,.T.);
#17292=ORIENTED_EDGE('',*,*,#12907,.T.);
#17293=ORIENTED_EDGE('',*,*,#13129,.T.);
#17294=ORIENTED_EDGE('',*,*,#13137,.F.);
#17295=ORIENTED_EDGE('',*,*,#13138,.T.);
#17296=ORIENTED_EDGE('',*,*,#12899,.T.);
#17297=ORIENTED_EDGE('',*,*,#13139,.T.);
#17298=ORIENTED_EDGE('',*,*,#13138,.F.);
#17299=ORIENTED_EDGE('',*,*,#13140,.T.);
#17300=ORIENTED_EDGE('',*,*,#13141,.F.);
#17301=ORIENTED_EDGE('',*,*,#12900,.F.);
#17302=ORIENTED_EDGE('',*,*,#13142,.F.);
#17303=ORIENTED_EDGE('',*,*,#13143,.T.);
#17304=ORIENTED_EDGE('',*,*,#12897,.T.);
#17305=ORIENTED_EDGE('',*,*,#13144,.T.);
#17306=ORIENTED_EDGE('',*,*,#13137,.T.);
#17307=ORIENTED_EDGE('',*,*,#13145,.F.);
#17308=ORIENTED_EDGE('',*,*,#13142,.T.);
#17309=ORIENTED_EDGE('',*,*,#13146,.F.);
#17310=ORIENTED_EDGE('',*,*,#13147,.T.);
#17311=ORIENTED_EDGE('',*,*,#13140,.F.);
#17312=ORIENTED_EDGE('',*,*,#13144,.F.);
#17313=ORIENTED_EDGE('',*,*,#12896,.F.);
#17314=ORIENTED_EDGE('',*,*,#13148,.F.);
#17315=ORIENTED_EDGE('',*,*,#13146,.T.);
#17316=ORIENTED_EDGE('',*,*,#13147,.F.);
#17317=ORIENTED_EDGE('',*,*,#13148,.T.);
#17318=ORIENTED_EDGE('',*,*,#12901,.T.);
#17319=ORIENTED_EDGE('',*,*,#13141,.T.);
#17320=ORIENTED_EDGE('',*,*,#12807,.F.);
#17321=ORIENTED_EDGE('',*,*,#13149,.T.);
#17322=ORIENTED_EDGE('',*,*,#13150,.F.);
#17323=ORIENTED_EDGE('',*,*,#13151,.T.);
#17324=ORIENTED_EDGE('',*,*,#13152,.F.);
#17325=ORIENTED_EDGE('',*,*,#13153,.T.);
#17326=ORIENTED_EDGE('',*,*,#12893,.T.);
#17327=ORIENTED_EDGE('',*,*,#13154,.T.);
#17328=ORIENTED_EDGE('',*,*,#13153,.F.);
#17329=ORIENTED_EDGE('',*,*,#13155,.T.);
#17330=ORIENTED_EDGE('',*,*,#13156,.F.);
#17331=ORIENTED_EDGE('',*,*,#12894,.F.);
#17332=ORIENTED_EDGE('',*,*,#13157,.F.);
#17333=ORIENTED_EDGE('',*,*,#13158,.T.);
#17334=ORIENTED_EDGE('',*,*,#12891,.T.);
#17335=ORIENTED_EDGE('',*,*,#13159,.T.);
#17336=ORIENTED_EDGE('',*,*,#13152,.T.);
#17337=ORIENTED_EDGE('',*,*,#13160,.F.);
#17338=ORIENTED_EDGE('',*,*,#13157,.T.);
#17339=ORIENTED_EDGE('',*,*,#13161,.F.);
#17340=ORIENTED_EDGE('',*,*,#13162,.T.);
#17341=ORIENTED_EDGE('',*,*,#13155,.F.);
#17342=ORIENTED_EDGE('',*,*,#13159,.F.);
#17343=ORIENTED_EDGE('',*,*,#12890,.F.);
#17344=ORIENTED_EDGE('',*,*,#13163,.F.);
#17345=ORIENTED_EDGE('',*,*,#13161,.T.);
#17346=ORIENTED_EDGE('',*,*,#13162,.F.);
#17347=ORIENTED_EDGE('',*,*,#13163,.T.);
#17348=ORIENTED_EDGE('',*,*,#12895,.T.);
#17349=ORIENTED_EDGE('',*,*,#13156,.T.);
#17350=ORIENTED_EDGE('',*,*,#13164,.F.);
#17351=ORIENTED_EDGE('',*,*,#13165,.T.);
#17352=ORIENTED_EDGE('',*,*,#12887,.T.);
#17353=ORIENTED_EDGE('',*,*,#13166,.T.);
#17354=ORIENTED_EDGE('',*,*,#13165,.F.);
#17355=ORIENTED_EDGE('',*,*,#13167,.T.);
#17356=ORIENTED_EDGE('',*,*,#13168,.F.);
#17357=ORIENTED_EDGE('',*,*,#12888,.F.);
#17358=ORIENTED_EDGE('',*,*,#13169,.F.);
#17359=ORIENTED_EDGE('',*,*,#13170,.T.);
#17360=ORIENTED_EDGE('',*,*,#12885,.T.);
#17361=ORIENTED_EDGE('',*,*,#13171,.T.);
#17362=ORIENTED_EDGE('',*,*,#13164,.T.);
#17363=ORIENTED_EDGE('',*,*,#13172,.F.);
#17364=ORIENTED_EDGE('',*,*,#13169,.T.);
#17365=ORIENTED_EDGE('',*,*,#13173,.F.);
#17366=ORIENTED_EDGE('',*,*,#13174,.T.);
#17367=ORIENTED_EDGE('',*,*,#13167,.F.);
#17368=ORIENTED_EDGE('',*,*,#13171,.F.);
#17369=ORIENTED_EDGE('',*,*,#12884,.F.);
#17370=ORIENTED_EDGE('',*,*,#13175,.F.);
#17371=ORIENTED_EDGE('',*,*,#13173,.T.);
#17372=ORIENTED_EDGE('',*,*,#13174,.F.);
#17373=ORIENTED_EDGE('',*,*,#13175,.T.);
#17374=ORIENTED_EDGE('',*,*,#12889,.T.);
#17375=ORIENTED_EDGE('',*,*,#13168,.T.);
#17376=ORIENTED_EDGE('',*,*,#12803,.F.);
#17377=ORIENTED_EDGE('',*,*,#13176,.T.);
#17378=ORIENTED_EDGE('',*,*,#13177,.F.);
#17379=ORIENTED_EDGE('',*,*,#13178,.T.);
#17380=ORIENTED_EDGE('',*,*,#13177,.T.);
#17381=ORIENTED_EDGE('',*,*,#13179,.F.);
#17382=ORIENTED_EDGE('',*,*,#13180,.T.);
#17383=ORIENTED_EDGE('',*,*,#13181,.F.);
#17384=ORIENTED_EDGE('',*,*,#13182,.T.);
#17385=ORIENTED_EDGE('',*,*,#13176,.F.);
#17386=ORIENTED_EDGE('',*,*,#12802,.F.);
#17387=ORIENTED_EDGE('',*,*,#13183,.F.);
#17388=ORIENTED_EDGE('',*,*,#13179,.T.);
#17389=ORIENTED_EDGE('',*,*,#13180,.F.);
#17390=ORIENTED_EDGE('',*,*,#13183,.T.);
#17391=ORIENTED_EDGE('',*,*,#12801,.T.);
#17392=ORIENTED_EDGE('',*,*,#13184,.T.);
#17393=ORIENTED_EDGE('',*,*,#13184,.F.);
#17394=ORIENTED_EDGE('',*,*,#12800,.F.);
#17395=ORIENTED_EDGE('',*,*,#13185,.T.);
#17396=ORIENTED_EDGE('',*,*,#13181,.T.);
#17397=ORIENTED_EDGE('',*,*,#13186,.F.);
#17398=ORIENTED_EDGE('',*,*,#13187,.T.);
#17399=ORIENTED_EDGE('',*,*,#12881,.T.);
#17400=ORIENTED_EDGE('',*,*,#13188,.T.);
#17401=ORIENTED_EDGE('',*,*,#13187,.F.);
#17402=ORIENTED_EDGE('',*,*,#13189,.T.);
#17403=ORIENTED_EDGE('',*,*,#13190,.F.);
#17404=ORIENTED_EDGE('',*,*,#12882,.F.);
#17405=ORIENTED_EDGE('',*,*,#13191,.F.);
#17406=ORIENTED_EDGE('',*,*,#13192,.T.);
#17407=ORIENTED_EDGE('',*,*,#12879,.T.);
#17408=ORIENTED_EDGE('',*,*,#13193,.T.);
#17409=ORIENTED_EDGE('',*,*,#13186,.T.);
#17410=ORIENTED_EDGE('',*,*,#13194,.F.);
#17411=ORIENTED_EDGE('',*,*,#13191,.T.);
#17412=ORIENTED_EDGE('',*,*,#13195,.F.);
#17413=ORIENTED_EDGE('',*,*,#13196,.T.);
#17414=ORIENTED_EDGE('',*,*,#13189,.F.);
#17415=ORIENTED_EDGE('',*,*,#13193,.F.);
#17416=ORIENTED_EDGE('',*,*,#12878,.F.);
#17417=ORIENTED_EDGE('',*,*,#13197,.F.);
#17418=ORIENTED_EDGE('',*,*,#13195,.T.);
#17419=ORIENTED_EDGE('',*,*,#13196,.F.);
#17420=ORIENTED_EDGE('',*,*,#13197,.T.);
#17421=ORIENTED_EDGE('',*,*,#12883,.T.);
#17422=ORIENTED_EDGE('',*,*,#13190,.T.);
#17423=ORIENTED_EDGE('',*,*,#13198,.F.);
#17424=ORIENTED_EDGE('',*,*,#13199,.T.);
#17425=ORIENTED_EDGE('',*,*,#12875,.T.);
#17426=ORIENTED_EDGE('',*,*,#13200,.T.);
#17427=ORIENTED_EDGE('',*,*,#13199,.F.);
#17428=ORIENTED_EDGE('',*,*,#13201,.T.);
#17429=ORIENTED_EDGE('',*,*,#13202,.F.);
#17430=ORIENTED_EDGE('',*,*,#12876,.F.);
#17431=ORIENTED_EDGE('',*,*,#13203,.F.);
#17432=ORIENTED_EDGE('',*,*,#13204,.T.);
#17433=ORIENTED_EDGE('',*,*,#12873,.T.);
#17434=ORIENTED_EDGE('',*,*,#13205,.T.);
#17435=ORIENTED_EDGE('',*,*,#13198,.T.);
#17436=ORIENTED_EDGE('',*,*,#13206,.F.);
#17437=ORIENTED_EDGE('',*,*,#13203,.T.);
#17438=ORIENTED_EDGE('',*,*,#13207,.F.);
#17439=ORIENTED_EDGE('',*,*,#13208,.T.);
#17440=ORIENTED_EDGE('',*,*,#13201,.F.);
#17441=ORIENTED_EDGE('',*,*,#13205,.F.);
#17442=ORIENTED_EDGE('',*,*,#12872,.F.);
#17443=ORIENTED_EDGE('',*,*,#13209,.F.);
#17444=ORIENTED_EDGE('',*,*,#13207,.T.);
#17445=ORIENTED_EDGE('',*,*,#13208,.F.);
#17446=ORIENTED_EDGE('',*,*,#13209,.T.);
#17447=ORIENTED_EDGE('',*,*,#12877,.T.);
#17448=ORIENTED_EDGE('',*,*,#13202,.T.);
#17449=ORIENTED_EDGE('',*,*,#12843,.F.);
#17450=ORIENTED_EDGE('',*,*,#13210,.T.);
#17451=ORIENTED_EDGE('',*,*,#13211,.F.);
#17452=ORIENTED_EDGE('',*,*,#13212,.T.);
#17453=ORIENTED_EDGE('',*,*,#13213,.F.);
#17454=ORIENTED_EDGE('',*,*,#13214,.T.);
#17455=ORIENTED_EDGE('',*,*,#12841,.T.);
#17456=ORIENTED_EDGE('',*,*,#13215,.T.);
#17457=ORIENTED_EDGE('',*,*,#13211,.T.);
#17458=ORIENTED_EDGE('',*,*,#13216,.F.);
#17459=ORIENTED_EDGE('',*,*,#13213,.T.);
#17460=ORIENTED_EDGE('',*,*,#13217,.F.);
#17461=ORIENTED_EDGE('',*,*,#13218,.T.);
#17462=ORIENTED_EDGE('',*,*,#13215,.F.);
#17463=ORIENTED_EDGE('',*,*,#12840,.F.);
#17464=ORIENTED_EDGE('',*,*,#13219,.T.);
#17465=ORIENTED_EDGE('',*,*,#13217,.T.);
#17466=ORIENTED_EDGE('',*,*,#13220,.F.);
#17467=ORIENTED_EDGE('',*,*,#13221,.T.);
#17468=ORIENTED_EDGE('',*,*,#12869,.T.);
#17469=ORIENTED_EDGE('',*,*,#13222,.T.);
#17470=ORIENTED_EDGE('',*,*,#13221,.F.);
#17471=ORIENTED_EDGE('',*,*,#13223,.T.);
#17472=ORIENTED_EDGE('',*,*,#13224,.F.);
#17473=ORIENTED_EDGE('',*,*,#12870,.F.);
#17474=ORIENTED_EDGE('',*,*,#13225,.F.);
#17475=ORIENTED_EDGE('',*,*,#13226,.T.);
#17476=ORIENTED_EDGE('',*,*,#12867,.T.);
#17477=ORIENTED_EDGE('',*,*,#13227,.T.);
#17478=ORIENTED_EDGE('',*,*,#13220,.T.);
#17479=ORIENTED_EDGE('',*,*,#13228,.F.);
#17480=ORIENTED_EDGE('',*,*,#13225,.T.);
#17481=ORIENTED_EDGE('',*,*,#13229,.F.);
#17482=ORIENTED_EDGE('',*,*,#13230,.T.);
#17483=ORIENTED_EDGE('',*,*,#13223,.F.);
#17484=ORIENTED_EDGE('',*,*,#13227,.F.);
#17485=ORIENTED_EDGE('',*,*,#12866,.F.);
#17486=ORIENTED_EDGE('',*,*,#13231,.F.);
#17487=ORIENTED_EDGE('',*,*,#13229,.T.);
#17488=ORIENTED_EDGE('',*,*,#13230,.F.);
#17489=ORIENTED_EDGE('',*,*,#13231,.T.);
#17490=ORIENTED_EDGE('',*,*,#12871,.T.);
#17491=ORIENTED_EDGE('',*,*,#13224,.T.);
#17492=ORIENTED_EDGE('',*,*,#13232,.F.);
#17493=ORIENTED_EDGE('',*,*,#13233,.T.);
#17494=ORIENTED_EDGE('',*,*,#12863,.T.);
#17495=ORIENTED_EDGE('',*,*,#13234,.T.);
#17496=ORIENTED_EDGE('',*,*,#13233,.F.);
#17497=ORIENTED_EDGE('',*,*,#13235,.T.);
#17498=ORIENTED_EDGE('',*,*,#13236,.F.);
#17499=ORIENTED_EDGE('',*,*,#12864,.F.);
#17500=ORIENTED_EDGE('',*,*,#13237,.F.);
#17501=ORIENTED_EDGE('',*,*,#13238,.T.);
#17502=ORIENTED_EDGE('',*,*,#12861,.T.);
#17503=ORIENTED_EDGE('',*,*,#13239,.T.);
#17504=ORIENTED_EDGE('',*,*,#13232,.T.);
#17505=ORIENTED_EDGE('',*,*,#13240,.F.);
#17506=ORIENTED_EDGE('',*,*,#13237,.T.);
#17507=ORIENTED_EDGE('',*,*,#13241,.F.);
#17508=ORIENTED_EDGE('',*,*,#13242,.T.);
#17509=ORIENTED_EDGE('',*,*,#13235,.F.);
#17510=ORIENTED_EDGE('',*,*,#13239,.F.);
#17511=ORIENTED_EDGE('',*,*,#12860,.F.);
#17512=ORIENTED_EDGE('',*,*,#13243,.F.);
#17513=ORIENTED_EDGE('',*,*,#13241,.T.);
#17514=ORIENTED_EDGE('',*,*,#13242,.F.);
#17515=ORIENTED_EDGE('',*,*,#13243,.T.);
#17516=ORIENTED_EDGE('',*,*,#12865,.T.);
#17517=ORIENTED_EDGE('',*,*,#13236,.T.);
#17518=ORIENTED_EDGE('',*,*,#13244,.F.);
#17519=ORIENTED_EDGE('',*,*,#13245,.T.);
#17520=ORIENTED_EDGE('',*,*,#12857,.T.);
#17521=ORIENTED_EDGE('',*,*,#13246,.T.);
#17522=ORIENTED_EDGE('',*,*,#13245,.F.);
#17523=ORIENTED_EDGE('',*,*,#13247,.T.);
#17524=ORIENTED_EDGE('',*,*,#13248,.F.);
#17525=ORIENTED_EDGE('',*,*,#12858,.F.);
#17526=ORIENTED_EDGE('',*,*,#13249,.F.);
#17527=ORIENTED_EDGE('',*,*,#13250,.T.);
#17528=ORIENTED_EDGE('',*,*,#12855,.T.);
#17529=ORIENTED_EDGE('',*,*,#13251,.T.);
#17530=ORIENTED_EDGE('',*,*,#13244,.T.);
#17531=ORIENTED_EDGE('',*,*,#13252,.F.);
#17532=ORIENTED_EDGE('',*,*,#13249,.T.);
#17533=ORIENTED_EDGE('',*,*,#13253,.F.);
#17534=ORIENTED_EDGE('',*,*,#13254,.T.);
#17535=ORIENTED_EDGE('',*,*,#13247,.F.);
#17536=ORIENTED_EDGE('',*,*,#13251,.F.);
#17537=ORIENTED_EDGE('',*,*,#12854,.F.);
#17538=ORIENTED_EDGE('',*,*,#13255,.F.);
#17539=ORIENTED_EDGE('',*,*,#13253,.T.);
#17540=ORIENTED_EDGE('',*,*,#13254,.F.);
#17541=ORIENTED_EDGE('',*,*,#13255,.T.);
#17542=ORIENTED_EDGE('',*,*,#12859,.T.);
#17543=ORIENTED_EDGE('',*,*,#13248,.T.);
#17544=ORIENTED_EDGE('',*,*,#13256,.F.);
#17545=ORIENTED_EDGE('',*,*,#13257,.T.);
#17546=ORIENTED_EDGE('',*,*,#12845,.T.);
#17547=ORIENTED_EDGE('',*,*,#13258,.T.);
#17548=ORIENTED_EDGE('',*,*,#12964,.T.);
#17549=ORIENTED_EDGE('',*,*,#13259,.F.);
#17550=ORIENTED_EDGE('',*,*,#13256,.T.);
#17551=ORIENTED_EDGE('',*,*,#13260,.F.);
#17552=ORIENTED_EDGE('',*,*,#13261,.T.);
#17553=ORIENTED_EDGE('',*,*,#13258,.F.);
#17554=ORIENTED_EDGE('',*,*,#12844,.F.);
#17555=ORIENTED_EDGE('',*,*,#13262,.T.);
#17556=ORIENTED_EDGE('',*,*,#13260,.T.);
#17557=ORIENTED_EDGE('',*,*,#13263,.F.);
#17558=ORIENTED_EDGE('',*,*,#13264,.T.);
#17559=ORIENTED_EDGE('',*,*,#12835,.T.);
#17560=ORIENTED_EDGE('',*,*,#13265,.T.);
#17561=ORIENTED_EDGE('',*,*,#13264,.F.);
#17562=ORIENTED_EDGE('',*,*,#13266,.T.);
#17563=ORIENTED_EDGE('',*,*,#13267,.T.);
#17564=ORIENTED_EDGE('',*,*,#12836,.F.);
#17565=ORIENTED_EDGE('',*,*,#13268,.F.);
#17566=ORIENTED_EDGE('',*,*,#13269,.T.);
#17567=ORIENTED_EDGE('',*,*,#12838,.F.);
#17568=ORIENTED_EDGE('',*,*,#13270,.T.);
#17569=ORIENTED_EDGE('',*,*,#13263,.T.);
#17570=ORIENTED_EDGE('',*,*,#13271,.F.);
#17571=ORIENTED_EDGE('',*,*,#13268,.T.);
#17572=ORIENTED_EDGE('',*,*,#13272,.T.);
#17573=ORIENTED_EDGE('',*,*,#13266,.F.);
#17574=ORIENTED_EDGE('',*,*,#13273,.F.);
#17575=ORIENTED_EDGE('',*,*,#13274,.T.);
#17576=ORIENTED_EDGE('',*,*,#12825,.T.);
#17577=ORIENTED_EDGE('',*,*,#13275,.T.);
#17578=ORIENTED_EDGE('',*,*,#13001,.T.);
#17579=ORIENTED_EDGE('',*,*,#13276,.F.);
#17580=ORIENTED_EDGE('',*,*,#13273,.T.);
#17581=ORIENTED_EDGE('',*,*,#13277,.F.);
#17582=ORIENTED_EDGE('',*,*,#13278,.T.);
#17583=ORIENTED_EDGE('',*,*,#13275,.F.);
#17584=ORIENTED_EDGE('',*,*,#12824,.F.);
#17585=ORIENTED_EDGE('',*,*,#13279,.T.);
#17586=ORIENTED_EDGE('',*,*,#13277,.T.);
#17587=ORIENTED_EDGE('',*,*,#13280,.F.);
#17588=ORIENTED_EDGE('',*,*,#13281,.T.);
#17589=ORIENTED_EDGE('',*,*,#12818,.F.);
#17590=ORIENTED_EDGE('',*,*,#13282,.T.);
#17591=ORIENTED_EDGE('',*,*,#13027,.T.);
#17592=ORIENTED_EDGE('',*,*,#13283,.F.);
#17593=ORIENTED_EDGE('',*,*,#13280,.T.);
#17594=ORIENTED_EDGE('',*,*,#13284,.T.);
#17595=ORIENTED_EDGE('',*,*,#13030,.F.);
#17596=ORIENTED_EDGE('',*,*,#13285,.F.);
#17597=ORIENTED_EDGE('',*,*,#13286,.T.);
#17598=ORIENTED_EDGE('',*,*,#12805,.T.);
#17599=ORIENTED_EDGE('',*,*,#13287,.T.);
#17600=ORIENTED_EDGE('',*,*,#13150,.T.);
#17601=ORIENTED_EDGE('',*,*,#13288,.F.);
#17602=ORIENTED_EDGE('',*,*,#13285,.T.);
#17603=ORIENTED_EDGE('',*,*,#13289,.F.);
#17604=ORIENTED_EDGE('',*,*,#13290,.T.);
#17605=ORIENTED_EDGE('',*,*,#13287,.F.);
#17606=ORIENTED_EDGE('',*,*,#12804,.F.);
#17607=ORIENTED_EDGE('',*,*,#13291,.T.);
#17608=ORIENTED_EDGE('',*,*,#13289,.T.);
#17609=ORIENTED_EDGE('',*,*,#13292,.F.);
#17610=ORIENTED_EDGE('',*,*,#13293,.T.);
#17611=ORIENTED_EDGE('',*,*,#12798,.F.);
#17612=ORIENTED_EDGE('',*,*,#13294,.T.);
#17613=ORIENTED_EDGE('',*,*,#13099,.T.);
#17614=ORIENTED_EDGE('',*,*,#13295,.F.);
#17615=ORIENTED_EDGE('',*,*,#13292,.T.);
#17616=ORIENTED_EDGE('',*,*,#13296,.T.);
#17617=ORIENTED_EDGE('',*,*,#13102,.F.);
#17618=ORIENTED_EDGE('',*,*,#13262,.F.);
#17619=ORIENTED_EDGE('',*,*,#12848,.T.);
#17620=ORIENTED_EDGE('',*,*,#12965,.F.);
#17621=ORIENTED_EDGE('',*,*,#13261,.F.);
#17622=ORIENTED_EDGE('',*,*,#12970,.F.);
#17623=ORIENTED_EDGE('',*,*,#12975,.F.);
#17624=ORIENTED_EDGE('',*,*,#12973,.F.);
#17625=ORIENTED_EDGE('',*,*,#12849,.T.);
#17626=ORIENTED_EDGE('',*,*,#13270,.F.);
#17627=ORIENTED_EDGE('',*,*,#12837,.T.);
#17628=ORIENTED_EDGE('',*,*,#13267,.F.);
#17629=ORIENTED_EDGE('',*,*,#13272,.F.);
#17630=ORIENTED_EDGE('',*,*,#13212,.F.);
#17631=ORIENTED_EDGE('',*,*,#13218,.F.);
#17632=ORIENTED_EDGE('',*,*,#13219,.F.);
#17633=ORIENTED_EDGE('',*,*,#12839,.T.);
#17634=ORIENTED_EDGE('',*,*,#13279,.F.);
#17635=ORIENTED_EDGE('',*,*,#12828,.T.);
#17636=ORIENTED_EDGE('',*,*,#13002,.F.);
#17637=ORIENTED_EDGE('',*,*,#13278,.F.);
#17638=ORIENTED_EDGE('',*,*,#13297,.F.);
#17639=ORIENTED_EDGE('',*,*,#13037,.F.);
#17640=ORIENTED_EDGE('',*,*,#13040,.F.);
#17641=ORIENTED_EDGE('',*,*,#12829,.T.);
#17642=ORIENTED_EDGE('',*,*,#13282,.F.);
#17643=ORIENTED_EDGE('',*,*,#12817,.T.);
#17644=ORIENTED_EDGE('',*,*,#13031,.F.);
#17645=ORIENTED_EDGE('',*,*,#13284,.F.);
#17646=ORIENTED_EDGE('',*,*,#13067,.F.);
#17647=ORIENTED_EDGE('',*,*,#13071,.F.);
#17648=ORIENTED_EDGE('',*,*,#13074,.F.);
#17649=ORIENTED_EDGE('',*,*,#12819,.T.);
#17650=ORIENTED_EDGE('',*,*,#13291,.F.);
#17651=ORIENTED_EDGE('',*,*,#12808,.T.);
#17652=ORIENTED_EDGE('',*,*,#13151,.F.);
#17653=ORIENTED_EDGE('',*,*,#13290,.F.);
#17654=ORIENTED_EDGE('',*,*,#13298,.F.);
#17655=ORIENTED_EDGE('',*,*,#13109,.F.);
#17656=ORIENTED_EDGE('',*,*,#13112,.F.);
#17657=ORIENTED_EDGE('',*,*,#12809,.T.);
#17658=ORIENTED_EDGE('',*,*,#13294,.F.);
#17659=ORIENTED_EDGE('',*,*,#12797,.T.);
#17660=ORIENTED_EDGE('',*,*,#13103,.F.);
#17661=ORIENTED_EDGE('',*,*,#13296,.F.);
#17662=ORIENTED_EDGE('',*,*,#13178,.F.);
#17663=ORIENTED_EDGE('',*,*,#13182,.F.);
#17664=ORIENTED_EDGE('',*,*,#13185,.F.);
#17665=ORIENTED_EDGE('',*,*,#12799,.T.);
#17666=ORIENTED_EDGE('',*,*,#13265,.F.);
#17667=ORIENTED_EDGE('',*,*,#12834,.F.);
#17668=ORIENTED_EDGE('',*,*,#13269,.F.);
#17669=ORIENTED_EDGE('',*,*,#13271,.T.);
#17670=ORIENTED_EDGE('',*,*,#13246,.F.);
#17671=ORIENTED_EDGE('',*,*,#12856,.F.);
#17672=ORIENTED_EDGE('',*,*,#13250,.F.);
#17673=ORIENTED_EDGE('',*,*,#13252,.T.);
#17674=ORIENTED_EDGE('',*,*,#13234,.F.);
#17675=ORIENTED_EDGE('',*,*,#12862,.F.);
#17676=ORIENTED_EDGE('',*,*,#13238,.F.);
#17677=ORIENTED_EDGE('',*,*,#13240,.T.);
#17678=ORIENTED_EDGE('',*,*,#13222,.F.);
#17679=ORIENTED_EDGE('',*,*,#12868,.F.);
#17680=ORIENTED_EDGE('',*,*,#13226,.F.);
#17681=ORIENTED_EDGE('',*,*,#13228,.T.);
#17682=ORIENTED_EDGE('',*,*,#13210,.F.);
#17683=ORIENTED_EDGE('',*,*,#12842,.F.);
#17684=ORIENTED_EDGE('',*,*,#13214,.F.);
#17685=ORIENTED_EDGE('',*,*,#13216,.T.);
#17686=ORIENTED_EDGE('',*,*,#13200,.F.);
#17687=ORIENTED_EDGE('',*,*,#12874,.F.);
#17688=ORIENTED_EDGE('',*,*,#13204,.F.);
#17689=ORIENTED_EDGE('',*,*,#13206,.T.);
#17690=ORIENTED_EDGE('',*,*,#13188,.F.);
#17691=ORIENTED_EDGE('',*,*,#12880,.F.);
#17692=ORIENTED_EDGE('',*,*,#13192,.F.);
#17693=ORIENTED_EDGE('',*,*,#13194,.T.);
#17694=ORIENTED_EDGE('',*,*,#13166,.F.);
#17695=ORIENTED_EDGE('',*,*,#12886,.F.);
#17696=ORIENTED_EDGE('',*,*,#13170,.F.);
#17697=ORIENTED_EDGE('',*,*,#13172,.T.);
#17698=ORIENTED_EDGE('',*,*,#13154,.F.);
#17699=ORIENTED_EDGE('',*,*,#12892,.F.);
#17700=ORIENTED_EDGE('',*,*,#13158,.F.);
#17701=ORIENTED_EDGE('',*,*,#13160,.T.);
#17702=ORIENTED_EDGE('',*,*,#13149,.F.);
#17703=ORIENTED_EDGE('',*,*,#12806,.F.);
#17704=ORIENTED_EDGE('',*,*,#13286,.F.);
#17705=ORIENTED_EDGE('',*,*,#13288,.T.);
#17706=ORIENTED_EDGE('',*,*,#13139,.F.);
#17707=ORIENTED_EDGE('',*,*,#12898,.F.);
#17708=ORIENTED_EDGE('',*,*,#13143,.F.);
#17709=ORIENTED_EDGE('',*,*,#13145,.T.);
#17710=ORIENTED_EDGE('',*,*,#13127,.F.);
#17711=ORIENTED_EDGE('',*,*,#12904,.F.);
#17712=ORIENTED_EDGE('',*,*,#13131,.F.);
#17713=ORIENTED_EDGE('',*,*,#13133,.T.);
#17714=ORIENTED_EDGE('',*,*,#13115,.F.);
#17715=ORIENTED_EDGE('',*,*,#12910,.F.);
#17716=ORIENTED_EDGE('',*,*,#13119,.F.);
#17717=ORIENTED_EDGE('',*,*,#13121,.T.);
#17718=ORIENTED_EDGE('',*,*,#13105,.F.);
#17719=ORIENTED_EDGE('',*,*,#13110,.T.);
#17720=ORIENTED_EDGE('',*,*,#13298,.T.);
#17721=ORIENTED_EDGE('',*,*,#12813,.F.);
#17722=ORIENTED_EDGE('',*,*,#13101,.F.);
#17723=ORIENTED_EDGE('',*,*,#12794,.F.);
#17724=ORIENTED_EDGE('',*,*,#13293,.F.);
#17725=ORIENTED_EDGE('',*,*,#13295,.T.);
#17726=ORIENTED_EDGE('',*,*,#13089,.F.);
#17727=ORIENTED_EDGE('',*,*,#12916,.F.);
#17728=ORIENTED_EDGE('',*,*,#13093,.F.);
#17729=ORIENTED_EDGE('',*,*,#13095,.T.);
#17730=ORIENTED_EDGE('',*,*,#13077,.F.);
#17731=ORIENTED_EDGE('',*,*,#12922,.F.);
#17732=ORIENTED_EDGE('',*,*,#13081,.F.);
#17733=ORIENTED_EDGE('',*,*,#13083,.T.);
#17734=ORIENTED_EDGE('',*,*,#13055,.F.);
#17735=ORIENTED_EDGE('',*,*,#12928,.F.);
#17736=ORIENTED_EDGE('',*,*,#13059,.F.);
#17737=ORIENTED_EDGE('',*,*,#13061,.T.);
#17738=ORIENTED_EDGE('',*,*,#13043,.F.);
#17739=ORIENTED_EDGE('',*,*,#12934,.F.);
#17740=ORIENTED_EDGE('',*,*,#13047,.F.);
#17741=ORIENTED_EDGE('',*,*,#13049,.T.);
#17742=ORIENTED_EDGE('',*,*,#13033,.F.);
#17743=ORIENTED_EDGE('',*,*,#13038,.T.);
#17744=ORIENTED_EDGE('',*,*,#13297,.T.);
#17745=ORIENTED_EDGE('',*,*,#12833,.F.);
#17746=ORIENTED_EDGE('',*,*,#13029,.F.);
#17747=ORIENTED_EDGE('',*,*,#12814,.F.);
#17748=ORIENTED_EDGE('',*,*,#13281,.F.);
#17749=ORIENTED_EDGE('',*,*,#13283,.T.);
#17750=ORIENTED_EDGE('',*,*,#13017,.F.);
#17751=ORIENTED_EDGE('',*,*,#12940,.F.);
#17752=ORIENTED_EDGE('',*,*,#13021,.F.);
#17753=ORIENTED_EDGE('',*,*,#13023,.T.);
#17754=ORIENTED_EDGE('',*,*,#13005,.F.);
#17755=ORIENTED_EDGE('',*,*,#12946,.F.);
#17756=ORIENTED_EDGE('',*,*,#13009,.F.);
#17757=ORIENTED_EDGE('',*,*,#13011,.T.);
#17758=ORIENTED_EDGE('',*,*,#13000,.F.);
#17759=ORIENTED_EDGE('',*,*,#12826,.F.);
#17760=ORIENTED_EDGE('',*,*,#13274,.F.);
#17761=ORIENTED_EDGE('',*,*,#13276,.T.);
#17762=ORIENTED_EDGE('',*,*,#12990,.F.);
#17763=ORIENTED_EDGE('',*,*,#12952,.F.);
#17764=ORIENTED_EDGE('',*,*,#12994,.F.);
#17765=ORIENTED_EDGE('',*,*,#12996,.T.);
#17766=ORIENTED_EDGE('',*,*,#12978,.F.);
#17767=ORIENTED_EDGE('',*,*,#12958,.F.);
#17768=ORIENTED_EDGE('',*,*,#12982,.F.);
#17769=ORIENTED_EDGE('',*,*,#12984,.T.);
#17770=ORIENTED_EDGE('',*,*,#12968,.F.);
#17771=ORIENTED_EDGE('',*,*,#12851,.F.);
#17772=ORIENTED_EDGE('',*,*,#12972,.F.);
#17773=ORIENTED_EDGE('',*,*,#12974,.T.);
#17774=ORIENTED_EDGE('',*,*,#12963,.F.);
#17775=ORIENTED_EDGE('',*,*,#12846,.F.);
#17776=ORIENTED_EDGE('',*,*,#13257,.F.);
#17777=ORIENTED_EDGE('',*,*,#13259,.T.);
#17778=ORIENTED_EDGE('',*,*,#12780,.T.);
#17779=ORIENTED_EDGE('',*,*,#13299,.T.);
#17780=ORIENTED_EDGE('',*,*,#13300,.F.);
#17781=ORIENTED_EDGE('',*,*,#13299,.F.);
#17782=ORIENTED_EDGE('',*,*,#13301,.F.);
#17783=ORIENTED_EDGE('',*,*,#13300,.T.);
#17784=ORIENTED_EDGE('',*,*,#12791,.F.);
#17785=ORIENTED_EDGE('',*,*,#13302,.T.);
#17786=ORIENTED_EDGE('',*,*,#13301,.T.);
#17787=ORIENTED_EDGE('',*,*,#13302,.F.);
#17788=ORIENTED_EDGE('',*,*,#12962,.T.);
#17789=ORIENTED_EDGE('',*,*,#13303,.T.);
#17790=ORIENTED_EDGE('',*,*,#12783,.F.);
#17791=ORIENTED_EDGE('',*,*,#13303,.F.);
#17792=ORIENTED_EDGE('',*,*,#13304,.T.);
#17793=ORIENTED_EDGE('',*,*,#13305,.T.);
#17794=ORIENTED_EDGE('',*,*,#13306,.T.);
#17795=ORIENTED_EDGE('',*,*,#13307,.T.);
#17796=ORIENTED_EDGE('',*,*,#13305,.F.);
#17797=ORIENTED_EDGE('',*,*,#13306,.F.);
#17798=ORIENTED_EDGE('',*,*,#13307,.F.);
#17799=ORIENTED_EDGE('',*,*,#13308,.T.);
#17800=ORIENTED_EDGE('',*,*,#13309,.F.);
#17801=ORIENTED_EDGE('',*,*,#13310,.F.);
#17802=ORIENTED_EDGE('',*,*,#13308,.F.);
#17803=ORIENTED_EDGE('',*,*,#13304,.F.);
#17804=ORIENTED_EDGE('',*,*,#13311,.F.);
#17805=ORIENTED_EDGE('',*,*,#13309,.T.);
#17806=ORIENTED_EDGE('',*,*,#13310,.T.);
#17807=ORIENTED_EDGE('',*,*,#13312,.T.);
#17808=ORIENTED_EDGE('',*,*,#13313,.T.);
#17809=ORIENTED_EDGE('',*,*,#13312,.F.);
#17810=ORIENTED_EDGE('',*,*,#13313,.F.);
#17811=ORIENTED_EDGE('',*,*,#13314,.T.);
#17812=ORIENTED_EDGE('',*,*,#13315,.T.);
#17813=ORIENTED_EDGE('',*,*,#13316,.T.);
#17814=ORIENTED_EDGE('',*,*,#13317,.T.);
#17815=ORIENTED_EDGE('',*,*,#13316,.F.);
#17816=ORIENTED_EDGE('',*,*,#13318,.F.);
#17817=ORIENTED_EDGE('',*,*,#13319,.T.);
#17818=ORIENTED_EDGE('',*,*,#13315,.F.);
#17819=ORIENTED_EDGE('',*,*,#13319,.F.);
#17820=ORIENTED_EDGE('',*,*,#13320,.F.);
#17821=ORIENTED_EDGE('',*,*,#13317,.F.);
#17822=ORIENTED_EDGE('',*,*,#13318,.T.);
#17823=ORIENTED_EDGE('',*,*,#13321,.T.);
#17824=ORIENTED_EDGE('',*,*,#13322,.T.);
#17825=ORIENTED_EDGE('',*,*,#13323,.T.);
#17826=ORIENTED_EDGE('',*,*,#13321,.F.);
#17827=ORIENTED_EDGE('',*,*,#13322,.F.);
#17828=ORIENTED_EDGE('',*,*,#13323,.F.);
#17829=ORIENTED_EDGE('',*,*,#13324,.T.);
#17830=ORIENTED_EDGE('',*,*,#13325,.F.);
#17831=ORIENTED_EDGE('',*,*,#13326,.F.);
#17832=ORIENTED_EDGE('',*,*,#13324,.F.);
#17833=ORIENTED_EDGE('',*,*,#13327,.T.);
#17834=ORIENTED_EDGE('',*,*,#13328,.T.);
#17835=ORIENTED_EDGE('',*,*,#13325,.T.);
#17836=ORIENTED_EDGE('',*,*,#13326,.T.);
#17837=ORIENTED_EDGE('',*,*,#13328,.F.);
#17838=ORIENTED_EDGE('',*,*,#13329,.F.);
#17839=ORIENTED_EDGE('',*,*,#13330,.T.);
#17840=ORIENTED_EDGE('',*,*,#13327,.F.);
#17841=ORIENTED_EDGE('',*,*,#13330,.F.);
#17842=ORIENTED_EDGE('',*,*,#13329,.T.);
#17843=ORIENTED_EDGE('',*,*,#13331,.T.);
#17844=ORIENTED_EDGE('',*,*,#13332,.T.);
#17845=ORIENTED_EDGE('',*,*,#13331,.F.);
#17846=ORIENTED_EDGE('',*,*,#13333,.F.);
#17847=ORIENTED_EDGE('',*,*,#13332,.F.);
#17848=ORIENTED_EDGE('',*,*,#13334,.T.);
#17849=ORIENTED_EDGE('',*,*,#13335,.T.);
#17850=ORIENTED_EDGE('',*,*,#13336,.T.);
#17851=ORIENTED_EDGE('',*,*,#13333,.T.);
#17852=ORIENTED_EDGE('',*,*,#13336,.F.);
#17853=ORIENTED_EDGE('',*,*,#13314,.F.);
#17854=ORIENTED_EDGE('',*,*,#13337,.T.);
#17855=ORIENTED_EDGE('',*,*,#13334,.F.);
#17856=ORIENTED_EDGE('',*,*,#13335,.F.);
#17857=ORIENTED_EDGE('',*,*,#13337,.F.);
#17858=ORIENTED_EDGE('',*,*,#13320,.T.);
#17859=ORIENTED_EDGE('',*,*,#13338,.T.);
#17860=ORIENTED_EDGE('',*,*,#13339,.T.);
#17861=ORIENTED_EDGE('',*,*,#13338,.F.);
#17862=ORIENTED_EDGE('',*,*,#13339,.F.);
#17863=ORIENTED_EDGE('',*,*,#13340,.T.);
#17864=ORIENTED_EDGE('',*,*,#13341,.F.);
#17865=ORIENTED_EDGE('',*,*,#13340,.F.);
#17866=ORIENTED_EDGE('',*,*,#13341,.T.);
#17867=ORIENTED_EDGE('',*,*,#13342,.T.);
#17868=ORIENTED_EDGE('',*,*,#13343,.T.);
#17869=ORIENTED_EDGE('',*,*,#13342,.F.);
#17870=ORIENTED_EDGE('',*,*,#13343,.F.);
#17871=ORIENTED_EDGE('',*,*,#13344,.T.);
#17872=ORIENTED_EDGE('',*,*,#13345,.T.);
#17873=ORIENTED_EDGE('',*,*,#13344,.F.);
#17874=ORIENTED_EDGE('',*,*,#13345,.F.);
#17875=ORIENTED_EDGE('',*,*,#13346,.T.);
#17876=ORIENTED_EDGE('',*,*,#13311,.T.);
#17877=ORIENTED_EDGE('',*,*,#13346,.F.);
#17878=ORIENTED_EDGE('',*,*,#13347,.T.);
#17879=ORIENTED_EDGE('',*,*,#13348,.T.);
#17880=ORIENTED_EDGE('',*,*,#13349,.T.);
#17881=ORIENTED_EDGE('',*,*,#13350,.T.);
#17882=ORIENTED_EDGE('',*,*,#13348,.F.);
#17883=ORIENTED_EDGE('',*,*,#13351,.F.);
#17884=ORIENTED_EDGE('',*,*,#13352,.T.);
#17885=ORIENTED_EDGE('',*,*,#13353,.T.);
#17886=ORIENTED_EDGE('',*,*,#13347,.F.);
#17887=ORIENTED_EDGE('',*,*,#13354,.T.);
#17888=ORIENTED_EDGE('',*,*,#13355,.T.);
#17889=ORIENTED_EDGE('',*,*,#13349,.F.);
#17890=ORIENTED_EDGE('',*,*,#13350,.F.);
#17891=ORIENTED_EDGE('',*,*,#13355,.F.);
#17892=ORIENTED_EDGE('',*,*,#13356,.T.);
#17893=ORIENTED_EDGE('',*,*,#13357,.T.);
#17894=ORIENTED_EDGE('',*,*,#13351,.T.);
#17895=ORIENTED_EDGE('',*,*,#13357,.F.);
#17896=ORIENTED_EDGE('',*,*,#13358,.F.);
#17897=ORIENTED_EDGE('',*,*,#13359,.T.);
#17898=ORIENTED_EDGE('',*,*,#13356,.F.);
#17899=ORIENTED_EDGE('',*,*,#13359,.F.);
#17900=ORIENTED_EDGE('',*,*,#13358,.T.);
#17901=ORIENTED_EDGE('',*,*,#13360,.T.);
#17902=ORIENTED_EDGE('',*,*,#13361,.T.);
#17903=ORIENTED_EDGE('',*,*,#13362,.T.);
#17904=ORIENTED_EDGE('',*,*,#13360,.F.);
#17905=ORIENTED_EDGE('',*,*,#13363,.F.);
#17906=ORIENTED_EDGE('',*,*,#13364,.F.);
#17907=ORIENTED_EDGE('',*,*,#13365,.T.);
#17908=ORIENTED_EDGE('',*,*,#13361,.F.);
#17909=ORIENTED_EDGE('',*,*,#13362,.F.);
#17910=ORIENTED_EDGE('',*,*,#13365,.F.);
#17911=ORIENTED_EDGE('',*,*,#13366,.T.);
#17912=ORIENTED_EDGE('',*,*,#13367,.T.);
#17913=ORIENTED_EDGE('',*,*,#13363,.T.);
#17914=ORIENTED_EDGE('',*,*,#13364,.T.);
#17915=ORIENTED_EDGE('',*,*,#13367,.F.);
#17916=ORIENTED_EDGE('',*,*,#13368,.F.);
#17917=ORIENTED_EDGE('',*,*,#13369,.T.);
#17918=ORIENTED_EDGE('',*,*,#13366,.F.);
#17919=ORIENTED_EDGE('',*,*,#13369,.F.);
#17920=ORIENTED_EDGE('',*,*,#13370,.T.);
#17921=ORIENTED_EDGE('',*,*,#13371,.T.);
#17922=ORIENTED_EDGE('',*,*,#13372,.T.);
#17923=ORIENTED_EDGE('',*,*,#13373,.T.);
#17924=ORIENTED_EDGE('',*,*,#13371,.F.);
#17925=ORIENTED_EDGE('',*,*,#13374,.F.);
#17926=ORIENTED_EDGE('',*,*,#13375,.F.);
#17927=ORIENTED_EDGE('',*,*,#13376,.T.);
#17928=ORIENTED_EDGE('',*,*,#13372,.F.);
#17929=ORIENTED_EDGE('',*,*,#13373,.F.);
#17930=ORIENTED_EDGE('',*,*,#13376,.F.);
#17931=ORIENTED_EDGE('',*,*,#13354,.F.);
#17932=ORIENTED_EDGE('',*,*,#13370,.F.);
#17933=ORIENTED_EDGE('',*,*,#13368,.T.);
#17934=ORIENTED_EDGE('',*,*,#13377,.T.);
#17935=ORIENTED_EDGE('',*,*,#13378,.T.);
#17936=ORIENTED_EDGE('',*,*,#13379,.F.);
#17937=ORIENTED_EDGE('',*,*,#13380,.T.);
#17938=ORIENTED_EDGE('',*,*,#13381,.F.);
#17939=ORIENTED_EDGE('',*,*,#13382,.T.);
#17940=ORIENTED_EDGE('',*,*,#13377,.F.);
#17941=ORIENTED_EDGE('',*,*,#13381,.T.);
#17942=ORIENTED_EDGE('',*,*,#13383,.T.);
#17943=ORIENTED_EDGE('',*,*,#13384,.T.);
#17944=ORIENTED_EDGE('',*,*,#13385,.T.);
#17945=ORIENTED_EDGE('',*,*,#13386,.T.);
#17946=ORIENTED_EDGE('',*,*,#13384,.F.);
#17947=ORIENTED_EDGE('',*,*,#13387,.T.);
#17948=ORIENTED_EDGE('',*,*,#13388,.F.);
#17949=ORIENTED_EDGE('',*,*,#13389,.T.);
#17950=ORIENTED_EDGE('',*,*,#13385,.F.);
#17951=ORIENTED_EDGE('',*,*,#13386,.F.);
#17952=ORIENTED_EDGE('',*,*,#13389,.F.);
#17953=ORIENTED_EDGE('',*,*,#13379,.T.);
#17954=ORIENTED_EDGE('',*,*,#13390,.T.);
#17955=ORIENTED_EDGE('',*,*,#13391,.T.);
#17956=ORIENTED_EDGE('',*,*,#13392,.T.);
#17957=ORIENTED_EDGE('',*,*,#13393,.T.);
#17958=ORIENTED_EDGE('',*,*,#13391,.F.);
#17959=ORIENTED_EDGE('',*,*,#13394,.T.);
#17960=ORIENTED_EDGE('',*,*,#13395,.F.);
#17961=ORIENTED_EDGE('',*,*,#13396,.T.);
#17962=ORIENTED_EDGE('',*,*,#13392,.F.);
#17963=ORIENTED_EDGE('',*,*,#13393,.F.);
#17964=ORIENTED_EDGE('',*,*,#13396,.F.);
#17965=ORIENTED_EDGE('',*,*,#13352,.F.);
#17966=ORIENTED_EDGE('',*,*,#13397,.T.);
#17967=ORIENTED_EDGE('',*,*,#13398,.T.);
#17968=ORIENTED_EDGE('',*,*,#13397,.F.);
#17969=ORIENTED_EDGE('',*,*,#13398,.F.);
#17970=ORIENTED_EDGE('',*,*,#13399,.T.);
#17971=ORIENTED_EDGE('',*,*,#13400,.T.);
#17972=ORIENTED_EDGE('',*,*,#13399,.F.);
#17973=ORIENTED_EDGE('',*,*,#13400,.F.);
#17974=ORIENTED_EDGE('',*,*,#13401,.T.);
#17975=ORIENTED_EDGE('',*,*,#13402,.T.);
#17976=ORIENTED_EDGE('',*,*,#13401,.F.);
#17977=ORIENTED_EDGE('',*,*,#13395,.T.);
#17978=ORIENTED_EDGE('',*,*,#13402,.F.);
#17979=ORIENTED_EDGE('',*,*,#13353,.F.);
#17980=ORIENTED_EDGE('',*,*,#13403,.T.);
#17981=ORIENTED_EDGE('',*,*,#13404,.T.);
#17982=ORIENTED_EDGE('',*,*,#13403,.F.);
#17983=ORIENTED_EDGE('',*,*,#13404,.F.);
#17984=ORIENTED_EDGE('',*,*,#13405,.T.);
#17985=ORIENTED_EDGE('',*,*,#13406,.T.);
#17986=ORIENTED_EDGE('',*,*,#13405,.F.);
#17987=ORIENTED_EDGE('',*,*,#13406,.F.);
#17988=ORIENTED_EDGE('',*,*,#13407,.T.);
#17989=ORIENTED_EDGE('',*,*,#13408,.T.);
#17990=ORIENTED_EDGE('',*,*,#13407,.F.);
#17991=ORIENTED_EDGE('',*,*,#13388,.T.);
#17992=ORIENTED_EDGE('',*,*,#13408,.F.);
#17993=ORIENTED_EDGE('',*,*,#13374,.T.);
#17994=ORIENTED_EDGE('',*,*,#13375,.T.);
#17995=ORIENTED_EDGE('',*,*,#13409,.T.);
#17996=ORIENTED_EDGE('',*,*,#13410,.T.);
#17997=ORIENTED_EDGE('',*,*,#13409,.F.);
#17998=ORIENTED_EDGE('',*,*,#13382,.F.);
#17999=ORIENTED_EDGE('',*,*,#13387,.F.);
#18000=ORIENTED_EDGE('',*,*,#13383,.F.);
#18001=ORIENTED_EDGE('',*,*,#13380,.F.);
#18002=ORIENTED_EDGE('',*,*,#13394,.F.);
#18003=ORIENTED_EDGE('',*,*,#13390,.F.);
#18004=ORIENTED_EDGE('',*,*,#13378,.F.);
#18005=ORIENTED_EDGE('',*,*,#13410,.F.);
#18006=ORIENTED_EDGE('',*,*,#13411,.F.);
#18007=ORIENTED_EDGE('',*,*,#13412,.T.);
#18008=ORIENTED_EDGE('',*,*,#13413,.F.);
#18009=ORIENTED_EDGE('',*,*,#13412,.F.);
#18010=ORIENTED_EDGE('',*,*,#13414,.F.);
#18011=ORIENTED_EDGE('',*,*,#13415,.T.);
#18012=ORIENTED_EDGE('',*,*,#13416,.F.);
#18013=ORIENTED_EDGE('',*,*,#13415,.F.);
#18014=ORIENTED_EDGE('',*,*,#13417,.F.);
#18015=ORIENTED_EDGE('',*,*,#13418,.T.);
#18016=ORIENTED_EDGE('',*,*,#13419,.T.);
#18017=ORIENTED_EDGE('',*,*,#13418,.F.);
#18018=ORIENTED_EDGE('',*,*,#13419,.F.);
#18019=ORIENTED_EDGE('',*,*,#13420,.T.);
#18020=ORIENTED_EDGE('',*,*,#13421,.F.);
#18021=ORIENTED_EDGE('',*,*,#13420,.F.);
#18022=ORIENTED_EDGE('',*,*,#13422,.F.);
#18023=ORIENTED_EDGE('',*,*,#13423,.T.);
#18024=ORIENTED_EDGE('',*,*,#13424,.F.);
#18025=ORIENTED_EDGE('',*,*,#13423,.F.);
#18026=ORIENTED_EDGE('',*,*,#13425,.F.);
#18027=ORIENTED_EDGE('',*,*,#13426,.T.);
#18028=ORIENTED_EDGE('',*,*,#13427,.F.);
#18029=ORIENTED_EDGE('',*,*,#13426,.F.);
#18030=ORIENTED_EDGE('',*,*,#13428,.F.);
#18031=ORIENTED_EDGE('',*,*,#13429,.T.);
#18032=ORIENTED_EDGE('',*,*,#13430,.F.);
#18033=ORIENTED_EDGE('',*,*,#13429,.F.);
#18034=ORIENTED_EDGE('',*,*,#13431,.F.);
#18035=ORIENTED_EDGE('',*,*,#13432,.T.);
#18036=ORIENTED_EDGE('',*,*,#13433,.F.);
#18037=ORIENTED_EDGE('',*,*,#13432,.F.);
#18038=ORIENTED_EDGE('',*,*,#13434,.F.);
#18039=ORIENTED_EDGE('',*,*,#13435,.T.);
#18040=ORIENTED_EDGE('',*,*,#13436,.F.);
#18041=ORIENTED_EDGE('',*,*,#13435,.F.);
#18042=ORIENTED_EDGE('',*,*,#13437,.F.);
#18043=ORIENTED_EDGE('',*,*,#13438,.T.);
#18044=ORIENTED_EDGE('',*,*,#13439,.F.);
#18045=ORIENTED_EDGE('',*,*,#13438,.F.);
#18046=ORIENTED_EDGE('',*,*,#13440,.T.);
#18047=ORIENTED_EDGE('',*,*,#13441,.T.);
#18048=ORIENTED_EDGE('',*,*,#13442,.T.);
#18049=ORIENTED_EDGE('',*,*,#13443,.T.);
#18050=ORIENTED_EDGE('',*,*,#13441,.F.);
#18051=ORIENTED_EDGE('',*,*,#13444,.F.);
#18052=ORIENTED_EDGE('',*,*,#13445,.F.);
#18053=ORIENTED_EDGE('',*,*,#13446,.T.);
#18054=ORIENTED_EDGE('',*,*,#13442,.F.);
#18055=ORIENTED_EDGE('',*,*,#13443,.F.);
#18056=ORIENTED_EDGE('',*,*,#13446,.F.);
#18057=ORIENTED_EDGE('',*,*,#13447,.F.);
#18058=ORIENTED_EDGE('',*,*,#13414,.T.);
#18059=ORIENTED_EDGE('',*,*,#13440,.F.);
#18060=ORIENTED_EDGE('',*,*,#13437,.T.);
#18061=ORIENTED_EDGE('',*,*,#13434,.T.);
#18062=ORIENTED_EDGE('',*,*,#13431,.T.);
#18063=ORIENTED_EDGE('',*,*,#13428,.T.);
#18064=ORIENTED_EDGE('',*,*,#13425,.T.);
#18065=ORIENTED_EDGE('',*,*,#13422,.T.);
#18066=ORIENTED_EDGE('',*,*,#13417,.T.);
#18067=ORIENTED_EDGE('',*,*,#13411,.T.);
#18068=ORIENTED_EDGE('',*,*,#13444,.T.);
#18069=ORIENTED_EDGE('',*,*,#13445,.T.);
#18070=ORIENTED_EDGE('',*,*,#13448,.T.);
#18071=ORIENTED_EDGE('',*,*,#13449,.T.);
#18072=ORIENTED_EDGE('',*,*,#13448,.F.);
#18073=ORIENTED_EDGE('',*,*,#13450,.F.);
#18074=ORIENTED_EDGE('',*,*,#13416,.T.);
#18075=ORIENTED_EDGE('',*,*,#13449,.F.);
#18076=ORIENTED_EDGE('',*,*,#13439,.T.);
#18077=ORIENTED_EDGE('',*,*,#13436,.T.);
#18078=ORIENTED_EDGE('',*,*,#13433,.T.);
#18079=ORIENTED_EDGE('',*,*,#13430,.T.);
#18080=ORIENTED_EDGE('',*,*,#13427,.T.);
#18081=ORIENTED_EDGE('',*,*,#13424,.T.);
#18082=ORIENTED_EDGE('',*,*,#13421,.T.);
#18083=ORIENTED_EDGE('',*,*,#13413,.T.);
#18084=ORIENTED_EDGE('',*,*,#13450,.T.);
#18085=ORIENTED_EDGE('',*,*,#13451,.T.);
#18086=ORIENTED_EDGE('',*,*,#13452,.T.);
#18087=ORIENTED_EDGE('',*,*,#13453,.T.);
#18088=ORIENTED_EDGE('',*,*,#13451,.F.);
#18089=ORIENTED_EDGE('',*,*,#13452,.F.);
#18090=ORIENTED_EDGE('',*,*,#13453,.F.);
#18091=ORIENTED_EDGE('',*,*,#13454,.T.);
#18092=ORIENTED_EDGE('',*,*,#13455,.F.);
#18093=ORIENTED_EDGE('',*,*,#13456,.F.);
#18094=ORIENTED_EDGE('',*,*,#13454,.F.);
#18095=ORIENTED_EDGE('',*,*,#13455,.T.);
#18096=ORIENTED_EDGE('',*,*,#13456,.T.);
#18097=ORIENTED_EDGE('',*,*,#13457,.T.);
#18098=ORIENTED_EDGE('',*,*,#13447,.T.);
#18099=ORIENTED_EDGE('',*,*,#13457,.F.);
#18100=ORIENTED_EDGE('',*,*,#13458,.T.);
#18101=ORIENTED_EDGE('',*,*,#13459,.T.);
#18102=ORIENTED_EDGE('',*,*,#13458,.F.);
#18103=ORIENTED_EDGE('',*,*,#13459,.F.);
#18104=ORIENTED_EDGE('',*,*,#13460,.T.);
#18105=ORIENTED_EDGE('',*,*,#13461,.F.);
#18106=ORIENTED_EDGE('',*,*,#13460,.F.);
#18107=ORIENTED_EDGE('',*,*,#13462,.T.);
#18108=ORIENTED_EDGE('',*,*,#13463,.T.);
#18109=ORIENTED_EDGE('',*,*,#13462,.F.);
#18110=ORIENTED_EDGE('',*,*,#13463,.F.);
#18111=ORIENTED_EDGE('',*,*,#13464,.T.);
#18112=ORIENTED_EDGE('',*,*,#13465,.F.);
#18113=ORIENTED_EDGE('',*,*,#13464,.F.);
#18114=ORIENTED_EDGE('',*,*,#13466,.F.);
#18115=ORIENTED_EDGE('',*,*,#13467,.T.);
#18116=ORIENTED_EDGE('',*,*,#13468,.F.);
#18117=ORIENTED_EDGE('',*,*,#13467,.F.);
#18118=ORIENTED_EDGE('',*,*,#13466,.T.);
#18119=ORIENTED_EDGE('',*,*,#13469,.F.);
#18120=ORIENTED_EDGE('',*,*,#13468,.T.);
#18121=ORIENTED_EDGE('',*,*,#13470,.F.);
#18122=ORIENTED_EDGE('',*,*,#13471,.T.);
#18123=ORIENTED_EDGE('',*,*,#13469,.T.);
#18124=ORIENTED_EDGE('',*,*,#13471,.F.);
#18125=ORIENTED_EDGE('',*,*,#13472,.F.);
#18126=ORIENTED_EDGE('',*,*,#13473,.T.);
#18127=ORIENTED_EDGE('',*,*,#13470,.T.);
#18128=ORIENTED_EDGE('',*,*,#13473,.F.);
#18129=ORIENTED_EDGE('',*,*,#13474,.T.);
#18130=ORIENTED_EDGE('',*,*,#13475,.T.);
#18131=ORIENTED_EDGE('',*,*,#13476,.F.);
#18132=ORIENTED_EDGE('',*,*,#13475,.F.);
#18133=ORIENTED_EDGE('',*,*,#13477,.F.);
#18134=ORIENTED_EDGE('',*,*,#13474,.F.);
#18135=ORIENTED_EDGE('',*,*,#13478,.F.);
#18136=ORIENTED_EDGE('',*,*,#13476,.T.);
#18137=ORIENTED_EDGE('',*,*,#13479,.F.);
#18138=ORIENTED_EDGE('',*,*,#13480,.T.);
#18139=ORIENTED_EDGE('',*,*,#13478,.T.);
#18140=ORIENTED_EDGE('',*,*,#13480,.F.);
#18141=ORIENTED_EDGE('',*,*,#13481,.F.);
#18142=ORIENTED_EDGE('',*,*,#13472,.T.);
#18143=ORIENTED_EDGE('',*,*,#13482,.F.);
#18144=ORIENTED_EDGE('',*,*,#13483,.T.);
#18145=ORIENTED_EDGE('',*,*,#13481,.T.);
#18146=ORIENTED_EDGE('',*,*,#13483,.F.);
#18147=ORIENTED_EDGE('',*,*,#13477,.T.);
#18148=ORIENTED_EDGE('',*,*,#13484,.T.);
#18149=ORIENTED_EDGE('',*,*,#13482,.T.);
#18150=ORIENTED_EDGE('',*,*,#13484,.F.);
#18151=ORIENTED_EDGE('',*,*,#13485,.F.);
#18152=ORIENTED_EDGE('',*,*,#13486,.T.);
#18153=ORIENTED_EDGE('',*,*,#13479,.T.);
#18154=ORIENTED_EDGE('',*,*,#13486,.F.);
#18155=ORIENTED_EDGE('',*,*,#13485,.T.);
#18156=ORIENTED_EDGE('',*,*,#13461,.T.);
#18157=ORIENTED_EDGE('',*,*,#13465,.T.);
#18158=ORIENTED_EDGE('',*,*,#13487,.F.);
#18159=ORIENTED_EDGE('',*,*,#13488,.F.);
#18160=ORIENTED_EDGE('',*,*,#13489,.T.);
#18161=ORIENTED_EDGE('',*,*,#13487,.T.);
#18162=ORIENTED_EDGE('',*,*,#13489,.F.);
#18163=ORIENTED_EDGE('',*,*,#13488,.T.);
#18164=ORIENTED_EDGE('',*,*,#13490,.F.);
#18165=ORIENTED_EDGE('',*,*,#13491,.F.);
#18166=ORIENTED_EDGE('',*,*,#13492,.T.);
#18167=ORIENTED_EDGE('',*,*,#13490,.T.);
#18168=ORIENTED_EDGE('',*,*,#13492,.F.);
#18169=ORIENTED_EDGE('',*,*,#13493,.F.);
#18170=ORIENTED_EDGE('',*,*,#13494,.T.);
#18171=ORIENTED_EDGE('',*,*,#13491,.T.);
#18172=ORIENTED_EDGE('',*,*,#13494,.F.);
#18173=ORIENTED_EDGE('',*,*,#13493,.T.);
#18174=ORIENTED_EDGE('',*,*,#13495,.T.);
#18175=ORIENTED_EDGE('',*,*,#13496,.T.);
#18176=ORIENTED_EDGE('',*,*,#13497,.T.);
#18177=ORIENTED_EDGE('',*,*,#13498,.T.);
#18178=ORIENTED_EDGE('',*,*,#13496,.F.);
#18179=ORIENTED_EDGE('',*,*,#13495,.F.);
#18180=ORIENTED_EDGE('',*,*,#13499,.F.);
#18181=ORIENTED_EDGE('',*,*,#13497,.F.);
#18182=ORIENTED_EDGE('',*,*,#13498,.F.);
#18183=ORIENTED_EDGE('',*,*,#13500,.T.);
#18184=ORIENTED_EDGE('',*,*,#13501,.T.);
#18185=ORIENTED_EDGE('',*,*,#13500,.F.);
#18186=ORIENTED_EDGE('',*,*,#13502,.T.);
#18187=ORIENTED_EDGE('',*,*,#13503,.T.);
#18188=ORIENTED_EDGE('',*,*,#13504,.T.);
#18189=ORIENTED_EDGE('',*,*,#13499,.T.);
#18190=ORIENTED_EDGE('',*,*,#13504,.F.);
#18191=ORIENTED_EDGE('',*,*,#13502,.F.);
#18192=ORIENTED_EDGE('',*,*,#13503,.F.);
#18193=ORIENTED_EDGE('',*,*,#13505,.T.);
#18194=ORIENTED_EDGE('',*,*,#13506,.F.);
#18195=ORIENTED_EDGE('',*,*,#13507,.F.);
#18196=ORIENTED_EDGE('',*,*,#13508,.T.);
#18197=ORIENTED_EDGE('',*,*,#13509,.F.);
#18198=ORIENTED_EDGE('',*,*,#13510,.T.);
#18199=ORIENTED_EDGE('',*,*,#13511,.F.);
#18200=ORIENTED_EDGE('',*,*,#13512,.F.);
#18201=ORIENTED_EDGE('',*,*,#13505,.F.);
#18202=ORIENTED_EDGE('',*,*,#13513,.T.);
#18203=ORIENTED_EDGE('',*,*,#13514,.T.);
#18204=ORIENTED_EDGE('',*,*,#13515,.T.);
#18205=ORIENTED_EDGE('',*,*,#13506,.T.);
#18206=ORIENTED_EDGE('',*,*,#13512,.T.);
#18207=ORIENTED_EDGE('',*,*,#13516,.T.);
#18208=ORIENTED_EDGE('',*,*,#13514,.F.);
#18209=ORIENTED_EDGE('',*,*,#13516,.F.);
#18210=ORIENTED_EDGE('',*,*,#13511,.T.);
#18211=ORIENTED_EDGE('',*,*,#13517,.T.);
#18212=ORIENTED_EDGE('',*,*,#13518,.T.);
#18213=ORIENTED_EDGE('',*,*,#13519,.T.);
#18214=ORIENTED_EDGE('',*,*,#13507,.T.);
#18215=ORIENTED_EDGE('',*,*,#13515,.F.);
#18216=ORIENTED_EDGE('',*,*,#13520,.F.);
#18217=ORIENTED_EDGE('',*,*,#13513,.F.);
#18218=ORIENTED_EDGE('',*,*,#13521,.T.);
#18219=ORIENTED_EDGE('',*,*,#13522,.T.);
#18220=ORIENTED_EDGE('',*,*,#13523,.T.);
#18221=ORIENTED_EDGE('',*,*,#13524,.T.);
#18222=ORIENTED_EDGE('',*,*,#13525,.T.);
#18223=ORIENTED_EDGE('',*,*,#13526,.T.);
#18224=ORIENTED_EDGE('',*,*,#13524,.F.);
#18225=ORIENTED_EDGE('',*,*,#13527,.T.);
#18226=ORIENTED_EDGE('',*,*,#13528,.F.);
#18227=ORIENTED_EDGE('',*,*,#13529,.T.);
#18228=ORIENTED_EDGE('',*,*,#13527,.F.);
#18229=ORIENTED_EDGE('',*,*,#13523,.F.);
#18230=ORIENTED_EDGE('',*,*,#13530,.F.);
#18231=ORIENTED_EDGE('',*,*,#13529,.F.);
#18232=ORIENTED_EDGE('',*,*,#13531,.F.);
#18233=ORIENTED_EDGE('',*,*,#13521,.F.);
#18234=ORIENTED_EDGE('',*,*,#13530,.T.);
#18235=ORIENTED_EDGE('',*,*,#13522,.F.);
#18236=ORIENTED_EDGE('',*,*,#13532,.T.);
#18237=ORIENTED_EDGE('',*,*,#13520,.T.);
#18238=ORIENTED_EDGE('',*,*,#13532,.F.);
#18239=ORIENTED_EDGE('',*,*,#13533,.F.);
#18240=ORIENTED_EDGE('',*,*,#13534,.F.);
#18241=ORIENTED_EDGE('',*,*,#13518,.F.);
#18242=ORIENTED_EDGE('',*,*,#13535,.F.);
#18243=ORIENTED_EDGE('',*,*,#13536,.T.);
#18244=ORIENTED_EDGE('',*,*,#13525,.F.);
#18245=ORIENTED_EDGE('',*,*,#13526,.F.);
#18246=ORIENTED_EDGE('',*,*,#13536,.F.);
#18247=ORIENTED_EDGE('',*,*,#13537,.F.);
#18248=ORIENTED_EDGE('',*,*,#13538,.T.);
#18249=ORIENTED_EDGE('',*,*,#13533,.T.);
#18250=ORIENTED_EDGE('',*,*,#13539,.T.);
#18251=ORIENTED_EDGE('',*,*,#13509,.T.);
#18252=ORIENTED_EDGE('',*,*,#13540,.T.);
#18253=ORIENTED_EDGE('',*,*,#13541,.T.);
#18254=ORIENTED_EDGE('',*,*,#13542,.T.);
#18255=ORIENTED_EDGE('',*,*,#13541,.F.);
#18256=ORIENTED_EDGE('',*,*,#13542,.F.);
#18257=ORIENTED_EDGE('',*,*,#13543,.T.);
#18258=ORIENTED_EDGE('',*,*,#13544,.F.);
#18259=ORIENTED_EDGE('',*,*,#13543,.F.);
#18260=ORIENTED_EDGE('',*,*,#13545,.F.);
#18261=ORIENTED_EDGE('',*,*,#13546,.F.);
#18262=ORIENTED_EDGE('',*,*,#13531,.T.);
#18263=ORIENTED_EDGE('',*,*,#13528,.T.);
#18264=ORIENTED_EDGE('',*,*,#13547,.F.);
#18265=ORIENTED_EDGE('',*,*,#13540,.F.);
#18266=ORIENTED_EDGE('',*,*,#13548,.T.);
#18267=ORIENTED_EDGE('',*,*,#13549,.T.);
#18268=ORIENTED_EDGE('',*,*,#13544,.T.);
#18269=ORIENTED_EDGE('',*,*,#13549,.F.);
#18270=ORIENTED_EDGE('',*,*,#13550,.F.);
#18271=ORIENTED_EDGE('',*,*,#13551,.F.);
#18272=ORIENTED_EDGE('',*,*,#13501,.F.);
#18273=ORIENTED_EDGE('',*,*,#13552,.F.);
#18274=ORIENTED_EDGE('',*,*,#13548,.F.);
#18275=ORIENTED_EDGE('',*,*,#13546,.T.);
#18276=ORIENTED_EDGE('',*,*,#13553,.T.);
#18277=ORIENTED_EDGE('',*,*,#13554,.T.);
#18278=ORIENTED_EDGE('',*,*,#13553,.F.);
#18279=ORIENTED_EDGE('',*,*,#13554,.F.);
#18280=ORIENTED_EDGE('',*,*,#13555,.T.);
#18281=ORIENTED_EDGE('',*,*,#13556,.F.);
#18282=ORIENTED_EDGE('',*,*,#13555,.F.);
#18283=ORIENTED_EDGE('',*,*,#13551,.T.);
#18284=ORIENTED_EDGE('',*,*,#13557,.T.);
#18285=ORIENTED_EDGE('',*,*,#13556,.T.);
#18286=ORIENTED_EDGE('',*,*,#13557,.F.);
#18287=ORIENTED_EDGE('',*,*,#13547,.T.);
#18288=ORIENTED_EDGE('',*,*,#13558,.T.);
#18289=ORIENTED_EDGE('',*,*,#13559,.T.);
#18290=ORIENTED_EDGE('',*,*,#13558,.F.);
#18291=ORIENTED_EDGE('',*,*,#13559,.F.);
#18292=ORIENTED_EDGE('',*,*,#13560,.T.);
#18293=ORIENTED_EDGE('',*,*,#13561,.F.);
#18294=ORIENTED_EDGE('',*,*,#13560,.F.);
#18295=ORIENTED_EDGE('',*,*,#13552,.T.);
#18296=ORIENTED_EDGE('',*,*,#13562,.T.);
#18297=ORIENTED_EDGE('',*,*,#13561,.T.);
#18298=ORIENTED_EDGE('',*,*,#13562,.F.);
#18299=ORIENTED_EDGE('',*,*,#13510,.F.);
#18300=ORIENTED_EDGE('',*,*,#13539,.F.);
#18301=ORIENTED_EDGE('',*,*,#13537,.T.);
#18302=ORIENTED_EDGE('',*,*,#13535,.T.);
#18303=ORIENTED_EDGE('',*,*,#13517,.F.);
#18304=ORIENTED_EDGE('',*,*,#13508,.F.);
#18305=ORIENTED_EDGE('',*,*,#13519,.F.);
#18306=ORIENTED_EDGE('',*,*,#13534,.T.);
#18307=ORIENTED_EDGE('',*,*,#13538,.F.);
#18308=ORIENTED_EDGE('',*,*,#13550,.T.);
#18309=ORIENTED_EDGE('',*,*,#13563,.T.);
#18310=ORIENTED_EDGE('',*,*,#13564,.T.);
#18311=ORIENTED_EDGE('',*,*,#13565,.T.);
#18312=ORIENTED_EDGE('',*,*,#13563,.F.);
#18313=ORIENTED_EDGE('',*,*,#13564,.F.);
#18314=ORIENTED_EDGE('',*,*,#13565,.F.);
#18315=ORIENTED_EDGE('',*,*,#13566,.T.);
#18316=ORIENTED_EDGE('',*,*,#13567,.F.);
#18317=ORIENTED_EDGE('',*,*,#13568,.F.);
#18318=ORIENTED_EDGE('',*,*,#13566,.F.);
#18319=ORIENTED_EDGE('',*,*,#13567,.T.);
#18320=ORIENTED_EDGE('',*,*,#13568,.T.);
#18321=ORIENTED_EDGE('',*,*,#13569,.T.);
#18322=ORIENTED_EDGE('',*,*,#13545,.T.);
#18323=ORIENTED_EDGE('',*,*,#13569,.F.);
#18324=ORIENTED_EDGE('',*,*,#13570,.T.);
#18325=ORIENTED_EDGE('',*,*,#13571,.T.);
#18326=ORIENTED_EDGE('',*,*,#13572,.T.);
#18327=ORIENTED_EDGE('',*,*,#13573,.T.);
#18328=ORIENTED_EDGE('',*,*,#13571,.F.);
#18329=ORIENTED_EDGE('',*,*,#13574,.F.);
#18330=ORIENTED_EDGE('',*,*,#13575,.F.);
#18331=ORIENTED_EDGE('',*,*,#13576,.T.);
#18332=ORIENTED_EDGE('',*,*,#13572,.F.);
#18333=ORIENTED_EDGE('',*,*,#13573,.F.);
#18334=ORIENTED_EDGE('',*,*,#13576,.F.);
#18335=ORIENTED_EDGE('',*,*,#13577,.F.);
#18336=ORIENTED_EDGE('',*,*,#13578,.F.);
#18337=ORIENTED_EDGE('',*,*,#13579,.F.);
#18338=ORIENTED_EDGE('',*,*,#13580,.F.);
#18339=ORIENTED_EDGE('',*,*,#13581,.F.);
#18340=ORIENTED_EDGE('',*,*,#13582,.F.);
#18341=ORIENTED_EDGE('',*,*,#13583,.F.);
#18342=ORIENTED_EDGE('',*,*,#13584,.F.);
#18343=ORIENTED_EDGE('',*,*,#13585,.F.);
#18344=ORIENTED_EDGE('',*,*,#13570,.F.);
#18345=ORIENTED_EDGE('',*,*,#13574,.T.);
#18346=ORIENTED_EDGE('',*,*,#13575,.T.);
#18347=ORIENTED_EDGE('',*,*,#13586,.T.);
#18348=ORIENTED_EDGE('',*,*,#13587,.T.);
#18349=ORIENTED_EDGE('',*,*,#13586,.F.);
#18350=ORIENTED_EDGE('',*,*,#13588,.F.);
#18351=ORIENTED_EDGE('',*,*,#13589,.F.);
#18352=ORIENTED_EDGE('',*,*,#13590,.F.);
#18353=ORIENTED_EDGE('',*,*,#13591,.F.);
#18354=ORIENTED_EDGE('',*,*,#13587,.F.);
#18355=ORIENTED_EDGE('',*,*,#13592,.T.);
#18356=ORIENTED_EDGE('',*,*,#13593,.T.);
#18357=ORIENTED_EDGE('',*,*,#13594,.T.);
#18358=ORIENTED_EDGE('',*,*,#13578,.T.);
#18359=ORIENTED_EDGE('',*,*,#13584,.T.);
#18360=ORIENTED_EDGE('',*,*,#13581,.T.);
#18361=ORIENTED_EDGE('',*,*,#13594,.F.);
#18362=ORIENTED_EDGE('',*,*,#13595,.F.);
#18363=ORIENTED_EDGE('',*,*,#13596,.F.);
#18364=ORIENTED_EDGE('',*,*,#13597,.T.);
#18365=ORIENTED_EDGE('',*,*,#13592,.F.);
#18366=ORIENTED_EDGE('',*,*,#13593,.F.);
#18367=ORIENTED_EDGE('',*,*,#13597,.F.);
#18368=ORIENTED_EDGE('',*,*,#13580,.T.);
#18369=ORIENTED_EDGE('',*,*,#13598,.T.);
#18370=ORIENTED_EDGE('',*,*,#13599,.T.);
#18371=ORIENTED_EDGE('',*,*,#13598,.F.);
#18372=ORIENTED_EDGE('',*,*,#13579,.T.);
#18373=ORIENTED_EDGE('',*,*,#13599,.F.);
#18374=ORIENTED_EDGE('',*,*,#13600,.T.);
#18375=ORIENTED_EDGE('',*,*,#13601,.F.);
#18376=ORIENTED_EDGE('',*,*,#13600,.F.);
#18377=ORIENTED_EDGE('',*,*,#13589,.T.);
#18378=ORIENTED_EDGE('',*,*,#13602,.T.);
#18379=ORIENTED_EDGE('',*,*,#13601,.T.);
#18380=ORIENTED_EDGE('',*,*,#13602,.F.);
#18381=ORIENTED_EDGE('',*,*,#13577,.T.);
#18382=ORIENTED_EDGE('',*,*,#13603,.T.);
#18383=ORIENTED_EDGE('',*,*,#13604,.T.);
#18384=ORIENTED_EDGE('',*,*,#13603,.F.);
#18385=ORIENTED_EDGE('',*,*,#13585,.T.);
#18386=ORIENTED_EDGE('',*,*,#13604,.F.);
#18387=ORIENTED_EDGE('',*,*,#13605,.T.);
#18388=ORIENTED_EDGE('',*,*,#13606,.F.);
#18389=ORIENTED_EDGE('',*,*,#13605,.F.);
#18390=ORIENTED_EDGE('',*,*,#13591,.T.);
#18391=ORIENTED_EDGE('',*,*,#13607,.T.);
#18392=ORIENTED_EDGE('',*,*,#13606,.T.);
#18393=ORIENTED_EDGE('',*,*,#13607,.F.);
#18394=ORIENTED_EDGE('',*,*,#13583,.T.);
#18395=ORIENTED_EDGE('',*,*,#13608,.T.);
#18396=ORIENTED_EDGE('',*,*,#13609,.T.);
#18397=ORIENTED_EDGE('',*,*,#13608,.F.);
#18398=ORIENTED_EDGE('',*,*,#13582,.T.);
#18399=ORIENTED_EDGE('',*,*,#13609,.F.);
#18400=ORIENTED_EDGE('',*,*,#13610,.T.);
#18401=ORIENTED_EDGE('',*,*,#13611,.F.);
#18402=ORIENTED_EDGE('',*,*,#13610,.F.);
#18403=ORIENTED_EDGE('',*,*,#13590,.T.);
#18404=ORIENTED_EDGE('',*,*,#13612,.T.);
#18405=ORIENTED_EDGE('',*,*,#13611,.T.);
#18406=ORIENTED_EDGE('',*,*,#13612,.F.);
#18407=ORIENTED_EDGE('',*,*,#13588,.T.);
#18408=ORIENTED_EDGE('',*,*,#13613,.T.);
#18409=ORIENTED_EDGE('',*,*,#13595,.T.);
#18410=ORIENTED_EDGE('',*,*,#13596,.T.);
#18411=ORIENTED_EDGE('',*,*,#13613,.F.);
#18412=ORIENTED_EDGE('',*,*,#13614,.F.);
#18413=ORIENTED_EDGE('',*,*,#13615,.F.);
#18414=ORIENTED_EDGE('',*,*,#13616,.F.);
#18415=ORIENTED_EDGE('',*,*,#13617,.F.);
#18416=ORIENTED_EDGE('',*,*,#13618,.F.);
#18417=ORIENTED_EDGE('',*,*,#13619,.F.);
#18418=ORIENTED_EDGE('',*,*,#13620,.T.);
#18419=ORIENTED_EDGE('',*,*,#13621,.F.);
#18420=ORIENTED_EDGE('',*,*,#13622,.F.);
#18421=ORIENTED_EDGE('',*,*,#13616,.T.);
#18422=ORIENTED_EDGE('',*,*,#13623,.F.);
#18423=ORIENTED_EDGE('',*,*,#13620,.F.);
#18424=ORIENTED_EDGE('',*,*,#13617,.T.);
#18425=ORIENTED_EDGE('',*,*,#13622,.T.);
#18426=ORIENTED_EDGE('',*,*,#13619,.T.);
#18427=ORIENTED_EDGE('',*,*,#13624,.F.);
#18428=ORIENTED_EDGE('',*,*,#13625,.T.);
#18429=ORIENTED_EDGE('',*,*,#13626,.T.);
#18430=ORIENTED_EDGE('',*,*,#13627,.T.);
#18431=ORIENTED_EDGE('',*,*,#13628,.T.);
#18432=ORIENTED_EDGE('',*,*,#13629,.T.);
#18433=ORIENTED_EDGE('',*,*,#13630,.T.);
#18434=ORIENTED_EDGE('',*,*,#13631,.T.);
#18435=ORIENTED_EDGE('',*,*,#13632,.T.);
#18436=ORIENTED_EDGE('',*,*,#13633,.T.);
#18437=ORIENTED_EDGE('',*,*,#13634,.T.);
#18438=ORIENTED_EDGE('',*,*,#13635,.T.);
#18439=ORIENTED_EDGE('',*,*,#13636,.T.);
#18440=ORIENTED_EDGE('',*,*,#13637,.T.);
#18441=ORIENTED_EDGE('',*,*,#13638,.T.);
#18442=ORIENTED_EDGE('',*,*,#13639,.T.);
#18443=ORIENTED_EDGE('',*,*,#13640,.T.);
#18444=ORIENTED_EDGE('',*,*,#13641,.T.);
#18445=ORIENTED_EDGE('',*,*,#13642,.T.);
#18446=ORIENTED_EDGE('',*,*,#13643,.T.);
#18447=ORIENTED_EDGE('',*,*,#13644,.T.);
#18448=ORIENTED_EDGE('',*,*,#13645,.T.);
#18449=ORIENTED_EDGE('',*,*,#13646,.T.);
#18450=ORIENTED_EDGE('',*,*,#13647,.T.);
#18451=ORIENTED_EDGE('',*,*,#13648,.T.);
#18452=ORIENTED_EDGE('',*,*,#13649,.T.);
#18453=ORIENTED_EDGE('',*,*,#13650,.T.);
#18454=ORIENTED_EDGE('',*,*,#13651,.T.);
#18455=ORIENTED_EDGE('',*,*,#13652,.T.);
#18456=ORIENTED_EDGE('',*,*,#13614,.T.);
#18457=ORIENTED_EDGE('',*,*,#13624,.T.);
#18458=ORIENTED_EDGE('',*,*,#13618,.T.);
#18459=ORIENTED_EDGE('',*,*,#13653,.F.);
#18460=ORIENTED_EDGE('',*,*,#13654,.F.);
#18461=ORIENTED_EDGE('',*,*,#13655,.T.);
#18462=ORIENTED_EDGE('',*,*,#13625,.F.);
#18463=ORIENTED_EDGE('',*,*,#13655,.F.);
#18464=ORIENTED_EDGE('',*,*,#13656,.F.);
#18465=ORIENTED_EDGE('',*,*,#13657,.T.);
#18466=ORIENTED_EDGE('',*,*,#13652,.F.);
#18467=ORIENTED_EDGE('',*,*,#13657,.F.);
#18468=ORIENTED_EDGE('',*,*,#13658,.F.);
#18469=ORIENTED_EDGE('',*,*,#13659,.T.);
#18470=ORIENTED_EDGE('',*,*,#13626,.F.);
#18471=ORIENTED_EDGE('',*,*,#13659,.F.);
#18472=ORIENTED_EDGE('',*,*,#13648,.F.);
#18473=ORIENTED_EDGE('',*,*,#13660,.T.);
#18474=ORIENTED_EDGE('',*,*,#13661,.F.);
#18475=ORIENTED_EDGE('',*,*,#13662,.F.);
#18476=ORIENTED_EDGE('',*,*,#13651,.F.);
#18477=ORIENTED_EDGE('',*,*,#13663,.T.);
#18478=ORIENTED_EDGE('',*,*,#13664,.F.);
#18479=ORIENTED_EDGE('',*,*,#13660,.F.);
#18480=ORIENTED_EDGE('',*,*,#13650,.F.);
#18481=ORIENTED_EDGE('',*,*,#13665,.T.);
#18482=ORIENTED_EDGE('',*,*,#13666,.F.);
#18483=ORIENTED_EDGE('',*,*,#13663,.F.);
#18484=ORIENTED_EDGE('',*,*,#13649,.F.);
#18485=ORIENTED_EDGE('',*,*,#13662,.T.);
#18486=ORIENTED_EDGE('',*,*,#13667,.F.);
#18487=ORIENTED_EDGE('',*,*,#13665,.F.);
#18488=ORIENTED_EDGE('',*,*,#13644,.F.);
#18489=ORIENTED_EDGE('',*,*,#13668,.T.);
#18490=ORIENTED_EDGE('',*,*,#13669,.F.);
#18491=ORIENTED_EDGE('',*,*,#13670,.F.);
#18492=ORIENTED_EDGE('',*,*,#13647,.F.);
#18493=ORIENTED_EDGE('',*,*,#13671,.T.);
#18494=ORIENTED_EDGE('',*,*,#13672,.F.);
#18495=ORIENTED_EDGE('',*,*,#13668,.F.);
#18496=ORIENTED_EDGE('',*,*,#13646,.F.);
#18497=ORIENTED_EDGE('',*,*,#13673,.T.);
#18498=ORIENTED_EDGE('',*,*,#13674,.F.);
#18499=ORIENTED_EDGE('',*,*,#13671,.F.);
#18500=ORIENTED_EDGE('',*,*,#13645,.F.);
#18501=ORIENTED_EDGE('',*,*,#13670,.T.);
#18502=ORIENTED_EDGE('',*,*,#13675,.F.);
#18503=ORIENTED_EDGE('',*,*,#13673,.F.);
#18504=ORIENTED_EDGE('',*,*,#13640,.F.);
#18505=ORIENTED_EDGE('',*,*,#13676,.T.);
#18506=ORIENTED_EDGE('',*,*,#13677,.F.);
#18507=ORIENTED_EDGE('',*,*,#13678,.F.);
#18508=ORIENTED_EDGE('',*,*,#13643,.F.);
#18509=ORIENTED_EDGE('',*,*,#13679,.T.);
#18510=ORIENTED_EDGE('',*,*,#13680,.F.);
#18511=ORIENTED_EDGE('',*,*,#13676,.F.);
#18512=ORIENTED_EDGE('',*,*,#13642,.F.);
#18513=ORIENTED_EDGE('',*,*,#13681,.T.);
#18514=ORIENTED_EDGE('',*,*,#13682,.F.);
#18515=ORIENTED_EDGE('',*,*,#13679,.F.);
#18516=ORIENTED_EDGE('',*,*,#13641,.F.);
#18517=ORIENTED_EDGE('',*,*,#13678,.T.);
#18518=ORIENTED_EDGE('',*,*,#13683,.F.);
#18519=ORIENTED_EDGE('',*,*,#13681,.F.);
#18520=ORIENTED_EDGE('',*,*,#13636,.F.);
#18521=ORIENTED_EDGE('',*,*,#13684,.T.);
#18522=ORIENTED_EDGE('',*,*,#13685,.F.);
#18523=ORIENTED_EDGE('',*,*,#13686,.F.);
#18524=ORIENTED_EDGE('',*,*,#13639,.F.);
#18525=ORIENTED_EDGE('',*,*,#13687,.T.);
#18526=ORIENTED_EDGE('',*,*,#13688,.F.);
#18527=ORIENTED_EDGE('',*,*,#13684,.F.);
#18528=ORIENTED_EDGE('',*,*,#13638,.F.);
#18529=ORIENTED_EDGE('',*,*,#13689,.T.);
#18530=ORIENTED_EDGE('',*,*,#13690,.F.);
#18531=ORIENTED_EDGE('',*,*,#13687,.F.);
#18532=ORIENTED_EDGE('',*,*,#13637,.F.);
#18533=ORIENTED_EDGE('',*,*,#13686,.T.);
#18534=ORIENTED_EDGE('',*,*,#13691,.F.);
#18535=ORIENTED_EDGE('',*,*,#13689,.F.);
#18536=ORIENTED_EDGE('',*,*,#13632,.F.);
#18537=ORIENTED_EDGE('',*,*,#13692,.T.);
#18538=ORIENTED_EDGE('',*,*,#13693,.F.);
#18539=ORIENTED_EDGE('',*,*,#13694,.F.);
#18540=ORIENTED_EDGE('',*,*,#13635,.F.);
#18541=ORIENTED_EDGE('',*,*,#13695,.T.);
#18542=ORIENTED_EDGE('',*,*,#13696,.F.);
#18543=ORIENTED_EDGE('',*,*,#13692,.F.);
#18544=ORIENTED_EDGE('',*,*,#13634,.F.);
#18545=ORIENTED_EDGE('',*,*,#13697,.T.);
#18546=ORIENTED_EDGE('',*,*,#13698,.F.);
#18547=ORIENTED_EDGE('',*,*,#13695,.F.);
#18548=ORIENTED_EDGE('',*,*,#13633,.F.);
#18549=ORIENTED_EDGE('',*,*,#13694,.T.);
#18550=ORIENTED_EDGE('',*,*,#13699,.F.);
#18551=ORIENTED_EDGE('',*,*,#13697,.F.);
#18552=ORIENTED_EDGE('',*,*,#13628,.F.);
#18553=ORIENTED_EDGE('',*,*,#13700,.T.);
#18554=ORIENTED_EDGE('',*,*,#13701,.F.);
#18555=ORIENTED_EDGE('',*,*,#13702,.F.);
#18556=ORIENTED_EDGE('',*,*,#13631,.F.);
#18557=ORIENTED_EDGE('',*,*,#13703,.T.);
#18558=ORIENTED_EDGE('',*,*,#13704,.F.);
#18559=ORIENTED_EDGE('',*,*,#13700,.F.);
#18560=ORIENTED_EDGE('',*,*,#13630,.F.);
#18561=ORIENTED_EDGE('',*,*,#13705,.T.);
#18562=ORIENTED_EDGE('',*,*,#13706,.F.);
#18563=ORIENTED_EDGE('',*,*,#13703,.F.);
#18564=ORIENTED_EDGE('',*,*,#13629,.F.);
#18565=ORIENTED_EDGE('',*,*,#13702,.T.);
#18566=ORIENTED_EDGE('',*,*,#13707,.F.);
#18567=ORIENTED_EDGE('',*,*,#13705,.F.);
#18568=ORIENTED_EDGE('',*,*,#13708,.T.);
#18569=ORIENTED_EDGE('',*,*,#13709,.T.);
#18570=ORIENTED_EDGE('',*,*,#13627,.F.);
#18571=ORIENTED_EDGE('',*,*,#13709,.F.);
#18572=ORIENTED_EDGE('',*,*,#13615,.T.);
#18573=ORIENTED_EDGE('',*,*,#13653,.T.);
#18574=ORIENTED_EDGE('',*,*,#13621,.T.);
#18575=ORIENTED_EDGE('',*,*,#13623,.T.);
#18576=ORIENTED_EDGE('',*,*,#13654,.T.);
#18577=ORIENTED_EDGE('',*,*,#13658,.T.);
#18578=ORIENTED_EDGE('',*,*,#13708,.F.);
#18579=ORIENTED_EDGE('',*,*,#13701,.T.);
#18580=ORIENTED_EDGE('',*,*,#13704,.T.);
#18581=ORIENTED_EDGE('',*,*,#13706,.T.);
#18582=ORIENTED_EDGE('',*,*,#13707,.T.);
#18583=ORIENTED_EDGE('',*,*,#13693,.T.);
#18584=ORIENTED_EDGE('',*,*,#13696,.T.);
#18585=ORIENTED_EDGE('',*,*,#13698,.T.);
#18586=ORIENTED_EDGE('',*,*,#13699,.T.);
#18587=ORIENTED_EDGE('',*,*,#13685,.T.);
#18588=ORIENTED_EDGE('',*,*,#13688,.T.);
#18589=ORIENTED_EDGE('',*,*,#13690,.T.);
#18590=ORIENTED_EDGE('',*,*,#13691,.T.);
#18591=ORIENTED_EDGE('',*,*,#13677,.T.);
#18592=ORIENTED_EDGE('',*,*,#13680,.T.);
#18593=ORIENTED_EDGE('',*,*,#13682,.T.);
#18594=ORIENTED_EDGE('',*,*,#13683,.T.);
#18595=ORIENTED_EDGE('',*,*,#13669,.T.);
#18596=ORIENTED_EDGE('',*,*,#13672,.T.);
#18597=ORIENTED_EDGE('',*,*,#13674,.T.);
#18598=ORIENTED_EDGE('',*,*,#13675,.T.);
#18599=ORIENTED_EDGE('',*,*,#13661,.T.);
#18600=ORIENTED_EDGE('',*,*,#13664,.T.);
#18601=ORIENTED_EDGE('',*,*,#13666,.T.);
#18602=ORIENTED_EDGE('',*,*,#13667,.T.);
#18603=ORIENTED_EDGE('',*,*,#13656,.T.);
#18604=ORIENTED_EDGE('',*,*,#13710,.T.);
#18605=ORIENTED_EDGE('',*,*,#13711,.T.);
#18606=ORIENTED_EDGE('',*,*,#13712,.T.);
#18607=ORIENTED_EDGE('',*,*,#13713,.T.);
#18608=ORIENTED_EDGE('',*,*,#13711,.F.);
#18609=ORIENTED_EDGE('',*,*,#13714,.T.);
#18610=ORIENTED_EDGE('',*,*,#13715,.F.);
#18611=ORIENTED_EDGE('',*,*,#13716,.F.);
#18612=ORIENTED_EDGE('',*,*,#13710,.F.);
#18613=ORIENTED_EDGE('',*,*,#13717,.T.);
#18614=ORIENTED_EDGE('',*,*,#13718,.F.);
#18615=ORIENTED_EDGE('',*,*,#13719,.T.);
#18616=ORIENTED_EDGE('',*,*,#13720,.F.);
#18617=ORIENTED_EDGE('',*,*,#13721,.F.);
#18618=ORIENTED_EDGE('',*,*,#13722,.F.);
#18619=ORIENTED_EDGE('',*,*,#13723,.F.);
#18620=ORIENTED_EDGE('',*,*,#13724,.F.);
#18621=ORIENTED_EDGE('',*,*,#13725,.T.);
#18622=ORIENTED_EDGE('',*,*,#13726,.F.);
#18623=ORIENTED_EDGE('',*,*,#13727,.T.);
#18624=ORIENTED_EDGE('',*,*,#13728,.F.);
#18625=ORIENTED_EDGE('',*,*,#13729,.T.);
#18626=ORIENTED_EDGE('',*,*,#13730,.F.);
#18627=ORIENTED_EDGE('',*,*,#13714,.F.);
#18628=ORIENTED_EDGE('',*,*,#13722,.T.);
#18629=ORIENTED_EDGE('',*,*,#13731,.T.);
#18630=ORIENTED_EDGE('',*,*,#13732,.T.);
#18631=ORIENTED_EDGE('',*,*,#13733,.T.);
#18632=ORIENTED_EDGE('',*,*,#13733,.F.);
#18633=ORIENTED_EDGE('',*,*,#13734,.F.);
#18634=ORIENTED_EDGE('',*,*,#13735,.F.);
#18635=ORIENTED_EDGE('',*,*,#13723,.T.);
#18636=ORIENTED_EDGE('',*,*,#13712,.F.);
#18637=ORIENTED_EDGE('',*,*,#13716,.T.);
#18638=ORIENTED_EDGE('',*,*,#13736,.F.);
#18639=ORIENTED_EDGE('',*,*,#13737,.T.);
#18640=ORIENTED_EDGE('',*,*,#13738,.F.);
#18641=ORIENTED_EDGE('',*,*,#13739,.T.);
#18642=ORIENTED_EDGE('',*,*,#13740,.F.);
#18643=ORIENTED_EDGE('',*,*,#13741,.T.);
#18644=ORIENTED_EDGE('',*,*,#13742,.F.);
#18645=ORIENTED_EDGE('',*,*,#13734,.T.);
#18646=ORIENTED_EDGE('',*,*,#13732,.F.);
#18647=ORIENTED_EDGE('',*,*,#13743,.F.);
#18648=ORIENTED_EDGE('',*,*,#13744,.F.);
#18649=ORIENTED_EDGE('',*,*,#13745,.F.);
#18650=ORIENTED_EDGE('',*,*,#13746,.F.);
#18651=ORIENTED_EDGE('',*,*,#13747,.T.);
#18652=ORIENTED_EDGE('',*,*,#13736,.T.);
#18653=ORIENTED_EDGE('',*,*,#13715,.T.);
#18654=ORIENTED_EDGE('',*,*,#13730,.T.);
#18655=ORIENTED_EDGE('',*,*,#13748,.T.);
#18656=ORIENTED_EDGE('',*,*,#13748,.F.);
#18657=ORIENTED_EDGE('',*,*,#13729,.F.);
#18658=ORIENTED_EDGE('',*,*,#13749,.F.);
#18659=ORIENTED_EDGE('',*,*,#13737,.F.);
#18660=ORIENTED_EDGE('',*,*,#13750,.T.);
#18661=ORIENTED_EDGE('',*,*,#13751,.T.);
#18662=ORIENTED_EDGE('',*,*,#13752,.T.);
#18663=ORIENTED_EDGE('',*,*,#13753,.T.);
#18664=ORIENTED_EDGE('',*,*,#13728,.T.);
#18665=ORIENTED_EDGE('',*,*,#13754,.T.);
#18666=ORIENTED_EDGE('',*,*,#13738,.T.);
#18667=ORIENTED_EDGE('',*,*,#13749,.T.);
#18668=ORIENTED_EDGE('',*,*,#13754,.F.);
#18669=ORIENTED_EDGE('',*,*,#13727,.F.);
#18670=ORIENTED_EDGE('',*,*,#13755,.F.);
#18671=ORIENTED_EDGE('',*,*,#13739,.F.);
#18672=ORIENTED_EDGE('',*,*,#13724,.T.);
#18673=ORIENTED_EDGE('',*,*,#13735,.T.);
#18674=ORIENTED_EDGE('',*,*,#13742,.T.);
#18675=ORIENTED_EDGE('',*,*,#13756,.T.);
#18676=ORIENTED_EDGE('',*,*,#13756,.F.);
#18677=ORIENTED_EDGE('',*,*,#13741,.F.);
#18678=ORIENTED_EDGE('',*,*,#13757,.F.);
#18679=ORIENTED_EDGE('',*,*,#13725,.F.);
#18680=ORIENTED_EDGE('',*,*,#13758,.T.);
#18681=ORIENTED_EDGE('',*,*,#13759,.T.);
#18682=ORIENTED_EDGE('',*,*,#13760,.T.);
#18683=ORIENTED_EDGE('',*,*,#13761,.T.);
#18684=ORIENTED_EDGE('',*,*,#13726,.T.);
#18685=ORIENTED_EDGE('',*,*,#13757,.T.);
#18686=ORIENTED_EDGE('',*,*,#13740,.T.);
#18687=ORIENTED_EDGE('',*,*,#13755,.T.);
#18688=ORIENTED_EDGE('',*,*,#13720,.T.);
#18689=ORIENTED_EDGE('',*,*,#13762,.T.);
#18690=ORIENTED_EDGE('',*,*,#13744,.T.);
#18691=ORIENTED_EDGE('',*,*,#13763,.T.);
#18692=ORIENTED_EDGE('',*,*,#13764,.T.);
#18693=ORIENTED_EDGE('',*,*,#13765,.T.);
#18694=ORIENTED_EDGE('',*,*,#13766,.F.);
#18695=ORIENTED_EDGE('',*,*,#13767,.F.);
#18696=ORIENTED_EDGE('',*,*,#13768,.T.);
#18697=ORIENTED_EDGE('',*,*,#13769,.T.);
#18698=ORIENTED_EDGE('',*,*,#13745,.T.);
#18699=ORIENTED_EDGE('',*,*,#13762,.F.);
#18700=ORIENTED_EDGE('',*,*,#13719,.F.);
#18701=ORIENTED_EDGE('',*,*,#13770,.F.);
#18702=ORIENTED_EDGE('',*,*,#13718,.T.);
#18703=ORIENTED_EDGE('',*,*,#13771,.T.);
#18704=ORIENTED_EDGE('',*,*,#13746,.T.);
#18705=ORIENTED_EDGE('',*,*,#13770,.T.);
#18706=ORIENTED_EDGE('',*,*,#13713,.F.);
#18707=ORIENTED_EDGE('',*,*,#13747,.F.);
#18708=ORIENTED_EDGE('',*,*,#13771,.F.);
#18709=ORIENTED_EDGE('',*,*,#13717,.F.);
#18710=ORIENTED_EDGE('',*,*,#13772,.F.);
#18711=ORIENTED_EDGE('',*,*,#13773,.T.);
#18712=ORIENTED_EDGE('',*,*,#13769,.F.);
#18713=ORIENTED_EDGE('',*,*,#13773,.F.);
#18714=ORIENTED_EDGE('',*,*,#13774,.F.);
#18715=ORIENTED_EDGE('',*,*,#13775,.T.);
#18716=ORIENTED_EDGE('',*,*,#13768,.F.);
#18717=ORIENTED_EDGE('',*,*,#13775,.F.);
#18718=ORIENTED_EDGE('',*,*,#13776,.T.);
#18719=ORIENTED_EDGE('',*,*,#13767,.T.);
#18720=ORIENTED_EDGE('',*,*,#13777,.F.);
#18721=ORIENTED_EDGE('',*,*,#13778,.F.);
#18722=ORIENTED_EDGE('',*,*,#13779,.T.);
#18723=ORIENTED_EDGE('',*,*,#13778,.T.);
#18724=ORIENTED_EDGE('',*,*,#13780,.F.);
#18725=ORIENTED_EDGE('',*,*,#13781,.F.);
#18726=ORIENTED_EDGE('',*,*,#13772,.T.);
#18727=ORIENTED_EDGE('',*,*,#13774,.T.);
#18728=ORIENTED_EDGE('',*,*,#13782,.T.);
#18729=ORIENTED_EDGE('',*,*,#13781,.T.);
#18730=ORIENTED_EDGE('',*,*,#13783,.F.);
#18731=ORIENTED_EDGE('',*,*,#13765,.F.);
#18732=ORIENTED_EDGE('',*,*,#13766,.T.);
#18733=ORIENTED_EDGE('',*,*,#13783,.T.);
#18734=ORIENTED_EDGE('',*,*,#13780,.T.);
#18735=ORIENTED_EDGE('',*,*,#13777,.T.);
#18736=ORIENTED_EDGE('',*,*,#13764,.F.);
#18737=ORIENTED_EDGE('',*,*,#13776,.F.);
#18738=ORIENTED_EDGE('',*,*,#13779,.F.);
#18739=ORIENTED_EDGE('',*,*,#13782,.F.);
#18740=ORIENTED_EDGE('',*,*,#13784,.F.);
#18741=ORIENTED_EDGE('',*,*,#13785,.T.);
#18742=ORIENTED_EDGE('',*,*,#13750,.F.);
#18743=ORIENTED_EDGE('',*,*,#13786,.F.);
#18744=ORIENTED_EDGE('',*,*,#13787,.F.);
#18745=ORIENTED_EDGE('',*,*,#13788,.T.);
#18746=ORIENTED_EDGE('',*,*,#13751,.F.);
#18747=ORIENTED_EDGE('',*,*,#13785,.F.);
#18748=ORIENTED_EDGE('',*,*,#13789,.F.);
#18749=ORIENTED_EDGE('',*,*,#13790,.T.);
#18750=ORIENTED_EDGE('',*,*,#13752,.F.);
#18751=ORIENTED_EDGE('',*,*,#13788,.F.);
#18752=ORIENTED_EDGE('',*,*,#13791,.F.);
#18753=ORIENTED_EDGE('',*,*,#13786,.T.);
#18754=ORIENTED_EDGE('',*,*,#13753,.F.);
#18755=ORIENTED_EDGE('',*,*,#13790,.F.);
#18756=ORIENTED_EDGE('',*,*,#13791,.T.);
#18757=ORIENTED_EDGE('',*,*,#13789,.T.);
#18758=ORIENTED_EDGE('',*,*,#13787,.T.);
#18759=ORIENTED_EDGE('',*,*,#13784,.T.);
#18760=ORIENTED_EDGE('',*,*,#13758,.F.);
#18761=ORIENTED_EDGE('',*,*,#13792,.T.);
#18762=ORIENTED_EDGE('',*,*,#13793,.T.);
#18763=ORIENTED_EDGE('',*,*,#13794,.F.);
#18764=ORIENTED_EDGE('',*,*,#13761,.F.);
#18765=ORIENTED_EDGE('',*,*,#13795,.T.);
#18766=ORIENTED_EDGE('',*,*,#13796,.T.);
#18767=ORIENTED_EDGE('',*,*,#13792,.F.);
#18768=ORIENTED_EDGE('',*,*,#13760,.F.);
#18769=ORIENTED_EDGE('',*,*,#13797,.T.);
#18770=ORIENTED_EDGE('',*,*,#13798,.T.);
#18771=ORIENTED_EDGE('',*,*,#13795,.F.);
#18772=ORIENTED_EDGE('',*,*,#13759,.F.);
#18773=ORIENTED_EDGE('',*,*,#13794,.T.);
#18774=ORIENTED_EDGE('',*,*,#13799,.T.);
#18775=ORIENTED_EDGE('',*,*,#13797,.F.);
#18776=ORIENTED_EDGE('',*,*,#13799,.F.);
#18777=ORIENTED_EDGE('',*,*,#13793,.F.);
#18778=ORIENTED_EDGE('',*,*,#13796,.F.);
#18779=ORIENTED_EDGE('',*,*,#13798,.F.);
#18780=ORIENTED_EDGE('',*,*,#13731,.F.);
#18781=ORIENTED_EDGE('',*,*,#13721,.T.);
#18782=ORIENTED_EDGE('',*,*,#13763,.F.);
#18783=ORIENTED_EDGE('',*,*,#13743,.T.);
#18784=ORIENTED_EDGE('',*,*,#13800,.T.);
#18785=ORIENTED_EDGE('',*,*,#13801,.T.);
#18786=ORIENTED_EDGE('',*,*,#13802,.T.);
#18787=ORIENTED_EDGE('',*,*,#13803,.T.);
#18788=ORIENTED_EDGE('',*,*,#13800,.F.);
#18789=ORIENTED_EDGE('',*,*,#13804,.T.);
#18790=ORIENTED_EDGE('',*,*,#13805,.F.);
#18791=ORIENTED_EDGE('',*,*,#13806,.T.);
#18792=ORIENTED_EDGE('',*,*,#13807,.F.);
#18793=ORIENTED_EDGE('',*,*,#13808,.T.);
#18794=ORIENTED_EDGE('',*,*,#13809,.T.);
#18795=ORIENTED_EDGE('',*,*,#13810,.T.);
#18796=ORIENTED_EDGE('',*,*,#13811,.T.);
#18797=ORIENTED_EDGE('',*,*,#13812,.T.);
#18798=ORIENTED_EDGE('',*,*,#13813,.F.);
#18799=ORIENTED_EDGE('',*,*,#13814,.T.);
#18800=ORIENTED_EDGE('',*,*,#13803,.F.);
#18801=ORIENTED_EDGE('',*,*,#13815,.T.);
#18802=ORIENTED_EDGE('',*,*,#13816,.F.);
#18803=ORIENTED_EDGE('',*,*,#13804,.F.);
#18804=ORIENTED_EDGE('',*,*,#13805,.T.);
#18805=ORIENTED_EDGE('',*,*,#13816,.T.);
#18806=ORIENTED_EDGE('',*,*,#13817,.T.);
#18807=ORIENTED_EDGE('',*,*,#13818,.T.);
#18808=ORIENTED_EDGE('',*,*,#13819,.F.);
#18809=ORIENTED_EDGE('',*,*,#13820,.T.);
#18810=ORIENTED_EDGE('',*,*,#13821,.F.);
#18811=ORIENTED_EDGE('',*,*,#13820,.F.);
#18812=ORIENTED_EDGE('',*,*,#13822,.F.);
#18813=ORIENTED_EDGE('',*,*,#13823,.T.);
#18814=ORIENTED_EDGE('',*,*,#13824,.F.);
#18815=ORIENTED_EDGE('',*,*,#13823,.F.);
#18816=ORIENTED_EDGE('',*,*,#13811,.F.);
#18817=ORIENTED_EDGE('',*,*,#13825,.T.);
#18818=ORIENTED_EDGE('',*,*,#13826,.F.);
#18819=ORIENTED_EDGE('',*,*,#13827,.F.);
#18820=ORIENTED_EDGE('',*,*,#13810,.F.);
#18821=ORIENTED_EDGE('',*,*,#13828,.T.);
#18822=ORIENTED_EDGE('',*,*,#13829,.F.);
#18823=ORIENTED_EDGE('',*,*,#13825,.F.);
#18824=ORIENTED_EDGE('',*,*,#13809,.F.);
#18825=ORIENTED_EDGE('',*,*,#13830,.T.);
#18826=ORIENTED_EDGE('',*,*,#13831,.F.);
#18827=ORIENTED_EDGE('',*,*,#13828,.F.);
#18828=ORIENTED_EDGE('',*,*,#13808,.F.);
#18829=ORIENTED_EDGE('',*,*,#13832,.T.);
#18830=ORIENTED_EDGE('',*,*,#13812,.F.);
#18831=ORIENTED_EDGE('',*,*,#13827,.T.);
#18832=ORIENTED_EDGE('',*,*,#13833,.F.);
#18833=ORIENTED_EDGE('',*,*,#13830,.F.);
#18834=ORIENTED_EDGE('',*,*,#13834,.F.);
#18835=ORIENTED_EDGE('',*,*,#13832,.F.);
#18836=ORIENTED_EDGE('',*,*,#13835,.T.);
#18837=ORIENTED_EDGE('',*,*,#13813,.T.);
#18838=ORIENTED_EDGE('',*,*,#13834,.T.);
#18839=ORIENTED_EDGE('',*,*,#13807,.T.);
#18840=ORIENTED_EDGE('',*,*,#13836,.T.);
#18841=ORIENTED_EDGE('',*,*,#13837,.T.);
#18842=ORIENTED_EDGE('',*,*,#13818,.F.);
#18843=ORIENTED_EDGE('',*,*,#13838,.T.);
#18844=ORIENTED_EDGE('',*,*,#13839,.F.);
#18845=ORIENTED_EDGE('',*,*,#13836,.F.);
#18846=ORIENTED_EDGE('',*,*,#13806,.F.);
#18847=ORIENTED_EDGE('',*,*,#13801,.F.);
#18848=ORIENTED_EDGE('',*,*,#13814,.F.);
#18849=ORIENTED_EDGE('',*,*,#13835,.F.);
#18850=ORIENTED_EDGE('',*,*,#13840,.F.);
#18851=ORIENTED_EDGE('',*,*,#13841,.T.);
#18852=ORIENTED_EDGE('',*,*,#13842,.T.);
#18853=ORIENTED_EDGE('',*,*,#13843,.T.);
#18854=ORIENTED_EDGE('',*,*,#13844,.F.);
#18855=ORIENTED_EDGE('',*,*,#13845,.F.);
#18856=ORIENTED_EDGE('',*,*,#13839,.T.);
#18857=ORIENTED_EDGE('',*,*,#13846,.T.);
#18858=ORIENTED_EDGE('',*,*,#13845,.T.);
#18859=ORIENTED_EDGE('',*,*,#13847,.F.);
#18860=ORIENTED_EDGE('',*,*,#13848,.F.);
#18861=ORIENTED_EDGE('',*,*,#13849,.T.);
#18862=ORIENTED_EDGE('',*,*,#13840,.T.);
#18863=ORIENTED_EDGE('',*,*,#13837,.F.);
#18864=ORIENTED_EDGE('',*,*,#13819,.T.);
#18865=ORIENTED_EDGE('',*,*,#13822,.T.);
#18866=ORIENTED_EDGE('',*,*,#13850,.T.);
#18867=ORIENTED_EDGE('',*,*,#13848,.T.);
#18868=ORIENTED_EDGE('',*,*,#13851,.F.);
#18869=ORIENTED_EDGE('',*,*,#13852,.F.);
#18870=ORIENTED_EDGE('',*,*,#13853,.T.);
#18871=ORIENTED_EDGE('',*,*,#13852,.T.);
#18872=ORIENTED_EDGE('',*,*,#13854,.F.);
#18873=ORIENTED_EDGE('',*,*,#13843,.F.);
#18874=ORIENTED_EDGE('',*,*,#13821,.T.);
#18875=ORIENTED_EDGE('',*,*,#13824,.T.);
#18876=ORIENTED_EDGE('',*,*,#13854,.T.);
#18877=ORIENTED_EDGE('',*,*,#13851,.T.);
#18878=ORIENTED_EDGE('',*,*,#13847,.T.);
#18879=ORIENTED_EDGE('',*,*,#13844,.T.);
#18880=ORIENTED_EDGE('',*,*,#13802,.F.);
#18881=ORIENTED_EDGE('',*,*,#13841,.F.);
#18882=ORIENTED_EDGE('',*,*,#13849,.F.);
#18883=ORIENTED_EDGE('',*,*,#13850,.F.);
#18884=ORIENTED_EDGE('',*,*,#13853,.F.);
#18885=ORIENTED_EDGE('',*,*,#13842,.F.);
#18886=ORIENTED_EDGE('',*,*,#13846,.F.);
#18887=ORIENTED_EDGE('',*,*,#13838,.F.);
#18888=ORIENTED_EDGE('',*,*,#13817,.F.);
#18889=ORIENTED_EDGE('',*,*,#13815,.F.);
#18890=ORIENTED_EDGE('',*,*,#13826,.T.);
#18891=ORIENTED_EDGE('',*,*,#13829,.T.);
#18892=ORIENTED_EDGE('',*,*,#13831,.T.);
#18893=ORIENTED_EDGE('',*,*,#13833,.T.);
#18894=ORIENTED_EDGE('',*,*,#13855,.F.);
#18895=ORIENTED_EDGE('',*,*,#13856,.T.);
#18896=ORIENTED_EDGE('',*,*,#13857,.F.);
#18897=ORIENTED_EDGE('',*,*,#13858,.F.);
#18898=ORIENTED_EDGE('',*,*,#13859,.F.);
#18899=ORIENTED_EDGE('',*,*,#13858,.T.);
#18900=ORIENTED_EDGE('',*,*,#13860,.F.);
#18901=ORIENTED_EDGE('',*,*,#13861,.F.);
#18902=ORIENTED_EDGE('',*,*,#13862,.F.);
#18903=ORIENTED_EDGE('',*,*,#13861,.T.);
#18904=ORIENTED_EDGE('',*,*,#13863,.F.);
#18905=ORIENTED_EDGE('',*,*,#13864,.F.);
#18906=ORIENTED_EDGE('',*,*,#13865,.F.);
#18907=ORIENTED_EDGE('',*,*,#13864,.T.);
#18908=ORIENTED_EDGE('',*,*,#13866,.F.);
#18909=ORIENTED_EDGE('',*,*,#13856,.F.);
#18910=ORIENTED_EDGE('',*,*,#13866,.T.);
#18911=ORIENTED_EDGE('',*,*,#13863,.T.);
#18912=ORIENTED_EDGE('',*,*,#13860,.T.);
#18913=ORIENTED_EDGE('',*,*,#13857,.T.);
#18914=ORIENTED_EDGE('',*,*,#13867,.F.);
#18915=ORIENTED_EDGE('',*,*,#13868,.T.);
#18916=ORIENTED_EDGE('',*,*,#13869,.F.);
#18917=ORIENTED_EDGE('',*,*,#13870,.F.);
#18918=ORIENTED_EDGE('',*,*,#13871,.F.);
#18919=ORIENTED_EDGE('',*,*,#13870,.T.);
#18920=ORIENTED_EDGE('',*,*,#13872,.F.);
#18921=ORIENTED_EDGE('',*,*,#13873,.F.);
#18922=ORIENTED_EDGE('',*,*,#13874,.F.);
#18923=ORIENTED_EDGE('',*,*,#13873,.T.);
#18924=ORIENTED_EDGE('',*,*,#13875,.F.);
#18925=ORIENTED_EDGE('',*,*,#13876,.F.);
#18926=ORIENTED_EDGE('',*,*,#13877,.F.);
#18927=ORIENTED_EDGE('',*,*,#13876,.T.);
#18928=ORIENTED_EDGE('',*,*,#13878,.F.);
#18929=ORIENTED_EDGE('',*,*,#13868,.F.);
#18930=ORIENTED_EDGE('',*,*,#13878,.T.);
#18931=ORIENTED_EDGE('',*,*,#13875,.T.);
#18932=ORIENTED_EDGE('',*,*,#13872,.T.);
#18933=ORIENTED_EDGE('',*,*,#13869,.T.);
#18934=ORIENTED_EDGE('',*,*,#13879,.F.);
#18935=ORIENTED_EDGE('',*,*,#13880,.T.);
#18936=ORIENTED_EDGE('',*,*,#13881,.F.);
#18937=ORIENTED_EDGE('',*,*,#13880,.F.);
#18938=ORIENTED_EDGE('',*,*,#13879,.T.);
#18939=ORIENTED_EDGE('',*,*,#13882,.F.);
#18940=ORIENTED_EDGE('',*,*,#13883,.T.);
#18941=ORIENTED_EDGE('',*,*,#13884,.F.);
#18942=ORIENTED_EDGE('',*,*,#13885,.F.);
#18943=ORIENTED_EDGE('',*,*,#13886,.F.);
#18944=ORIENTED_EDGE('',*,*,#13885,.T.);
#18945=ORIENTED_EDGE('',*,*,#13887,.F.);
#18946=ORIENTED_EDGE('',*,*,#13888,.F.);
#18947=ORIENTED_EDGE('',*,*,#13889,.F.);
#18948=ORIENTED_EDGE('',*,*,#13888,.T.);
#18949=ORIENTED_EDGE('',*,*,#13890,.F.);
#18950=ORIENTED_EDGE('',*,*,#13891,.F.);
#18951=ORIENTED_EDGE('',*,*,#13892,.F.);
#18952=ORIENTED_EDGE('',*,*,#13891,.T.);
#18953=ORIENTED_EDGE('',*,*,#13893,.F.);
#18954=ORIENTED_EDGE('',*,*,#13883,.F.);
#18955=ORIENTED_EDGE('',*,*,#13893,.T.);
#18956=ORIENTED_EDGE('',*,*,#13890,.T.);
#18957=ORIENTED_EDGE('',*,*,#13887,.T.);
#18958=ORIENTED_EDGE('',*,*,#13884,.T.);
#18959=ORIENTED_EDGE('',*,*,#13894,.F.);
#18960=ORIENTED_EDGE('',*,*,#13895,.T.);
#18961=ORIENTED_EDGE('',*,*,#13896,.F.);
#18962=ORIENTED_EDGE('',*,*,#13897,.F.);
#18963=ORIENTED_EDGE('',*,*,#13898,.F.);
#18964=ORIENTED_EDGE('',*,*,#13897,.T.);
#18965=ORIENTED_EDGE('',*,*,#13899,.F.);
#18966=ORIENTED_EDGE('',*,*,#13900,.F.);
#18967=ORIENTED_EDGE('',*,*,#13901,.F.);
#18968=ORIENTED_EDGE('',*,*,#13900,.T.);
#18969=ORIENTED_EDGE('',*,*,#13902,.F.);
#18970=ORIENTED_EDGE('',*,*,#13903,.F.);
#18971=ORIENTED_EDGE('',*,*,#13904,.F.);
#18972=ORIENTED_EDGE('',*,*,#13903,.T.);
#18973=ORIENTED_EDGE('',*,*,#13905,.F.);
#18974=ORIENTED_EDGE('',*,*,#13895,.F.);
#18975=ORIENTED_EDGE('',*,*,#13905,.T.);
#18976=ORIENTED_EDGE('',*,*,#13902,.T.);
#18977=ORIENTED_EDGE('',*,*,#13899,.T.);
#18978=ORIENTED_EDGE('',*,*,#13896,.T.);
#18979=ORIENTED_EDGE('',*,*,#13906,.F.);
#18980=ORIENTED_EDGE('',*,*,#13907,.T.);
#18981=ORIENTED_EDGE('',*,*,#13908,.F.);
#18982=ORIENTED_EDGE('',*,*,#13909,.F.);
#18983=ORIENTED_EDGE('',*,*,#13910,.F.);
#18984=ORIENTED_EDGE('',*,*,#13909,.T.);
#18985=ORIENTED_EDGE('',*,*,#13911,.F.);
#18986=ORIENTED_EDGE('',*,*,#13912,.F.);
#18987=ORIENTED_EDGE('',*,*,#13913,.F.);
#18988=ORIENTED_EDGE('',*,*,#13912,.T.);
#18989=ORIENTED_EDGE('',*,*,#13914,.F.);
#18990=ORIENTED_EDGE('',*,*,#13915,.F.);
#18991=ORIENTED_EDGE('',*,*,#13916,.F.);
#18992=ORIENTED_EDGE('',*,*,#13915,.T.);
#18993=ORIENTED_EDGE('',*,*,#13917,.F.);
#18994=ORIENTED_EDGE('',*,*,#13907,.F.);
#18995=ORIENTED_EDGE('',*,*,#13917,.T.);
#18996=ORIENTED_EDGE('',*,*,#13914,.T.);
#18997=ORIENTED_EDGE('',*,*,#13911,.T.);
#18998=ORIENTED_EDGE('',*,*,#13908,.T.);
#18999=ORIENTED_EDGE('',*,*,#13918,.F.);
#19000=ORIENTED_EDGE('',*,*,#13919,.T.);
#19001=ORIENTED_EDGE('',*,*,#13920,.F.);
#19002=ORIENTED_EDGE('',*,*,#13921,.F.);
#19003=ORIENTED_EDGE('',*,*,#13922,.F.);
#19004=ORIENTED_EDGE('',*,*,#13921,.T.);
#19005=ORIENTED_EDGE('',*,*,#13923,.F.);
#19006=ORIENTED_EDGE('',*,*,#13924,.F.);
#19007=ORIENTED_EDGE('',*,*,#13925,.F.);
#19008=ORIENTED_EDGE('',*,*,#13924,.T.);
#19009=ORIENTED_EDGE('',*,*,#13926,.F.);
#19010=ORIENTED_EDGE('',*,*,#13927,.F.);
#19011=ORIENTED_EDGE('',*,*,#13928,.F.);
#19012=ORIENTED_EDGE('',*,*,#13927,.T.);
#19013=ORIENTED_EDGE('',*,*,#13929,.F.);
#19014=ORIENTED_EDGE('',*,*,#13919,.F.);
#19015=ORIENTED_EDGE('',*,*,#13929,.T.);
#19016=ORIENTED_EDGE('',*,*,#13926,.T.);
#19017=ORIENTED_EDGE('',*,*,#13923,.T.);
#19018=ORIENTED_EDGE('',*,*,#13920,.T.);
#19019=ORIENTED_EDGE('',*,*,#13930,.F.);
#19020=ORIENTED_EDGE('',*,*,#13931,.T.);
#19021=ORIENTED_EDGE('',*,*,#13932,.F.);
#19022=ORIENTED_EDGE('',*,*,#13931,.F.);
#19023=ORIENTED_EDGE('',*,*,#13933,.F.);
#19024=ORIENTED_EDGE('',*,*,#13934,.T.);
#19025=ORIENTED_EDGE('',*,*,#13935,.F.);
#19026=ORIENTED_EDGE('',*,*,#13934,.F.);
#19027=ORIENTED_EDGE('',*,*,#13936,.F.);
#19028=ORIENTED_EDGE('',*,*,#13937,.T.);
#19029=ORIENTED_EDGE('',*,*,#13938,.F.);
#19030=ORIENTED_EDGE('',*,*,#13937,.F.);
#19031=ORIENTED_EDGE('',*,*,#13939,.T.);
#19032=ORIENTED_EDGE('',*,*,#13940,.T.);
#19033=ORIENTED_EDGE('',*,*,#13941,.F.);
#19034=ORIENTED_EDGE('',*,*,#13940,.F.);
#19035=ORIENTED_EDGE('',*,*,#13942,.F.);
#19036=ORIENTED_EDGE('',*,*,#13930,.T.);
#19037=ORIENTED_EDGE('',*,*,#13933,.T.);
#19038=ORIENTED_EDGE('',*,*,#13936,.T.);
#19039=ORIENTED_EDGE('',*,*,#13941,.T.);
#19040=ORIENTED_EDGE('',*,*,#13943,.F.);
#19041=ORIENTED_EDGE('',*,*,#13944,.T.);
#19042=ORIENTED_EDGE('',*,*,#13942,.T.);
#19043=ORIENTED_EDGE('',*,*,#13944,.F.);
#19044=ORIENTED_EDGE('',*,*,#13943,.T.);
#19045=ORIENTED_EDGE('',*,*,#13867,.T.);
#19046=ORIENTED_EDGE('',*,*,#13871,.T.);
#19047=ORIENTED_EDGE('',*,*,#13874,.T.);
#19048=ORIENTED_EDGE('',*,*,#13877,.T.);
#19049=ORIENTED_EDGE('',*,*,#13882,.T.);
#19050=ORIENTED_EDGE('',*,*,#13886,.T.);
#19051=ORIENTED_EDGE('',*,*,#13889,.T.);
#19052=ORIENTED_EDGE('',*,*,#13892,.T.);
#19053=ORIENTED_EDGE('',*,*,#13894,.T.);
#19054=ORIENTED_EDGE('',*,*,#13898,.T.);
#19055=ORIENTED_EDGE('',*,*,#13901,.T.);
#19056=ORIENTED_EDGE('',*,*,#13904,.T.);
#19057=ORIENTED_EDGE('',*,*,#13906,.T.);
#19058=ORIENTED_EDGE('',*,*,#13910,.T.);
#19059=ORIENTED_EDGE('',*,*,#13913,.T.);
#19060=ORIENTED_EDGE('',*,*,#13916,.T.);
#19061=ORIENTED_EDGE('',*,*,#13918,.T.);
#19062=ORIENTED_EDGE('',*,*,#13922,.T.);
#19063=ORIENTED_EDGE('',*,*,#13925,.T.);
#19064=ORIENTED_EDGE('',*,*,#13928,.T.);
#19065=ORIENTED_EDGE('',*,*,#13932,.T.);
#19066=ORIENTED_EDGE('',*,*,#13935,.T.);
#19067=ORIENTED_EDGE('',*,*,#13938,.T.);
#19068=ORIENTED_EDGE('',*,*,#13939,.F.);
#19069=ORIENTED_EDGE('',*,*,#13881,.T.);
#19070=ORIENTED_EDGE('',*,*,#13855,.T.);
#19071=ORIENTED_EDGE('',*,*,#13859,.T.);
#19072=ORIENTED_EDGE('',*,*,#13862,.T.);
#19073=ORIENTED_EDGE('',*,*,#13865,.T.);
#19074=ORIENTED_EDGE('',*,*,#13945,.F.);
#19075=ORIENTED_EDGE('',*,*,#13946,.T.);
#19076=ORIENTED_EDGE('',*,*,#13947,.T.);
#19077=ORIENTED_EDGE('',*,*,#13948,.T.);
#19078=ORIENTED_EDGE('',*,*,#13947,.F.);
#19079=ORIENTED_EDGE('',*,*,#13949,.T.);
#19080=ORIENTED_EDGE('',*,*,#13950,.T.);
#19081=ORIENTED_EDGE('',*,*,#13951,.T.);
#19082=ORIENTED_EDGE('',*,*,#13952,.F.);
#19083=ORIENTED_EDGE('',*,*,#13953,.T.);
#19084=ORIENTED_EDGE('',*,*,#13945,.T.);
#19085=ORIENTED_EDGE('',*,*,#13954,.T.);
#19086=ORIENTED_EDGE('',*,*,#13955,.F.);
#19087=ORIENTED_EDGE('',*,*,#13956,.T.);
#19088=ORIENTED_EDGE('',*,*,#13952,.T.);
#19089=ORIENTED_EDGE('',*,*,#13957,.T.);
#19090=ORIENTED_EDGE('',*,*,#13958,.F.);
#19091=ORIENTED_EDGE('',*,*,#13959,.T.);
#19092=ORIENTED_EDGE('',*,*,#13960,.F.);
#19093=ORIENTED_EDGE('',*,*,#13961,.F.);
#19094=ORIENTED_EDGE('',*,*,#13962,.F.);
#19095=ORIENTED_EDGE('',*,*,#13963,.T.);
#19096=ORIENTED_EDGE('',*,*,#13958,.T.);
#19097=ORIENTED_EDGE('',*,*,#13964,.F.);
#19098=ORIENTED_EDGE('',*,*,#13965,.F.);
#19099=ORIENTED_EDGE('',*,*,#13966,.T.);
#19100=ORIENTED_EDGE('',*,*,#13962,.T.);
#19101=ORIENTED_EDGE('',*,*,#13967,.F.);
#19102=ORIENTED_EDGE('',*,*,#13968,.F.);
#19103=ORIENTED_EDGE('',*,*,#13969,.T.);
#19104=ORIENTED_EDGE('',*,*,#13965,.T.);
#19105=ORIENTED_EDGE('',*,*,#13970,.F.);
#19106=ORIENTED_EDGE('',*,*,#13960,.T.);
#19107=ORIENTED_EDGE('',*,*,#13971,.T.);
#19108=ORIENTED_EDGE('',*,*,#13972,.F.);
#19109=ORIENTED_EDGE('',*,*,#13973,.F.);
#19110=ORIENTED_EDGE('',*,*,#13974,.T.);
#19111=ORIENTED_EDGE('',*,*,#13974,.F.);
#19112=ORIENTED_EDGE('',*,*,#13975,.F.);
#19113=ORIENTED_EDGE('',*,*,#13957,.F.);
#19114=ORIENTED_EDGE('',*,*,#13954,.F.);
#19115=ORIENTED_EDGE('',*,*,#13951,.F.);
#19116=ORIENTED_EDGE('',*,*,#13976,.F.);
#19117=ORIENTED_EDGE('',*,*,#13977,.T.);
#19118=ORIENTED_EDGE('',*,*,#13970,.T.);
#19119=ORIENTED_EDGE('',*,*,#13967,.T.);
#19120=ORIENTED_EDGE('',*,*,#13964,.T.);
#19121=ORIENTED_EDGE('',*,*,#13961,.T.);
#19122=ORIENTED_EDGE('',*,*,#13950,.F.);
#19123=ORIENTED_EDGE('',*,*,#13978,.T.);
#19124=ORIENTED_EDGE('',*,*,#13979,.T.);
#19125=ORIENTED_EDGE('',*,*,#13976,.T.);
#19126=ORIENTED_EDGE('',*,*,#13968,.T.);
#19127=ORIENTED_EDGE('',*,*,#13977,.F.);
#19128=ORIENTED_EDGE('',*,*,#13979,.F.);
#19129=ORIENTED_EDGE('',*,*,#13980,.T.);
#19130=ORIENTED_EDGE('',*,*,#13971,.F.);
#19131=ORIENTED_EDGE('',*,*,#13959,.F.);
#19132=ORIENTED_EDGE('',*,*,#13963,.F.);
#19133=ORIENTED_EDGE('',*,*,#13966,.F.);
#19134=ORIENTED_EDGE('',*,*,#13969,.F.);
#19135=ORIENTED_EDGE('',*,*,#13980,.F.);
#19136=ORIENTED_EDGE('',*,*,#13978,.F.);
#19137=ORIENTED_EDGE('',*,*,#13949,.F.);
#19138=ORIENTED_EDGE('',*,*,#13946,.F.);
#19139=ORIENTED_EDGE('',*,*,#13953,.F.);
#19140=ORIENTED_EDGE('',*,*,#13956,.F.);
#19141=ORIENTED_EDGE('',*,*,#13981,.F.);
#19142=ORIENTED_EDGE('',*,*,#13955,.T.);
#19143=ORIENTED_EDGE('',*,*,#13975,.T.);
#19144=ORIENTED_EDGE('',*,*,#13982,.F.);
#19145=ORIENTED_EDGE('',*,*,#13981,.T.);
#19146=ORIENTED_EDGE('',*,*,#13983,.T.);
#19147=ORIENTED_EDGE('',*,*,#13984,.F.);
#19148=ORIENTED_EDGE('',*,*,#13983,.F.);
#19149=ORIENTED_EDGE('',*,*,#13985,.F.);
#19150=ORIENTED_EDGE('',*,*,#13986,.T.);
#19151=ORIENTED_EDGE('',*,*,#13987,.T.);
#19152=ORIENTED_EDGE('',*,*,#13988,.F.);
#19153=ORIENTED_EDGE('',*,*,#13989,.F.);
#19154=ORIENTED_EDGE('',*,*,#13990,.T.);
#19155=ORIENTED_EDGE('',*,*,#13991,.T.);
#19156=ORIENTED_EDGE('',*,*,#13986,.F.);
#19157=ORIENTED_EDGE('',*,*,#13992,.F.);
#19158=ORIENTED_EDGE('',*,*,#13993,.T.);
#19159=ORIENTED_EDGE('',*,*,#13994,.T.);
#19160=ORIENTED_EDGE('',*,*,#13990,.F.);
#19161=ORIENTED_EDGE('',*,*,#13995,.F.);
#19162=ORIENTED_EDGE('',*,*,#13996,.T.);
#19163=ORIENTED_EDGE('',*,*,#13997,.T.);
#19164=ORIENTED_EDGE('',*,*,#13993,.F.);
#19165=ORIENTED_EDGE('',*,*,#13998,.F.);
#19166=ORIENTED_EDGE('',*,*,#13999,.T.);
#19167=ORIENTED_EDGE('',*,*,#14000,.T.);
#19168=ORIENTED_EDGE('',*,*,#13996,.F.);
#19169=ORIENTED_EDGE('',*,*,#14001,.F.);
#19170=ORIENTED_EDGE('',*,*,#13988,.T.);
#19171=ORIENTED_EDGE('',*,*,#14002,.T.);
#19172=ORIENTED_EDGE('',*,*,#13999,.F.);
#19173=ORIENTED_EDGE('',*,*,#14002,.F.);
#19174=ORIENTED_EDGE('',*,*,#13987,.F.);
#19175=ORIENTED_EDGE('',*,*,#13991,.F.);
#19176=ORIENTED_EDGE('',*,*,#13994,.F.);
#19177=ORIENTED_EDGE('',*,*,#13997,.F.);
#19178=ORIENTED_EDGE('',*,*,#14000,.F.);
#19179=ORIENTED_EDGE('',*,*,#13984,.T.);
#19180=ORIENTED_EDGE('',*,*,#14003,.F.);
#19181=ORIENTED_EDGE('',*,*,#13948,.F.);
#19182=ORIENTED_EDGE('',*,*,#14004,.T.);
#19183=ORIENTED_EDGE('',*,*,#14003,.T.);
#19184=ORIENTED_EDGE('',*,*,#14004,.F.);
#19185=ORIENTED_EDGE('',*,*,#14005,.F.);
#19186=ORIENTED_EDGE('',*,*,#14006,.T.);
#19187=ORIENTED_EDGE('',*,*,#13972,.T.);
#19188=ORIENTED_EDGE('',*,*,#13982,.T.);
#19189=ORIENTED_EDGE('',*,*,#13973,.T.);
#19190=ORIENTED_EDGE('',*,*,#14006,.F.);
#19191=ORIENTED_EDGE('',*,*,#14005,.T.);
#19192=ORIENTED_EDGE('',*,*,#13985,.T.);
#19193=ORIENTED_EDGE('',*,*,#14001,.T.);
#19194=ORIENTED_EDGE('',*,*,#13998,.T.);
#19195=ORIENTED_EDGE('',*,*,#13995,.T.);
#19196=ORIENTED_EDGE('',*,*,#13992,.T.);
#19197=ORIENTED_EDGE('',*,*,#13989,.T.);
#19198=ORIENTED_EDGE('',*,*,#14007,.F.);
#19199=ORIENTED_EDGE('',*,*,#14008,.T.);
#19200=ORIENTED_EDGE('',*,*,#14009,.T.);
#19201=ORIENTED_EDGE('',*,*,#14010,.T.);
#19202=ORIENTED_EDGE('',*,*,#14011,.T.);
#19203=ORIENTED_EDGE('',*,*,#14010,.F.);
#19204=ORIENTED_EDGE('',*,*,#14012,.T.);
#19205=ORIENTED_EDGE('',*,*,#14013,.T.);
#19206=ORIENTED_EDGE('',*,*,#14014,.F.);
#19207=ORIENTED_EDGE('',*,*,#14015,.T.);
#19208=ORIENTED_EDGE('',*,*,#14007,.T.);
#19209=ORIENTED_EDGE('',*,*,#14016,.T.);
#19210=ORIENTED_EDGE('',*,*,#14017,.F.);
#19211=ORIENTED_EDGE('',*,*,#14018,.T.);
#19212=ORIENTED_EDGE('',*,*,#14014,.T.);
#19213=ORIENTED_EDGE('',*,*,#14019,.T.);
#19214=ORIENTED_EDGE('',*,*,#14020,.F.);
#19215=ORIENTED_EDGE('',*,*,#14021,.T.);
#19216=ORIENTED_EDGE('',*,*,#14017,.T.);
#19217=ORIENTED_EDGE('',*,*,#14022,.T.);
#19218=ORIENTED_EDGE('',*,*,#14023,.F.);
#19219=ORIENTED_EDGE('',*,*,#14024,.T.);
#19220=ORIENTED_EDGE('',*,*,#14020,.T.);
#19221=ORIENTED_EDGE('',*,*,#14025,.T.);
#19222=ORIENTED_EDGE('',*,*,#14026,.F.);
#19223=ORIENTED_EDGE('',*,*,#14027,.T.);
#19224=ORIENTED_EDGE('',*,*,#14023,.T.);
#19225=ORIENTED_EDGE('',*,*,#14028,.T.);
#19226=ORIENTED_EDGE('',*,*,#14029,.F.);
#19227=ORIENTED_EDGE('',*,*,#14030,.T.);
#19228=ORIENTED_EDGE('',*,*,#14026,.T.);
#19229=ORIENTED_EDGE('',*,*,#14031,.T.);
#19230=ORIENTED_EDGE('',*,*,#14032,.F.);
#19231=ORIENTED_EDGE('',*,*,#14033,.T.);
#19232=ORIENTED_EDGE('',*,*,#14029,.T.);
#19233=ORIENTED_EDGE('',*,*,#14034,.T.);
#19234=ORIENTED_EDGE('',*,*,#14035,.F.);
#19235=ORIENTED_EDGE('',*,*,#14036,.T.);
#19236=ORIENTED_EDGE('',*,*,#14037,.F.);
#19237=ORIENTED_EDGE('',*,*,#14038,.F.);
#19238=ORIENTED_EDGE('',*,*,#14039,.F.);
#19239=ORIENTED_EDGE('',*,*,#14040,.T.);
#19240=ORIENTED_EDGE('',*,*,#14035,.T.);
#19241=ORIENTED_EDGE('',*,*,#14041,.F.);
#19242=ORIENTED_EDGE('',*,*,#14042,.F.);
#19243=ORIENTED_EDGE('',*,*,#14043,.T.);
#19244=ORIENTED_EDGE('',*,*,#14039,.T.);
#19245=ORIENTED_EDGE('',*,*,#14044,.F.);
#19246=ORIENTED_EDGE('',*,*,#14045,.F.);
#19247=ORIENTED_EDGE('',*,*,#14046,.T.);
#19248=ORIENTED_EDGE('',*,*,#14042,.T.);
#19249=ORIENTED_EDGE('',*,*,#14047,.F.);
#19250=ORIENTED_EDGE('',*,*,#14048,.F.);
#19251=ORIENTED_EDGE('',*,*,#14049,.T.);
#19252=ORIENTED_EDGE('',*,*,#14045,.T.);
#19253=ORIENTED_EDGE('',*,*,#14050,.F.);
#19254=ORIENTED_EDGE('',*,*,#14051,.F.);
#19255=ORIENTED_EDGE('',*,*,#14052,.T.);
#19256=ORIENTED_EDGE('',*,*,#14048,.T.);
#19257=ORIENTED_EDGE('',*,*,#14053,.F.);
#19258=ORIENTED_EDGE('',*,*,#14054,.F.);
#19259=ORIENTED_EDGE('',*,*,#14055,.T.);
#19260=ORIENTED_EDGE('',*,*,#14051,.T.);
#19261=ORIENTED_EDGE('',*,*,#14056,.F.);
#19262=ORIENTED_EDGE('',*,*,#14057,.F.);
#19263=ORIENTED_EDGE('',*,*,#14058,.T.);
#19264=ORIENTED_EDGE('',*,*,#14054,.T.);
#19265=ORIENTED_EDGE('',*,*,#14059,.F.);
#19266=ORIENTED_EDGE('',*,*,#14060,.F.);
#19267=ORIENTED_EDGE('',*,*,#14061,.F.);
#19268=ORIENTED_EDGE('',*,*,#14034,.F.);
#19269=ORIENTED_EDGE('',*,*,#14031,.F.);
#19270=ORIENTED_EDGE('',*,*,#14028,.F.);
#19271=ORIENTED_EDGE('',*,*,#14025,.F.);
#19272=ORIENTED_EDGE('',*,*,#14022,.F.);
#19273=ORIENTED_EDGE('',*,*,#14019,.F.);
#19274=ORIENTED_EDGE('',*,*,#14016,.F.);
#19275=ORIENTED_EDGE('',*,*,#14013,.F.);
#19276=ORIENTED_EDGE('',*,*,#14062,.F.);
#19277=ORIENTED_EDGE('',*,*,#14063,.T.);
#19278=ORIENTED_EDGE('',*,*,#14059,.T.);
#19279=ORIENTED_EDGE('',*,*,#14056,.T.);
#19280=ORIENTED_EDGE('',*,*,#14053,.T.);
#19281=ORIENTED_EDGE('',*,*,#14050,.T.);
#19282=ORIENTED_EDGE('',*,*,#14047,.T.);
#19283=ORIENTED_EDGE('',*,*,#14044,.T.);
#19284=ORIENTED_EDGE('',*,*,#14041,.T.);
#19285=ORIENTED_EDGE('',*,*,#14038,.T.);
#19286=ORIENTED_EDGE('',*,*,#14009,.F.);
#19287=ORIENTED_EDGE('',*,*,#14064,.T.);
#19288=ORIENTED_EDGE('',*,*,#14065,.T.);
#19289=ORIENTED_EDGE('',*,*,#14062,.T.);
#19290=ORIENTED_EDGE('',*,*,#14012,.F.);
#19291=ORIENTED_EDGE('',*,*,#14057,.T.);
#19292=ORIENTED_EDGE('',*,*,#14063,.F.);
#19293=ORIENTED_EDGE('',*,*,#14065,.F.);
#19294=ORIENTED_EDGE('',*,*,#14066,.T.);
#19295=ORIENTED_EDGE('',*,*,#14067,.F.);
#19296=ORIENTED_EDGE('',*,*,#14036,.F.);
#19297=ORIENTED_EDGE('',*,*,#14040,.F.);
#19298=ORIENTED_EDGE('',*,*,#14043,.F.);
#19299=ORIENTED_EDGE('',*,*,#14046,.F.);
#19300=ORIENTED_EDGE('',*,*,#14049,.F.);
#19301=ORIENTED_EDGE('',*,*,#14052,.F.);
#19302=ORIENTED_EDGE('',*,*,#14055,.F.);
#19303=ORIENTED_EDGE('',*,*,#14058,.F.);
#19304=ORIENTED_EDGE('',*,*,#14066,.F.);
#19305=ORIENTED_EDGE('',*,*,#14064,.F.);
#19306=ORIENTED_EDGE('',*,*,#14008,.F.);
#19307=ORIENTED_EDGE('',*,*,#14015,.F.);
#19308=ORIENTED_EDGE('',*,*,#14018,.F.);
#19309=ORIENTED_EDGE('',*,*,#14021,.F.);
#19310=ORIENTED_EDGE('',*,*,#14024,.F.);
#19311=ORIENTED_EDGE('',*,*,#14027,.F.);
#19312=ORIENTED_EDGE('',*,*,#14030,.F.);
#19313=ORIENTED_EDGE('',*,*,#14033,.F.);
#19314=ORIENTED_EDGE('',*,*,#14068,.F.);
#19315=ORIENTED_EDGE('',*,*,#14032,.T.);
#19316=ORIENTED_EDGE('',*,*,#14061,.T.);
#19317=ORIENTED_EDGE('',*,*,#14069,.F.);
#19318=ORIENTED_EDGE('',*,*,#14068,.T.);
#19319=ORIENTED_EDGE('',*,*,#14070,.T.);
#19320=ORIENTED_EDGE('',*,*,#14071,.T.);
#19321=ORIENTED_EDGE('',*,*,#14070,.F.);
#19322=ORIENTED_EDGE('',*,*,#14071,.F.);
#19323=ORIENTED_EDGE('',*,*,#14072,.T.);
#19324=ORIENTED_EDGE('',*,*,#14073,.T.);
#19325=ORIENTED_EDGE('',*,*,#14072,.F.);
#19326=ORIENTED_EDGE('',*,*,#14073,.F.);
#19327=ORIENTED_EDGE('',*,*,#14074,.T.);
#19328=ORIENTED_EDGE('',*,*,#14075,.F.);
#19329=ORIENTED_EDGE('',*,*,#14074,.F.);
#19330=ORIENTED_EDGE('',*,*,#14076,.F.);
#19331=ORIENTED_EDGE('',*,*,#14077,.F.);
#19332=ORIENTED_EDGE('',*,*,#14078,.F.);
#19333=ORIENTED_EDGE('',*,*,#14079,.F.);
#19334=ORIENTED_EDGE('',*,*,#14080,.F.);
#19335=ORIENTED_EDGE('',*,*,#14081,.F.);
#19336=ORIENTED_EDGE('',*,*,#14082,.F.);
#19337=ORIENTED_EDGE('',*,*,#14083,.F.);
#19338=ORIENTED_EDGE('',*,*,#14084,.F.);
#19339=ORIENTED_EDGE('',*,*,#14085,.F.);
#19340=ORIENTED_EDGE('',*,*,#14086,.F.);
#19341=ORIENTED_EDGE('',*,*,#14087,.F.);
#19342=ORIENTED_EDGE('',*,*,#14088,.F.);
#19343=ORIENTED_EDGE('',*,*,#14089,.F.);
#19344=ORIENTED_EDGE('',*,*,#14090,.F.);
#19345=ORIENTED_EDGE('',*,*,#14091,.F.);
#19346=ORIENTED_EDGE('',*,*,#14092,.F.);
#19347=ORIENTED_EDGE('',*,*,#14093,.F.);
#19348=ORIENTED_EDGE('',*,*,#14089,.T.);
#19349=ORIENTED_EDGE('',*,*,#14094,.T.);
#19350=ORIENTED_EDGE('',*,*,#14095,.T.);
#19351=ORIENTED_EDGE('',*,*,#14096,.F.);
#19352=ORIENTED_EDGE('',*,*,#14097,.T.);
#19353=ORIENTED_EDGE('',*,*,#14098,.F.);
#19354=ORIENTED_EDGE('',*,*,#14085,.T.);
#19355=ORIENTED_EDGE('',*,*,#14099,.T.);
#19356=ORIENTED_EDGE('',*,*,#14086,.T.);
#19357=ORIENTED_EDGE('',*,*,#14098,.T.);
#19358=ORIENTED_EDGE('',*,*,#14100,.T.);
#19359=ORIENTED_EDGE('',*,*,#14101,.F.);
#19360=ORIENTED_EDGE('',*,*,#14102,.T.);
#19361=ORIENTED_EDGE('',*,*,#14103,.F.);
#19362=ORIENTED_EDGE('',*,*,#14082,.T.);
#19363=ORIENTED_EDGE('',*,*,#14104,.T.);
#19364=ORIENTED_EDGE('',*,*,#14083,.T.);
#19365=ORIENTED_EDGE('',*,*,#14103,.T.);
#19366=ORIENTED_EDGE('',*,*,#14105,.T.);
#19367=ORIENTED_EDGE('',*,*,#14106,.F.);
#19368=ORIENTED_EDGE('',*,*,#14107,.T.);
#19369=ORIENTED_EDGE('',*,*,#14108,.F.);
#19370=ORIENTED_EDGE('',*,*,#14079,.T.);
#19371=ORIENTED_EDGE('',*,*,#14109,.T.);
#19372=ORIENTED_EDGE('',*,*,#14092,.T.);
#19373=ORIENTED_EDGE('',*,*,#14110,.F.);
#19374=ORIENTED_EDGE('',*,*,#14090,.T.);
#19375=ORIENTED_EDGE('',*,*,#14099,.F.);
#19376=ORIENTED_EDGE('',*,*,#14087,.T.);
#19377=ORIENTED_EDGE('',*,*,#14104,.F.);
#19378=ORIENTED_EDGE('',*,*,#14084,.T.);
#19379=ORIENTED_EDGE('',*,*,#14109,.F.);
#19380=ORIENTED_EDGE('',*,*,#14081,.T.);
#19381=ORIENTED_EDGE('',*,*,#14111,.F.);
#19382=ORIENTED_EDGE('',*,*,#14078,.T.);
#19383=ORIENTED_EDGE('',*,*,#14112,.F.);
#19384=ORIENTED_EDGE('',*,*,#14069,.T.);
#19385=ORIENTED_EDGE('',*,*,#14060,.T.);
#19386=ORIENTED_EDGE('',*,*,#14037,.T.);
#19387=ORIENTED_EDGE('',*,*,#14067,.T.);
#19388=ORIENTED_EDGE('',*,*,#14080,.T.);
#19389=ORIENTED_EDGE('',*,*,#14108,.T.);
#19390=ORIENTED_EDGE('',*,*,#14113,.T.);
#19391=ORIENTED_EDGE('',*,*,#14114,.F.);
#19392=ORIENTED_EDGE('',*,*,#14115,.T.);
#19393=ORIENTED_EDGE('',*,*,#14116,.F.);
#19394=ORIENTED_EDGE('',*,*,#14076,.T.);
#19395=ORIENTED_EDGE('',*,*,#14111,.T.);
#19396=ORIENTED_EDGE('',*,*,#14117,.F.);
#19397=ORIENTED_EDGE('',*,*,#14118,.F.);
#19398=ORIENTED_EDGE('',*,*,#14119,.F.);
#19399=ORIENTED_EDGE('',*,*,#14115,.F.);
#19400=ORIENTED_EDGE('',*,*,#14120,.F.);
#19401=ORIENTED_EDGE('',*,*,#14121,.F.);
#19402=ORIENTED_EDGE('',*,*,#14107,.F.);
#19403=ORIENTED_EDGE('',*,*,#14122,.F.);
#19404=ORIENTED_EDGE('',*,*,#14113,.F.);
#19405=ORIENTED_EDGE('',*,*,#14102,.F.);
#19406=ORIENTED_EDGE('',*,*,#14123,.F.);
#19407=ORIENTED_EDGE('',*,*,#14105,.F.);
#19408=ORIENTED_EDGE('',*,*,#14097,.F.);
#19409=ORIENTED_EDGE('',*,*,#14124,.F.);
#19410=ORIENTED_EDGE('',*,*,#14100,.F.);
#19411=ORIENTED_EDGE('',*,*,#14095,.F.);
#19412=ORIENTED_EDGE('',*,*,#14125,.F.);
#19413=ORIENTED_EDGE('',*,*,#14126,.F.);
#19414=ORIENTED_EDGE('',*,*,#14091,.T.);
#19415=ORIENTED_EDGE('',*,*,#14127,.T.);
#19416=ORIENTED_EDGE('',*,*,#14119,.T.);
#19417=ORIENTED_EDGE('',*,*,#14128,.F.);
#19418=ORIENTED_EDGE('',*,*,#14125,.T.);
#19419=ORIENTED_EDGE('',*,*,#14094,.F.);
#19420=ORIENTED_EDGE('',*,*,#14088,.T.);
#19421=ORIENTED_EDGE('',*,*,#14110,.T.);
#19422=ORIENTED_EDGE('',*,*,#14129,.F.);
#19423=ORIENTED_EDGE('',*,*,#14011,.F.);
#19424=ORIENTED_EDGE('',*,*,#14130,.T.);
#19425=ORIENTED_EDGE('',*,*,#14129,.T.);
#19426=ORIENTED_EDGE('',*,*,#14130,.F.);
#19427=ORIENTED_EDGE('',*,*,#14093,.T.);
#19428=ORIENTED_EDGE('',*,*,#14112,.T.);
#19429=ORIENTED_EDGE('',*,*,#14077,.T.);
#19430=ORIENTED_EDGE('',*,*,#14116,.T.);
#19431=ORIENTED_EDGE('',*,*,#14121,.T.);
#19432=ORIENTED_EDGE('',*,*,#14131,.F.);
#19433=ORIENTED_EDGE('',*,*,#14117,.T.);
#19434=ORIENTED_EDGE('',*,*,#14127,.F.);
#19435=ORIENTED_EDGE('',*,*,#14126,.T.);
#19436=ORIENTED_EDGE('',*,*,#14128,.T.);
#19437=ORIENTED_EDGE('',*,*,#14118,.T.);
#19438=ORIENTED_EDGE('',*,*,#14131,.T.);
#19439=ORIENTED_EDGE('',*,*,#14120,.T.);
#19440=ORIENTED_EDGE('',*,*,#14114,.T.);
#19441=ORIENTED_EDGE('',*,*,#14122,.T.);
#19442=ORIENTED_EDGE('',*,*,#14106,.T.);
#19443=ORIENTED_EDGE('',*,*,#14123,.T.);
#19444=ORIENTED_EDGE('',*,*,#14101,.T.);
#19445=ORIENTED_EDGE('',*,*,#14124,.T.);
#19446=ORIENTED_EDGE('',*,*,#14096,.T.);
#19447=ORIENTED_EDGE('',*,*,#14075,.T.);
#19448=ORIENTED_EDGE('',*,*,#14132,.F.);
#19449=ORIENTED_EDGE('',*,*,#14133,.T.);
#19450=ORIENTED_EDGE('',*,*,#14134,.T.);
#19451=ORIENTED_EDGE('',*,*,#14135,.T.);
#19452=ORIENTED_EDGE('',*,*,#14136,.T.);
#19453=ORIENTED_EDGE('',*,*,#14135,.F.);
#19454=ORIENTED_EDGE('',*,*,#14137,.T.);
#19455=ORIENTED_EDGE('',*,*,#14138,.T.);
#19456=ORIENTED_EDGE('',*,*,#14139,.F.);
#19457=ORIENTED_EDGE('',*,*,#14140,.T.);
#19458=ORIENTED_EDGE('',*,*,#14132,.T.);
#19459=ORIENTED_EDGE('',*,*,#14141,.T.);
#19460=ORIENTED_EDGE('',*,*,#14142,.F.);
#19461=ORIENTED_EDGE('',*,*,#14143,.T.);
#19462=ORIENTED_EDGE('',*,*,#14139,.T.);
#19463=ORIENTED_EDGE('',*,*,#14144,.T.);
#19464=ORIENTED_EDGE('',*,*,#14145,.F.);
#19465=ORIENTED_EDGE('',*,*,#14146,.T.);
#19466=ORIENTED_EDGE('',*,*,#14142,.T.);
#19467=ORIENTED_EDGE('',*,*,#14147,.T.);
#19468=ORIENTED_EDGE('',*,*,#14148,.F.);
#19469=ORIENTED_EDGE('',*,*,#14149,.T.);
#19470=ORIENTED_EDGE('',*,*,#14145,.T.);
#19471=ORIENTED_EDGE('',*,*,#14150,.T.);
#19472=ORIENTED_EDGE('',*,*,#14151,.F.);
#19473=ORIENTED_EDGE('',*,*,#14152,.T.);
#19474=ORIENTED_EDGE('',*,*,#14148,.T.);
#19475=ORIENTED_EDGE('',*,*,#14153,.T.);
#19476=ORIENTED_EDGE('',*,*,#14154,.F.);
#19477=ORIENTED_EDGE('',*,*,#14155,.T.);
#19478=ORIENTED_EDGE('',*,*,#14151,.T.);
#19479=ORIENTED_EDGE('',*,*,#14156,.T.);
#19480=ORIENTED_EDGE('',*,*,#14157,.F.);
#19481=ORIENTED_EDGE('',*,*,#14158,.T.);
#19482=ORIENTED_EDGE('',*,*,#14154,.T.);
#19483=ORIENTED_EDGE('',*,*,#14159,.T.);
#19484=ORIENTED_EDGE('',*,*,#14160,.F.);
#19485=ORIENTED_EDGE('',*,*,#14161,.T.);
#19486=ORIENTED_EDGE('',*,*,#14157,.T.);
#19487=ORIENTED_EDGE('',*,*,#14162,.T.);
#19488=ORIENTED_EDGE('',*,*,#14163,.F.);
#19489=ORIENTED_EDGE('',*,*,#14164,.T.);
#19490=ORIENTED_EDGE('',*,*,#14160,.T.);
#19491=ORIENTED_EDGE('',*,*,#14165,.T.);
#19492=ORIENTED_EDGE('',*,*,#14166,.F.);
#19493=ORIENTED_EDGE('',*,*,#14167,.T.);
#19494=ORIENTED_EDGE('',*,*,#14163,.T.);
#19495=ORIENTED_EDGE('',*,*,#14168,.T.);
#19496=ORIENTED_EDGE('',*,*,#14169,.F.);
#19497=ORIENTED_EDGE('',*,*,#14170,.T.);
#19498=ORIENTED_EDGE('',*,*,#14166,.T.);
#19499=ORIENTED_EDGE('',*,*,#14171,.T.);
#19500=ORIENTED_EDGE('',*,*,#14172,.F.);
#19501=ORIENTED_EDGE('',*,*,#14173,.T.);
#19502=ORIENTED_EDGE('',*,*,#14169,.T.);
#19503=ORIENTED_EDGE('',*,*,#14174,.T.);
#19504=ORIENTED_EDGE('',*,*,#14175,.F.);
#19505=ORIENTED_EDGE('',*,*,#14176,.T.);
#19506=ORIENTED_EDGE('',*,*,#14172,.T.);
#19507=ORIENTED_EDGE('',*,*,#14177,.T.);
#19508=ORIENTED_EDGE('',*,*,#14178,.F.);
#19509=ORIENTED_EDGE('',*,*,#14179,.T.);
#19510=ORIENTED_EDGE('',*,*,#14175,.T.);
#19511=ORIENTED_EDGE('',*,*,#14180,.T.);
#19512=ORIENTED_EDGE('',*,*,#14181,.F.);
#19513=ORIENTED_EDGE('',*,*,#14182,.T.);
#19514=ORIENTED_EDGE('',*,*,#14178,.T.);
#19515=ORIENTED_EDGE('',*,*,#14183,.T.);
#19516=ORIENTED_EDGE('',*,*,#14184,.F.);
#19517=ORIENTED_EDGE('',*,*,#14185,.T.);
#19518=ORIENTED_EDGE('',*,*,#14181,.T.);
#19519=ORIENTED_EDGE('',*,*,#14186,.T.);
#19520=ORIENTED_EDGE('',*,*,#14187,.F.);
#19521=ORIENTED_EDGE('',*,*,#14188,.T.);
#19522=ORIENTED_EDGE('',*,*,#14184,.T.);
#19523=ORIENTED_EDGE('',*,*,#14189,.T.);
#19524=ORIENTED_EDGE('',*,*,#14190,.F.);
#19525=ORIENTED_EDGE('',*,*,#14191,.T.);
#19526=ORIENTED_EDGE('',*,*,#14187,.T.);
#19527=ORIENTED_EDGE('',*,*,#14192,.T.);
#19528=ORIENTED_EDGE('',*,*,#14193,.F.);
#19529=ORIENTED_EDGE('',*,*,#14194,.T.);
#19530=ORIENTED_EDGE('',*,*,#14190,.T.);
#19531=ORIENTED_EDGE('',*,*,#14195,.T.);
#19532=ORIENTED_EDGE('',*,*,#14196,.F.);
#19533=ORIENTED_EDGE('',*,*,#14197,.T.);
#19534=ORIENTED_EDGE('',*,*,#14193,.T.);
#19535=ORIENTED_EDGE('',*,*,#14198,.T.);
#19536=ORIENTED_EDGE('',*,*,#14199,.F.);
#19537=ORIENTED_EDGE('',*,*,#14200,.T.);
#19538=ORIENTED_EDGE('',*,*,#14196,.T.);
#19539=ORIENTED_EDGE('',*,*,#14201,.T.);
#19540=ORIENTED_EDGE('',*,*,#14202,.F.);
#19541=ORIENTED_EDGE('',*,*,#14203,.T.);
#19542=ORIENTED_EDGE('',*,*,#14199,.T.);
#19543=ORIENTED_EDGE('',*,*,#14204,.T.);
#19544=ORIENTED_EDGE('',*,*,#14205,.F.);
#19545=ORIENTED_EDGE('',*,*,#14206,.T.);
#19546=ORIENTED_EDGE('',*,*,#14202,.T.);
#19547=ORIENTED_EDGE('',*,*,#14207,.T.);
#19548=ORIENTED_EDGE('',*,*,#14208,.F.);
#19549=ORIENTED_EDGE('',*,*,#14209,.T.);
#19550=ORIENTED_EDGE('',*,*,#14205,.T.);
#19551=ORIENTED_EDGE('',*,*,#14210,.T.);
#19552=ORIENTED_EDGE('',*,*,#14211,.F.);
#19553=ORIENTED_EDGE('',*,*,#14212,.T.);
#19554=ORIENTED_EDGE('',*,*,#14208,.T.);
#19555=ORIENTED_EDGE('',*,*,#14213,.T.);
#19556=ORIENTED_EDGE('',*,*,#14214,.F.);
#19557=ORIENTED_EDGE('',*,*,#14215,.T.);
#19558=ORIENTED_EDGE('',*,*,#14211,.T.);
#19559=ORIENTED_EDGE('',*,*,#14216,.T.);
#19560=ORIENTED_EDGE('',*,*,#14217,.F.);
#19561=ORIENTED_EDGE('',*,*,#14218,.T.);
#19562=ORIENTED_EDGE('',*,*,#14214,.T.);
#19563=ORIENTED_EDGE('',*,*,#14219,.T.);
#19564=ORIENTED_EDGE('',*,*,#14220,.F.);
#19565=ORIENTED_EDGE('',*,*,#14221,.T.);
#19566=ORIENTED_EDGE('',*,*,#14222,.F.);
#19567=ORIENTED_EDGE('',*,*,#14223,.F.);
#19568=ORIENTED_EDGE('',*,*,#14224,.F.);
#19569=ORIENTED_EDGE('',*,*,#14225,.T.);
#19570=ORIENTED_EDGE('',*,*,#14220,.T.);
#19571=ORIENTED_EDGE('',*,*,#14226,.F.);
#19572=ORIENTED_EDGE('',*,*,#14227,.F.);
#19573=ORIENTED_EDGE('',*,*,#14228,.T.);
#19574=ORIENTED_EDGE('',*,*,#14224,.T.);
#19575=ORIENTED_EDGE('',*,*,#14229,.F.);
#19576=ORIENTED_EDGE('',*,*,#14230,.F.);
#19577=ORIENTED_EDGE('',*,*,#14231,.T.);
#19578=ORIENTED_EDGE('',*,*,#14227,.T.);
#19579=ORIENTED_EDGE('',*,*,#14232,.F.);
#19580=ORIENTED_EDGE('',*,*,#14233,.F.);
#19581=ORIENTED_EDGE('',*,*,#14234,.T.);
#19582=ORIENTED_EDGE('',*,*,#14230,.T.);
#19583=ORIENTED_EDGE('',*,*,#14235,.F.);
#19584=ORIENTED_EDGE('',*,*,#14236,.F.);
#19585=ORIENTED_EDGE('',*,*,#14237,.T.);
#19586=ORIENTED_EDGE('',*,*,#14233,.T.);
#19587=ORIENTED_EDGE('',*,*,#14238,.F.);
#19588=ORIENTED_EDGE('',*,*,#14239,.F.);
#19589=ORIENTED_EDGE('',*,*,#14240,.T.);
#19590=ORIENTED_EDGE('',*,*,#14236,.T.);
#19591=ORIENTED_EDGE('',*,*,#14241,.F.);
#19592=ORIENTED_EDGE('',*,*,#14242,.F.);
#19593=ORIENTED_EDGE('',*,*,#14243,.T.);
#19594=ORIENTED_EDGE('',*,*,#14239,.T.);
#19595=ORIENTED_EDGE('',*,*,#14244,.F.);
#19596=ORIENTED_EDGE('',*,*,#14245,.F.);
#19597=ORIENTED_EDGE('',*,*,#14246,.T.);
#19598=ORIENTED_EDGE('',*,*,#14242,.T.);
#19599=ORIENTED_EDGE('',*,*,#14247,.F.);
#19600=ORIENTED_EDGE('',*,*,#14248,.F.);
#19601=ORIENTED_EDGE('',*,*,#14249,.T.);
#19602=ORIENTED_EDGE('',*,*,#14245,.T.);
#19603=ORIENTED_EDGE('',*,*,#14250,.F.);
#19604=ORIENTED_EDGE('',*,*,#14251,.F.);
#19605=ORIENTED_EDGE('',*,*,#14252,.T.);
#19606=ORIENTED_EDGE('',*,*,#14248,.T.);
#19607=ORIENTED_EDGE('',*,*,#14253,.F.);
#19608=ORIENTED_EDGE('',*,*,#14254,.F.);
#19609=ORIENTED_EDGE('',*,*,#14255,.T.);
#19610=ORIENTED_EDGE('',*,*,#14251,.T.);
#19611=ORIENTED_EDGE('',*,*,#14256,.F.);
#19612=ORIENTED_EDGE('',*,*,#14257,.F.);
#19613=ORIENTED_EDGE('',*,*,#14258,.T.);
#19614=ORIENTED_EDGE('',*,*,#14254,.T.);
#19615=ORIENTED_EDGE('',*,*,#14259,.F.);
#19616=ORIENTED_EDGE('',*,*,#14260,.F.);
#19617=ORIENTED_EDGE('',*,*,#14261,.T.);
#19618=ORIENTED_EDGE('',*,*,#14257,.T.);
#19619=ORIENTED_EDGE('',*,*,#14262,.F.);
#19620=ORIENTED_EDGE('',*,*,#14263,.F.);
#19621=ORIENTED_EDGE('',*,*,#14264,.T.);
#19622=ORIENTED_EDGE('',*,*,#14260,.T.);
#19623=ORIENTED_EDGE('',*,*,#14265,.F.);
#19624=ORIENTED_EDGE('',*,*,#14266,.F.);
#19625=ORIENTED_EDGE('',*,*,#14267,.T.);
#19626=ORIENTED_EDGE('',*,*,#14263,.T.);
#19627=ORIENTED_EDGE('',*,*,#14268,.F.);
#19628=ORIENTED_EDGE('',*,*,#14269,.F.);
#19629=ORIENTED_EDGE('',*,*,#14270,.T.);
#19630=ORIENTED_EDGE('',*,*,#14266,.T.);
#19631=ORIENTED_EDGE('',*,*,#14271,.F.);
#19632=ORIENTED_EDGE('',*,*,#14272,.F.);
#19633=ORIENTED_EDGE('',*,*,#14273,.T.);
#19634=ORIENTED_EDGE('',*,*,#14269,.T.);
#19635=ORIENTED_EDGE('',*,*,#14274,.F.);
#19636=ORIENTED_EDGE('',*,*,#14275,.F.);
#19637=ORIENTED_EDGE('',*,*,#14276,.T.);
#19638=ORIENTED_EDGE('',*,*,#14272,.T.);
#19639=ORIENTED_EDGE('',*,*,#14277,.F.);
#19640=ORIENTED_EDGE('',*,*,#14278,.F.);
#19641=ORIENTED_EDGE('',*,*,#14279,.T.);
#19642=ORIENTED_EDGE('',*,*,#14275,.T.);
#19643=ORIENTED_EDGE('',*,*,#14280,.F.);
#19644=ORIENTED_EDGE('',*,*,#14281,.F.);
#19645=ORIENTED_EDGE('',*,*,#14282,.T.);
#19646=ORIENTED_EDGE('',*,*,#14278,.T.);
#19647=ORIENTED_EDGE('',*,*,#14283,.F.);
#19648=ORIENTED_EDGE('',*,*,#14284,.F.);
#19649=ORIENTED_EDGE('',*,*,#14285,.T.);
#19650=ORIENTED_EDGE('',*,*,#14281,.T.);
#19651=ORIENTED_EDGE('',*,*,#14286,.F.);
#19652=ORIENTED_EDGE('',*,*,#14287,.F.);
#19653=ORIENTED_EDGE('',*,*,#14288,.T.);
#19654=ORIENTED_EDGE('',*,*,#14284,.T.);
#19655=ORIENTED_EDGE('',*,*,#14289,.F.);
#19656=ORIENTED_EDGE('',*,*,#14290,.F.);
#19657=ORIENTED_EDGE('',*,*,#14291,.T.);
#19658=ORIENTED_EDGE('',*,*,#14287,.T.);
#19659=ORIENTED_EDGE('',*,*,#14292,.F.);
#19660=ORIENTED_EDGE('',*,*,#14293,.F.);
#19661=ORIENTED_EDGE('',*,*,#14294,.T.);
#19662=ORIENTED_EDGE('',*,*,#14290,.T.);
#19663=ORIENTED_EDGE('',*,*,#14295,.F.);
#19664=ORIENTED_EDGE('',*,*,#14296,.F.);
#19665=ORIENTED_EDGE('',*,*,#14297,.T.);
#19666=ORIENTED_EDGE('',*,*,#14293,.T.);
#19667=ORIENTED_EDGE('',*,*,#14298,.F.);
#19668=ORIENTED_EDGE('',*,*,#14299,.F.);
#19669=ORIENTED_EDGE('',*,*,#14300,.T.);
#19670=ORIENTED_EDGE('',*,*,#14296,.T.);
#19671=ORIENTED_EDGE('',*,*,#14301,.F.);
#19672=ORIENTED_EDGE('',*,*,#14302,.F.);
#19673=ORIENTED_EDGE('',*,*,#14303,.T.);
#19674=ORIENTED_EDGE('',*,*,#14299,.T.);
#19675=ORIENTED_EDGE('',*,*,#14304,.F.);
#19676=ORIENTED_EDGE('',*,*,#14305,.F.);
#19677=ORIENTED_EDGE('',*,*,#14306,.F.);
#19678=ORIENTED_EDGE('',*,*,#14307,.T.);
#19679=ORIENTED_EDGE('',*,*,#14302,.T.);
#19680=ORIENTED_EDGE('',*,*,#14308,.F.);
#19681=ORIENTED_EDGE('',*,*,#14222,.T.);
#19682=ORIENTED_EDGE('',*,*,#14309,.T.);
#19683=ORIENTED_EDGE('',*,*,#14310,.F.);
#19684=ORIENTED_EDGE('',*,*,#14311,.F.);
#19685=ORIENTED_EDGE('',*,*,#14312,.T.);
#19686=ORIENTED_EDGE('',*,*,#14312,.F.);
#19687=ORIENTED_EDGE('',*,*,#14313,.F.);
#19688=ORIENTED_EDGE('',*,*,#14219,.F.);
#19689=ORIENTED_EDGE('',*,*,#14216,.F.);
#19690=ORIENTED_EDGE('',*,*,#14213,.F.);
#19691=ORIENTED_EDGE('',*,*,#14210,.F.);
#19692=ORIENTED_EDGE('',*,*,#14207,.F.);
#19693=ORIENTED_EDGE('',*,*,#14204,.F.);
#19694=ORIENTED_EDGE('',*,*,#14201,.F.);
#19695=ORIENTED_EDGE('',*,*,#14198,.F.);
#19696=ORIENTED_EDGE('',*,*,#14195,.F.);
#19697=ORIENTED_EDGE('',*,*,#14192,.F.);
#19698=ORIENTED_EDGE('',*,*,#14189,.F.);
#19699=ORIENTED_EDGE('',*,*,#14186,.F.);
#19700=ORIENTED_EDGE('',*,*,#14183,.F.);
#19701=ORIENTED_EDGE('',*,*,#14180,.F.);
#19702=ORIENTED_EDGE('',*,*,#14177,.F.);
#19703=ORIENTED_EDGE('',*,*,#14174,.F.);
#19704=ORIENTED_EDGE('',*,*,#14171,.F.);
#19705=ORIENTED_EDGE('',*,*,#14168,.F.);
#19706=ORIENTED_EDGE('',*,*,#14165,.F.);
#19707=ORIENTED_EDGE('',*,*,#14162,.F.);
#19708=ORIENTED_EDGE('',*,*,#14159,.F.);
#19709=ORIENTED_EDGE('',*,*,#14156,.F.);
#19710=ORIENTED_EDGE('',*,*,#14153,.F.);
#19711=ORIENTED_EDGE('',*,*,#14150,.F.);
#19712=ORIENTED_EDGE('',*,*,#14147,.F.);
#19713=ORIENTED_EDGE('',*,*,#14144,.F.);
#19714=ORIENTED_EDGE('',*,*,#14141,.F.);
#19715=ORIENTED_EDGE('',*,*,#14138,.F.);
#19716=ORIENTED_EDGE('',*,*,#14314,.F.);
#19717=ORIENTED_EDGE('',*,*,#14315,.T.);
#19718=ORIENTED_EDGE('',*,*,#14308,.T.);
#19719=ORIENTED_EDGE('',*,*,#14304,.T.);
#19720=ORIENTED_EDGE('',*,*,#14301,.T.);
#19721=ORIENTED_EDGE('',*,*,#14298,.T.);
#19722=ORIENTED_EDGE('',*,*,#14295,.T.);
#19723=ORIENTED_EDGE('',*,*,#14292,.T.);
#19724=ORIENTED_EDGE('',*,*,#14289,.T.);
#19725=ORIENTED_EDGE('',*,*,#14286,.T.);
#19726=ORIENTED_EDGE('',*,*,#14283,.T.);
#19727=ORIENTED_EDGE('',*,*,#14280,.T.);
#19728=ORIENTED_EDGE('',*,*,#14277,.T.);
#19729=ORIENTED_EDGE('',*,*,#14274,.T.);
#19730=ORIENTED_EDGE('',*,*,#14271,.T.);
#19731=ORIENTED_EDGE('',*,*,#14268,.T.);
#19732=ORIENTED_EDGE('',*,*,#14265,.T.);
#19733=ORIENTED_EDGE('',*,*,#14262,.T.);
#19734=ORIENTED_EDGE('',*,*,#14259,.T.);
#19735=ORIENTED_EDGE('',*,*,#14256,.T.);
#19736=ORIENTED_EDGE('',*,*,#14253,.T.);
#19737=ORIENTED_EDGE('',*,*,#14250,.T.);
#19738=ORIENTED_EDGE('',*,*,#14247,.T.);
#19739=ORIENTED_EDGE('',*,*,#14244,.T.);
#19740=ORIENTED_EDGE('',*,*,#14241,.T.);
#19741=ORIENTED_EDGE('',*,*,#14238,.T.);
#19742=ORIENTED_EDGE('',*,*,#14235,.T.);
#19743=ORIENTED_EDGE('',*,*,#14232,.T.);
#19744=ORIENTED_EDGE('',*,*,#14229,.T.);
#19745=ORIENTED_EDGE('',*,*,#14226,.T.);
#19746=ORIENTED_EDGE('',*,*,#14223,.T.);
#19747=ORIENTED_EDGE('',*,*,#14134,.F.);
#19748=ORIENTED_EDGE('',*,*,#14316,.T.);
#19749=ORIENTED_EDGE('',*,*,#14306,.T.);
#19750=ORIENTED_EDGE('',*,*,#14317,.T.);
#19751=ORIENTED_EDGE('',*,*,#14314,.T.);
#19752=ORIENTED_EDGE('',*,*,#14137,.F.);
#19753=ORIENTED_EDGE('',*,*,#14305,.T.);
#19754=ORIENTED_EDGE('',*,*,#14315,.F.);
#19755=ORIENTED_EDGE('',*,*,#14317,.F.);
#19756=ORIENTED_EDGE('',*,*,#14309,.F.);
#19757=ORIENTED_EDGE('',*,*,#14221,.F.);
#19758=ORIENTED_EDGE('',*,*,#14225,.F.);
#19759=ORIENTED_EDGE('',*,*,#14228,.F.);
#19760=ORIENTED_EDGE('',*,*,#14231,.F.);
#19761=ORIENTED_EDGE('',*,*,#14234,.F.);
#19762=ORIENTED_EDGE('',*,*,#14237,.F.);
#19763=ORIENTED_EDGE('',*,*,#14240,.F.);
#19764=ORIENTED_EDGE('',*,*,#14243,.F.);
#19765=ORIENTED_EDGE('',*,*,#14246,.F.);
#19766=ORIENTED_EDGE('',*,*,#14249,.F.);
#19767=ORIENTED_EDGE('',*,*,#14252,.F.);
#19768=ORIENTED_EDGE('',*,*,#14255,.F.);
#19769=ORIENTED_EDGE('',*,*,#14258,.F.);
#19770=ORIENTED_EDGE('',*,*,#14261,.F.);
#19771=ORIENTED_EDGE('',*,*,#14264,.F.);
#19772=ORIENTED_EDGE('',*,*,#14267,.F.);
#19773=ORIENTED_EDGE('',*,*,#14270,.F.);
#19774=ORIENTED_EDGE('',*,*,#14273,.F.);
#19775=ORIENTED_EDGE('',*,*,#14276,.F.);
#19776=ORIENTED_EDGE('',*,*,#14279,.F.);
#19777=ORIENTED_EDGE('',*,*,#14282,.F.);
#19778=ORIENTED_EDGE('',*,*,#14285,.F.);
#19779=ORIENTED_EDGE('',*,*,#14288,.F.);
#19780=ORIENTED_EDGE('',*,*,#14291,.F.);
#19781=ORIENTED_EDGE('',*,*,#14294,.F.);
#19782=ORIENTED_EDGE('',*,*,#14297,.F.);
#19783=ORIENTED_EDGE('',*,*,#14300,.F.);
#19784=ORIENTED_EDGE('',*,*,#14303,.F.);
#19785=ORIENTED_EDGE('',*,*,#14307,.F.);
#19786=ORIENTED_EDGE('',*,*,#14316,.F.);
#19787=ORIENTED_EDGE('',*,*,#14133,.F.);
#19788=ORIENTED_EDGE('',*,*,#14140,.F.);
#19789=ORIENTED_EDGE('',*,*,#14143,.F.);
#19790=ORIENTED_EDGE('',*,*,#14146,.F.);
#19791=ORIENTED_EDGE('',*,*,#14149,.F.);
#19792=ORIENTED_EDGE('',*,*,#14152,.F.);
#19793=ORIENTED_EDGE('',*,*,#14155,.F.);
#19794=ORIENTED_EDGE('',*,*,#14158,.F.);
#19795=ORIENTED_EDGE('',*,*,#14161,.F.);
#19796=ORIENTED_EDGE('',*,*,#14164,.F.);
#19797=ORIENTED_EDGE('',*,*,#14167,.F.);
#19798=ORIENTED_EDGE('',*,*,#14170,.F.);
#19799=ORIENTED_EDGE('',*,*,#14173,.F.);
#19800=ORIENTED_EDGE('',*,*,#14176,.F.);
#19801=ORIENTED_EDGE('',*,*,#14179,.F.);
#19802=ORIENTED_EDGE('',*,*,#14182,.F.);
#19803=ORIENTED_EDGE('',*,*,#14185,.F.);
#19804=ORIENTED_EDGE('',*,*,#14188,.F.);
#19805=ORIENTED_EDGE('',*,*,#14191,.F.);
#19806=ORIENTED_EDGE('',*,*,#14194,.F.);
#19807=ORIENTED_EDGE('',*,*,#14197,.F.);
#19808=ORIENTED_EDGE('',*,*,#14200,.F.);
#19809=ORIENTED_EDGE('',*,*,#14203,.F.);
#19810=ORIENTED_EDGE('',*,*,#14206,.F.);
#19811=ORIENTED_EDGE('',*,*,#14209,.F.);
#19812=ORIENTED_EDGE('',*,*,#14212,.F.);
#19813=ORIENTED_EDGE('',*,*,#14215,.F.);
#19814=ORIENTED_EDGE('',*,*,#14218,.F.);
#19815=ORIENTED_EDGE('',*,*,#14318,.F.);
#19816=ORIENTED_EDGE('',*,*,#14319,.F.);
#19817=ORIENTED_EDGE('',*,*,#14320,.T.);
#19818=ORIENTED_EDGE('',*,*,#14321,.T.);
#19819=ORIENTED_EDGE('',*,*,#14322,.F.);
#19820=ORIENTED_EDGE('',*,*,#14321,.F.);
#19821=ORIENTED_EDGE('',*,*,#14323,.T.);
#19822=ORIENTED_EDGE('',*,*,#14324,.F.);
#19823=ORIENTED_EDGE('',*,*,#14325,.F.);
#19824=ORIENTED_EDGE('',*,*,#14326,.F.);
#19825=ORIENTED_EDGE('',*,*,#14323,.F.);
#19826=ORIENTED_EDGE('',*,*,#14320,.F.);
#19827=ORIENTED_EDGE('',*,*,#14327,.F.);
#19828=ORIENTED_EDGE('',*,*,#14328,.T.);
#19829=ORIENTED_EDGE('',*,*,#14329,.T.);
#19830=ORIENTED_EDGE('',*,*,#14330,.F.);
#19831=ORIENTED_EDGE('',*,*,#14329,.F.);
#19832=ORIENTED_EDGE('',*,*,#14331,.T.);
#19833=ORIENTED_EDGE('',*,*,#14332,.F.);
#19834=ORIENTED_EDGE('',*,*,#14333,.F.);
#19835=ORIENTED_EDGE('',*,*,#14334,.F.);
#19836=ORIENTED_EDGE('',*,*,#14331,.F.);
#19837=ORIENTED_EDGE('',*,*,#14328,.F.);
#19838=ORIENTED_EDGE('',*,*,#14335,.F.);
#19839=ORIENTED_EDGE('',*,*,#14336,.T.);
#19840=ORIENTED_EDGE('',*,*,#14337,.T.);
#19841=ORIENTED_EDGE('',*,*,#14338,.F.);
#19842=ORIENTED_EDGE('',*,*,#14337,.F.);
#19843=ORIENTED_EDGE('',*,*,#14339,.T.);
#19844=ORIENTED_EDGE('',*,*,#14340,.F.);
#19845=ORIENTED_EDGE('',*,*,#14341,.F.);
#19846=ORIENTED_EDGE('',*,*,#14342,.F.);
#19847=ORIENTED_EDGE('',*,*,#14339,.F.);
#19848=ORIENTED_EDGE('',*,*,#14336,.F.);
#19849=ORIENTED_EDGE('',*,*,#14343,.F.);
#19850=ORIENTED_EDGE('',*,*,#14344,.T.);
#19851=ORIENTED_EDGE('',*,*,#14345,.T.);
#19852=ORIENTED_EDGE('',*,*,#14346,.F.);
#19853=ORIENTED_EDGE('',*,*,#14345,.F.);
#19854=ORIENTED_EDGE('',*,*,#14347,.T.);
#19855=ORIENTED_EDGE('',*,*,#14348,.F.);
#19856=ORIENTED_EDGE('',*,*,#14349,.F.);
#19857=ORIENTED_EDGE('',*,*,#14350,.F.);
#19858=ORIENTED_EDGE('',*,*,#14347,.F.);
#19859=ORIENTED_EDGE('',*,*,#14344,.F.);
#19860=ORIENTED_EDGE('',*,*,#14351,.F.);
#19861=ORIENTED_EDGE('',*,*,#14352,.T.);
#19862=ORIENTED_EDGE('',*,*,#14353,.T.);
#19863=ORIENTED_EDGE('',*,*,#14354,.F.);
#19864=ORIENTED_EDGE('',*,*,#14353,.F.);
#19865=ORIENTED_EDGE('',*,*,#14355,.T.);
#19866=ORIENTED_EDGE('',*,*,#14356,.F.);
#19867=ORIENTED_EDGE('',*,*,#14357,.F.);
#19868=ORIENTED_EDGE('',*,*,#14358,.F.);
#19869=ORIENTED_EDGE('',*,*,#14355,.F.);
#19870=ORIENTED_EDGE('',*,*,#14352,.F.);
#19871=ORIENTED_EDGE('',*,*,#14359,.F.);
#19872=ORIENTED_EDGE('',*,*,#14360,.T.);
#19873=ORIENTED_EDGE('',*,*,#14361,.T.);
#19874=ORIENTED_EDGE('',*,*,#14362,.F.);
#19875=ORIENTED_EDGE('',*,*,#14361,.F.);
#19876=ORIENTED_EDGE('',*,*,#14363,.T.);
#19877=ORIENTED_EDGE('',*,*,#14364,.F.);
#19878=ORIENTED_EDGE('',*,*,#14365,.F.);
#19879=ORIENTED_EDGE('',*,*,#14366,.F.);
#19880=ORIENTED_EDGE('',*,*,#14363,.F.);
#19881=ORIENTED_EDGE('',*,*,#14360,.F.);
#19882=ORIENTED_EDGE('',*,*,#14367,.F.);
#19883=ORIENTED_EDGE('',*,*,#14368,.T.);
#19884=ORIENTED_EDGE('',*,*,#14369,.T.);
#19885=ORIENTED_EDGE('',*,*,#14370,.F.);
#19886=ORIENTED_EDGE('',*,*,#14369,.F.);
#19887=ORIENTED_EDGE('',*,*,#14371,.T.);
#19888=ORIENTED_EDGE('',*,*,#14372,.F.);
#19889=ORIENTED_EDGE('',*,*,#14373,.F.);
#19890=ORIENTED_EDGE('',*,*,#14374,.F.);
#19891=ORIENTED_EDGE('',*,*,#14371,.F.);
#19892=ORIENTED_EDGE('',*,*,#14368,.F.);
#19893=ORIENTED_EDGE('',*,*,#14375,.F.);
#19894=ORIENTED_EDGE('',*,*,#14376,.T.);
#19895=ORIENTED_EDGE('',*,*,#14377,.T.);
#19896=ORIENTED_EDGE('',*,*,#14378,.F.);
#19897=ORIENTED_EDGE('',*,*,#14377,.F.);
#19898=ORIENTED_EDGE('',*,*,#14379,.T.);
#19899=ORIENTED_EDGE('',*,*,#14380,.F.);
#19900=ORIENTED_EDGE('',*,*,#14381,.F.);
#19901=ORIENTED_EDGE('',*,*,#14382,.F.);
#19902=ORIENTED_EDGE('',*,*,#14379,.F.);
#19903=ORIENTED_EDGE('',*,*,#14376,.F.);
#19904=ORIENTED_EDGE('',*,*,#14383,.F.);
#19905=ORIENTED_EDGE('',*,*,#14384,.T.);
#19906=ORIENTED_EDGE('',*,*,#14385,.T.);
#19907=ORIENTED_EDGE('',*,*,#14386,.F.);
#19908=ORIENTED_EDGE('',*,*,#14385,.F.);
#19909=ORIENTED_EDGE('',*,*,#14387,.T.);
#19910=ORIENTED_EDGE('',*,*,#14388,.F.);
#19911=ORIENTED_EDGE('',*,*,#14389,.F.);
#19912=ORIENTED_EDGE('',*,*,#14390,.F.);
#19913=ORIENTED_EDGE('',*,*,#14387,.F.);
#19914=ORIENTED_EDGE('',*,*,#14384,.F.);
#19915=ORIENTED_EDGE('',*,*,#14391,.F.);
#19916=ORIENTED_EDGE('',*,*,#14392,.T.);
#19917=ORIENTED_EDGE('',*,*,#14393,.T.);
#19918=ORIENTED_EDGE('',*,*,#14394,.F.);
#19919=ORIENTED_EDGE('',*,*,#14393,.F.);
#19920=ORIENTED_EDGE('',*,*,#14395,.T.);
#19921=ORIENTED_EDGE('',*,*,#14396,.F.);
#19922=ORIENTED_EDGE('',*,*,#14397,.F.);
#19923=ORIENTED_EDGE('',*,*,#14398,.F.);
#19924=ORIENTED_EDGE('',*,*,#14395,.F.);
#19925=ORIENTED_EDGE('',*,*,#14392,.F.);
#19926=ORIENTED_EDGE('',*,*,#14399,.F.);
#19927=ORIENTED_EDGE('',*,*,#14400,.T.);
#19928=ORIENTED_EDGE('',*,*,#14401,.T.);
#19929=ORIENTED_EDGE('',*,*,#14402,.F.);
#19930=ORIENTED_EDGE('',*,*,#14401,.F.);
#19931=ORIENTED_EDGE('',*,*,#14403,.T.);
#19932=ORIENTED_EDGE('',*,*,#14404,.F.);
#19933=ORIENTED_EDGE('',*,*,#14405,.F.);
#19934=ORIENTED_EDGE('',*,*,#14406,.F.);
#19935=ORIENTED_EDGE('',*,*,#14403,.F.);
#19936=ORIENTED_EDGE('',*,*,#14400,.F.);
#19937=ORIENTED_EDGE('',*,*,#14407,.F.);
#19938=ORIENTED_EDGE('',*,*,#14408,.T.);
#19939=ORIENTED_EDGE('',*,*,#14409,.T.);
#19940=ORIENTED_EDGE('',*,*,#14410,.F.);
#19941=ORIENTED_EDGE('',*,*,#14409,.F.);
#19942=ORIENTED_EDGE('',*,*,#14411,.T.);
#19943=ORIENTED_EDGE('',*,*,#14412,.F.);
#19944=ORIENTED_EDGE('',*,*,#14413,.F.);
#19945=ORIENTED_EDGE('',*,*,#14414,.F.);
#19946=ORIENTED_EDGE('',*,*,#14411,.F.);
#19947=ORIENTED_EDGE('',*,*,#14408,.F.);
#19948=ORIENTED_EDGE('',*,*,#14415,.F.);
#19949=ORIENTED_EDGE('',*,*,#14416,.T.);
#19950=ORIENTED_EDGE('',*,*,#14417,.T.);
#19951=ORIENTED_EDGE('',*,*,#14418,.F.);
#19952=ORIENTED_EDGE('',*,*,#14417,.F.);
#19953=ORIENTED_EDGE('',*,*,#14419,.T.);
#19954=ORIENTED_EDGE('',*,*,#14420,.F.);
#19955=ORIENTED_EDGE('',*,*,#14421,.F.);
#19956=ORIENTED_EDGE('',*,*,#14422,.F.);
#19957=ORIENTED_EDGE('',*,*,#14419,.F.);
#19958=ORIENTED_EDGE('',*,*,#14416,.F.);
#19959=ORIENTED_EDGE('',*,*,#14423,.F.);
#19960=ORIENTED_EDGE('',*,*,#14424,.T.);
#19961=ORIENTED_EDGE('',*,*,#14425,.T.);
#19962=ORIENTED_EDGE('',*,*,#14426,.F.);
#19963=ORIENTED_EDGE('',*,*,#14425,.F.);
#19964=ORIENTED_EDGE('',*,*,#14427,.T.);
#19965=ORIENTED_EDGE('',*,*,#14428,.F.);
#19966=ORIENTED_EDGE('',*,*,#14429,.F.);
#19967=ORIENTED_EDGE('',*,*,#14430,.F.);
#19968=ORIENTED_EDGE('',*,*,#14427,.F.);
#19969=ORIENTED_EDGE('',*,*,#14424,.F.);
#19970=ORIENTED_EDGE('',*,*,#14431,.F.);
#19971=ORIENTED_EDGE('',*,*,#14432,.T.);
#19972=ORIENTED_EDGE('',*,*,#14433,.T.);
#19973=ORIENTED_EDGE('',*,*,#14434,.F.);
#19974=ORIENTED_EDGE('',*,*,#14433,.F.);
#19975=ORIENTED_EDGE('',*,*,#14435,.T.);
#19976=ORIENTED_EDGE('',*,*,#14436,.F.);
#19977=ORIENTED_EDGE('',*,*,#14437,.F.);
#19978=ORIENTED_EDGE('',*,*,#14438,.F.);
#19979=ORIENTED_EDGE('',*,*,#14435,.F.);
#19980=ORIENTED_EDGE('',*,*,#14432,.F.);
#19981=ORIENTED_EDGE('',*,*,#14439,.F.);
#19982=ORIENTED_EDGE('',*,*,#14440,.T.);
#19983=ORIENTED_EDGE('',*,*,#14441,.T.);
#19984=ORIENTED_EDGE('',*,*,#14442,.F.);
#19985=ORIENTED_EDGE('',*,*,#14441,.F.);
#19986=ORIENTED_EDGE('',*,*,#14443,.T.);
#19987=ORIENTED_EDGE('',*,*,#14444,.F.);
#19988=ORIENTED_EDGE('',*,*,#14445,.F.);
#19989=ORIENTED_EDGE('',*,*,#14446,.F.);
#19990=ORIENTED_EDGE('',*,*,#14443,.F.);
#19991=ORIENTED_EDGE('',*,*,#14440,.F.);
#19992=ORIENTED_EDGE('',*,*,#14447,.F.);
#19993=ORIENTED_EDGE('',*,*,#14448,.T.);
#19994=ORIENTED_EDGE('',*,*,#14449,.T.);
#19995=ORIENTED_EDGE('',*,*,#14450,.F.);
#19996=ORIENTED_EDGE('',*,*,#14449,.F.);
#19997=ORIENTED_EDGE('',*,*,#14451,.T.);
#19998=ORIENTED_EDGE('',*,*,#14452,.F.);
#19999=ORIENTED_EDGE('',*,*,#14453,.F.);
#20000=ORIENTED_EDGE('',*,*,#14454,.F.);
#20001=ORIENTED_EDGE('',*,*,#14451,.F.);
#20002=ORIENTED_EDGE('',*,*,#14448,.F.);
#20003=ORIENTED_EDGE('',*,*,#14455,.F.);
#20004=ORIENTED_EDGE('',*,*,#14456,.T.);
#20005=ORIENTED_EDGE('',*,*,#14457,.T.);
#20006=ORIENTED_EDGE('',*,*,#14458,.F.);
#20007=ORIENTED_EDGE('',*,*,#14459,.F.);
#20008=ORIENTED_EDGE('',*,*,#14457,.F.);
#20009=ORIENTED_EDGE('',*,*,#14460,.T.);
#20010=ORIENTED_EDGE('',*,*,#14461,.F.);
#20011=ORIENTED_EDGE('',*,*,#14462,.F.);
#20012=ORIENTED_EDGE('',*,*,#14463,.F.);
#20013=ORIENTED_EDGE('',*,*,#14460,.F.);
#20014=ORIENTED_EDGE('',*,*,#14456,.F.);
#20015=ORIENTED_EDGE('',*,*,#14464,.F.);
#20016=ORIENTED_EDGE('',*,*,#14465,.T.);
#20017=ORIENTED_EDGE('',*,*,#14466,.T.);
#20018=ORIENTED_EDGE('',*,*,#14467,.F.);
#20019=ORIENTED_EDGE('',*,*,#14466,.F.);
#20020=ORIENTED_EDGE('',*,*,#14468,.T.);
#20021=ORIENTED_EDGE('',*,*,#14469,.F.);
#20022=ORIENTED_EDGE('',*,*,#14470,.F.);
#20023=ORIENTED_EDGE('',*,*,#14471,.F.);
#20024=ORIENTED_EDGE('',*,*,#14468,.F.);
#20025=ORIENTED_EDGE('',*,*,#14465,.F.);
#20026=ORIENTED_EDGE('',*,*,#14472,.F.);
#20027=ORIENTED_EDGE('',*,*,#14473,.T.);
#20028=ORIENTED_EDGE('',*,*,#14474,.T.);
#20029=ORIENTED_EDGE('',*,*,#14475,.F.);
#20030=ORIENTED_EDGE('',*,*,#14474,.F.);
#20031=ORIENTED_EDGE('',*,*,#14476,.T.);
#20032=ORIENTED_EDGE('',*,*,#14477,.F.);
#20033=ORIENTED_EDGE('',*,*,#14478,.F.);
#20034=ORIENTED_EDGE('',*,*,#14479,.F.);
#20035=ORIENTED_EDGE('',*,*,#14476,.F.);
#20036=ORIENTED_EDGE('',*,*,#14473,.F.);
#20037=ORIENTED_EDGE('',*,*,#14480,.F.);
#20038=ORIENTED_EDGE('',*,*,#14481,.T.);
#20039=ORIENTED_EDGE('',*,*,#14482,.T.);
#20040=ORIENTED_EDGE('',*,*,#14483,.F.);
#20041=ORIENTED_EDGE('',*,*,#14482,.F.);
#20042=ORIENTED_EDGE('',*,*,#14484,.T.);
#20043=ORIENTED_EDGE('',*,*,#14485,.F.);
#20044=ORIENTED_EDGE('',*,*,#14486,.F.);
#20045=ORIENTED_EDGE('',*,*,#14487,.F.);
#20046=ORIENTED_EDGE('',*,*,#14484,.F.);
#20047=ORIENTED_EDGE('',*,*,#14481,.F.);
#20048=ORIENTED_EDGE('',*,*,#14488,.F.);
#20049=ORIENTED_EDGE('',*,*,#14489,.T.);
#20050=ORIENTED_EDGE('',*,*,#14490,.T.);
#20051=ORIENTED_EDGE('',*,*,#14491,.F.);
#20052=ORIENTED_EDGE('',*,*,#14490,.F.);
#20053=ORIENTED_EDGE('',*,*,#14492,.T.);
#20054=ORIENTED_EDGE('',*,*,#14493,.F.);
#20055=ORIENTED_EDGE('',*,*,#14494,.F.);
#20056=ORIENTED_EDGE('',*,*,#14495,.F.);
#20057=ORIENTED_EDGE('',*,*,#14492,.F.);
#20058=ORIENTED_EDGE('',*,*,#14489,.F.);
#20059=ORIENTED_EDGE('',*,*,#14496,.F.);
#20060=ORIENTED_EDGE('',*,*,#14497,.T.);
#20061=ORIENTED_EDGE('',*,*,#14498,.T.);
#20062=ORIENTED_EDGE('',*,*,#14499,.F.);
#20063=ORIENTED_EDGE('',*,*,#14498,.F.);
#20064=ORIENTED_EDGE('',*,*,#14500,.T.);
#20065=ORIENTED_EDGE('',*,*,#14501,.F.);
#20066=ORIENTED_EDGE('',*,*,#14502,.F.);
#20067=ORIENTED_EDGE('',*,*,#14503,.F.);
#20068=ORIENTED_EDGE('',*,*,#14500,.F.);
#20069=ORIENTED_EDGE('',*,*,#14497,.F.);
#20070=ORIENTED_EDGE('',*,*,#14504,.F.);
#20071=ORIENTED_EDGE('',*,*,#14505,.T.);
#20072=ORIENTED_EDGE('',*,*,#14506,.T.);
#20073=ORIENTED_EDGE('',*,*,#14507,.F.);
#20074=ORIENTED_EDGE('',*,*,#14506,.F.);
#20075=ORIENTED_EDGE('',*,*,#14508,.T.);
#20076=ORIENTED_EDGE('',*,*,#14509,.F.);
#20077=ORIENTED_EDGE('',*,*,#14510,.F.);
#20078=ORIENTED_EDGE('',*,*,#14511,.F.);
#20079=ORIENTED_EDGE('',*,*,#14508,.F.);
#20080=ORIENTED_EDGE('',*,*,#14505,.F.);
#20081=ORIENTED_EDGE('',*,*,#14512,.F.);
#20082=ORIENTED_EDGE('',*,*,#14513,.T.);
#20083=ORIENTED_EDGE('',*,*,#14514,.T.);
#20084=ORIENTED_EDGE('',*,*,#14515,.F.);
#20085=ORIENTED_EDGE('',*,*,#14514,.F.);
#20086=ORIENTED_EDGE('',*,*,#14516,.T.);
#20087=ORIENTED_EDGE('',*,*,#14517,.F.);
#20088=ORIENTED_EDGE('',*,*,#14518,.F.);
#20089=ORIENTED_EDGE('',*,*,#14519,.F.);
#20090=ORIENTED_EDGE('',*,*,#14516,.F.);
#20091=ORIENTED_EDGE('',*,*,#14513,.F.);
#20092=ORIENTED_EDGE('',*,*,#14520,.F.);
#20093=ORIENTED_EDGE('',*,*,#14521,.T.);
#20094=ORIENTED_EDGE('',*,*,#14522,.T.);
#20095=ORIENTED_EDGE('',*,*,#14523,.F.);
#20096=ORIENTED_EDGE('',*,*,#14522,.F.);
#20097=ORIENTED_EDGE('',*,*,#14524,.T.);
#20098=ORIENTED_EDGE('',*,*,#14525,.F.);
#20099=ORIENTED_EDGE('',*,*,#14526,.F.);
#20100=ORIENTED_EDGE('',*,*,#14527,.F.);
#20101=ORIENTED_EDGE('',*,*,#14524,.F.);
#20102=ORIENTED_EDGE('',*,*,#14521,.F.);
#20103=ORIENTED_EDGE('',*,*,#14528,.F.);
#20104=ORIENTED_EDGE('',*,*,#14529,.T.);
#20105=ORIENTED_EDGE('',*,*,#14530,.T.);
#20106=ORIENTED_EDGE('',*,*,#14531,.F.);
#20107=ORIENTED_EDGE('',*,*,#14530,.F.);
#20108=ORIENTED_EDGE('',*,*,#14532,.T.);
#20109=ORIENTED_EDGE('',*,*,#14533,.F.);
#20110=ORIENTED_EDGE('',*,*,#14534,.F.);
#20111=ORIENTED_EDGE('',*,*,#14535,.F.);
#20112=ORIENTED_EDGE('',*,*,#14532,.F.);
#20113=ORIENTED_EDGE('',*,*,#14529,.F.);
#20114=ORIENTED_EDGE('',*,*,#14536,.F.);
#20115=ORIENTED_EDGE('',*,*,#14537,.T.);
#20116=ORIENTED_EDGE('',*,*,#14538,.T.);
#20117=ORIENTED_EDGE('',*,*,#14539,.F.);
#20118=ORIENTED_EDGE('',*,*,#14538,.F.);
#20119=ORIENTED_EDGE('',*,*,#14540,.T.);
#20120=ORIENTED_EDGE('',*,*,#14541,.F.);
#20121=ORIENTED_EDGE('',*,*,#14542,.F.);
#20122=ORIENTED_EDGE('',*,*,#14543,.F.);
#20123=ORIENTED_EDGE('',*,*,#14540,.F.);
#20124=ORIENTED_EDGE('',*,*,#14537,.F.);
#20125=ORIENTED_EDGE('',*,*,#14544,.F.);
#20126=ORIENTED_EDGE('',*,*,#14545,.T.);
#20127=ORIENTED_EDGE('',*,*,#14546,.T.);
#20128=ORIENTED_EDGE('',*,*,#14547,.F.);
#20129=ORIENTED_EDGE('',*,*,#14546,.F.);
#20130=ORIENTED_EDGE('',*,*,#14548,.T.);
#20131=ORIENTED_EDGE('',*,*,#14549,.F.);
#20132=ORIENTED_EDGE('',*,*,#14550,.F.);
#20133=ORIENTED_EDGE('',*,*,#14551,.F.);
#20134=ORIENTED_EDGE('',*,*,#14548,.F.);
#20135=ORIENTED_EDGE('',*,*,#14545,.F.);
#20136=ORIENTED_EDGE('',*,*,#14552,.F.);
#20137=ORIENTED_EDGE('',*,*,#14553,.T.);
#20138=ORIENTED_EDGE('',*,*,#14554,.T.);
#20139=ORIENTED_EDGE('',*,*,#14555,.F.);
#20140=ORIENTED_EDGE('',*,*,#14554,.F.);
#20141=ORIENTED_EDGE('',*,*,#14556,.T.);
#20142=ORIENTED_EDGE('',*,*,#14557,.F.);
#20143=ORIENTED_EDGE('',*,*,#14558,.F.);
#20144=ORIENTED_EDGE('',*,*,#14559,.F.);
#20145=ORIENTED_EDGE('',*,*,#14556,.F.);
#20146=ORIENTED_EDGE('',*,*,#14553,.F.);
#20147=ORIENTED_EDGE('',*,*,#14560,.F.);
#20148=ORIENTED_EDGE('',*,*,#14561,.T.);
#20149=ORIENTED_EDGE('',*,*,#14562,.T.);
#20150=ORIENTED_EDGE('',*,*,#14563,.F.);
#20151=ORIENTED_EDGE('',*,*,#14562,.F.);
#20152=ORIENTED_EDGE('',*,*,#14564,.T.);
#20153=ORIENTED_EDGE('',*,*,#14565,.F.);
#20154=ORIENTED_EDGE('',*,*,#14566,.F.);
#20155=ORIENTED_EDGE('',*,*,#14567,.F.);
#20156=ORIENTED_EDGE('',*,*,#14564,.F.);
#20157=ORIENTED_EDGE('',*,*,#14561,.F.);
#20158=ORIENTED_EDGE('',*,*,#14568,.F.);
#20159=ORIENTED_EDGE('',*,*,#14569,.T.);
#20160=ORIENTED_EDGE('',*,*,#14570,.T.);
#20161=ORIENTED_EDGE('',*,*,#14571,.F.);
#20162=ORIENTED_EDGE('',*,*,#14570,.F.);
#20163=ORIENTED_EDGE('',*,*,#14572,.T.);
#20164=ORIENTED_EDGE('',*,*,#14573,.F.);
#20165=ORIENTED_EDGE('',*,*,#14574,.F.);
#20166=ORIENTED_EDGE('',*,*,#14575,.F.);
#20167=ORIENTED_EDGE('',*,*,#14572,.F.);
#20168=ORIENTED_EDGE('',*,*,#14569,.F.);
#20169=ORIENTED_EDGE('',*,*,#14576,.F.);
#20170=ORIENTED_EDGE('',*,*,#14577,.T.);
#20171=ORIENTED_EDGE('',*,*,#14578,.T.);
#20172=ORIENTED_EDGE('',*,*,#14579,.F.);
#20173=ORIENTED_EDGE('',*,*,#14578,.F.);
#20174=ORIENTED_EDGE('',*,*,#14580,.T.);
#20175=ORIENTED_EDGE('',*,*,#14581,.F.);
#20176=ORIENTED_EDGE('',*,*,#14582,.F.);
#20177=ORIENTED_EDGE('',*,*,#14583,.F.);
#20178=ORIENTED_EDGE('',*,*,#14580,.F.);
#20179=ORIENTED_EDGE('',*,*,#14577,.F.);
#20180=ORIENTED_EDGE('',*,*,#14584,.F.);
#20181=ORIENTED_EDGE('',*,*,#14585,.T.);
#20182=ORIENTED_EDGE('',*,*,#14586,.T.);
#20183=ORIENTED_EDGE('',*,*,#14587,.F.);
#20184=ORIENTED_EDGE('',*,*,#14586,.F.);
#20185=ORIENTED_EDGE('',*,*,#14588,.T.);
#20186=ORIENTED_EDGE('',*,*,#14589,.F.);
#20187=ORIENTED_EDGE('',*,*,#14590,.F.);
#20188=ORIENTED_EDGE('',*,*,#14591,.F.);
#20189=ORIENTED_EDGE('',*,*,#14588,.F.);
#20190=ORIENTED_EDGE('',*,*,#14585,.F.);
#20191=ORIENTED_EDGE('',*,*,#14592,.F.);
#20192=ORIENTED_EDGE('',*,*,#14593,.T.);
#20193=ORIENTED_EDGE('',*,*,#14594,.T.);
#20194=ORIENTED_EDGE('',*,*,#14595,.F.);
#20195=ORIENTED_EDGE('',*,*,#14594,.F.);
#20196=ORIENTED_EDGE('',*,*,#14596,.T.);
#20197=ORIENTED_EDGE('',*,*,#14597,.F.);
#20198=ORIENTED_EDGE('',*,*,#14598,.F.);
#20199=ORIENTED_EDGE('',*,*,#14599,.F.);
#20200=ORIENTED_EDGE('',*,*,#14596,.F.);
#20201=ORIENTED_EDGE('',*,*,#14593,.F.);
#20202=ORIENTED_EDGE('',*,*,#14325,.T.);
#20203=ORIENTED_EDGE('',*,*,#14319,.T.);
#20204=ORIENTED_EDGE('',*,*,#14322,.T.);
#20205=ORIENTED_EDGE('',*,*,#14600,.F.);
#20206=ORIENTED_EDGE('',*,*,#14333,.T.);
#20207=ORIENTED_EDGE('',*,*,#14327,.T.);
#20208=ORIENTED_EDGE('',*,*,#14330,.T.);
#20209=ORIENTED_EDGE('',*,*,#14601,.F.);
#20210=ORIENTED_EDGE('',*,*,#14341,.T.);
#20211=ORIENTED_EDGE('',*,*,#14335,.T.);
#20212=ORIENTED_EDGE('',*,*,#14338,.T.);
#20213=ORIENTED_EDGE('',*,*,#14602,.F.);
#20214=ORIENTED_EDGE('',*,*,#14349,.T.);
#20215=ORIENTED_EDGE('',*,*,#14343,.T.);
#20216=ORIENTED_EDGE('',*,*,#14346,.T.);
#20217=ORIENTED_EDGE('',*,*,#14603,.F.);
#20218=ORIENTED_EDGE('',*,*,#14357,.T.);
#20219=ORIENTED_EDGE('',*,*,#14351,.T.);
#20220=ORIENTED_EDGE('',*,*,#14354,.T.);
#20221=ORIENTED_EDGE('',*,*,#14604,.F.);
#20222=ORIENTED_EDGE('',*,*,#14365,.T.);
#20223=ORIENTED_EDGE('',*,*,#14359,.T.);
#20224=ORIENTED_EDGE('',*,*,#14362,.T.);
#20225=ORIENTED_EDGE('',*,*,#14605,.F.);
#20226=ORIENTED_EDGE('',*,*,#14373,.T.);
#20227=ORIENTED_EDGE('',*,*,#14367,.T.);
#20228=ORIENTED_EDGE('',*,*,#14370,.T.);
#20229=ORIENTED_EDGE('',*,*,#14606,.F.);
#20230=ORIENTED_EDGE('',*,*,#14381,.T.);
#20231=ORIENTED_EDGE('',*,*,#14375,.T.);
#20232=ORIENTED_EDGE('',*,*,#14378,.T.);
#20233=ORIENTED_EDGE('',*,*,#14607,.F.);
#20234=ORIENTED_EDGE('',*,*,#14389,.T.);
#20235=ORIENTED_EDGE('',*,*,#14383,.T.);
#20236=ORIENTED_EDGE('',*,*,#14386,.T.);
#20237=ORIENTED_EDGE('',*,*,#14608,.F.);
#20238=ORIENTED_EDGE('',*,*,#14397,.T.);
#20239=ORIENTED_EDGE('',*,*,#14391,.T.);
#20240=ORIENTED_EDGE('',*,*,#14394,.T.);
#20241=ORIENTED_EDGE('',*,*,#14609,.F.);
#20242=ORIENTED_EDGE('',*,*,#14405,.T.);
#20243=ORIENTED_EDGE('',*,*,#14399,.T.);
#20244=ORIENTED_EDGE('',*,*,#14402,.T.);
#20245=ORIENTED_EDGE('',*,*,#14610,.F.);
#20246=ORIENTED_EDGE('',*,*,#14413,.T.);
#20247=ORIENTED_EDGE('',*,*,#14407,.T.);
#20248=ORIENTED_EDGE('',*,*,#14410,.T.);
#20249=ORIENTED_EDGE('',*,*,#14611,.F.);
#20250=ORIENTED_EDGE('',*,*,#14421,.T.);
#20251=ORIENTED_EDGE('',*,*,#14415,.T.);
#20252=ORIENTED_EDGE('',*,*,#14418,.T.);
#20253=ORIENTED_EDGE('',*,*,#14612,.F.);
#20254=ORIENTED_EDGE('',*,*,#14429,.T.);
#20255=ORIENTED_EDGE('',*,*,#14423,.T.);
#20256=ORIENTED_EDGE('',*,*,#14426,.T.);
#20257=ORIENTED_EDGE('',*,*,#14613,.F.);
#20258=ORIENTED_EDGE('',*,*,#14437,.T.);
#20259=ORIENTED_EDGE('',*,*,#14431,.T.);
#20260=ORIENTED_EDGE('',*,*,#14434,.T.);
#20261=ORIENTED_EDGE('',*,*,#14614,.F.);
#20262=ORIENTED_EDGE('',*,*,#14445,.T.);
#20263=ORIENTED_EDGE('',*,*,#14439,.T.);
#20264=ORIENTED_EDGE('',*,*,#14442,.T.);
#20265=ORIENTED_EDGE('',*,*,#14615,.F.);
#20266=ORIENTED_EDGE('',*,*,#14453,.T.);
#20267=ORIENTED_EDGE('',*,*,#14447,.T.);
#20268=ORIENTED_EDGE('',*,*,#14450,.T.);
#20269=ORIENTED_EDGE('',*,*,#14616,.F.);
#20270=ORIENTED_EDGE('',*,*,#14462,.T.);
#20271=ORIENTED_EDGE('',*,*,#14455,.T.);
#20272=ORIENTED_EDGE('',*,*,#14617,.T.);
#20273=ORIENTED_EDGE('',*,*,#14618,.T.);
#20274=ORIENTED_EDGE('',*,*,#14617,.F.);
#20275=ORIENTED_EDGE('',*,*,#14458,.T.);
#20276=ORIENTED_EDGE('',*,*,#14459,.T.);
#20277=ORIENTED_EDGE('',*,*,#14619,.F.);
#20278=ORIENTED_EDGE('',*,*,#14470,.T.);
#20279=ORIENTED_EDGE('',*,*,#14464,.T.);
#20280=ORIENTED_EDGE('',*,*,#14467,.T.);
#20281=ORIENTED_EDGE('',*,*,#14620,.F.);
#20282=ORIENTED_EDGE('',*,*,#14478,.T.);
#20283=ORIENTED_EDGE('',*,*,#14472,.T.);
#20284=ORIENTED_EDGE('',*,*,#14475,.T.);
#20285=ORIENTED_EDGE('',*,*,#14621,.F.);
#20286=ORIENTED_EDGE('',*,*,#14486,.T.);
#20287=ORIENTED_EDGE('',*,*,#14480,.T.);
#20288=ORIENTED_EDGE('',*,*,#14483,.T.);
#20289=ORIENTED_EDGE('',*,*,#14622,.F.);
#20290=ORIENTED_EDGE('',*,*,#14494,.T.);
#20291=ORIENTED_EDGE('',*,*,#14488,.T.);
#20292=ORIENTED_EDGE('',*,*,#14491,.T.);
#20293=ORIENTED_EDGE('',*,*,#14623,.F.);
#20294=ORIENTED_EDGE('',*,*,#14502,.T.);
#20295=ORIENTED_EDGE('',*,*,#14496,.T.);
#20296=ORIENTED_EDGE('',*,*,#14499,.T.);
#20297=ORIENTED_EDGE('',*,*,#14624,.F.);
#20298=ORIENTED_EDGE('',*,*,#14510,.T.);
#20299=ORIENTED_EDGE('',*,*,#14504,.T.);
#20300=ORIENTED_EDGE('',*,*,#14507,.T.);
#20301=ORIENTED_EDGE('',*,*,#14625,.F.);
#20302=ORIENTED_EDGE('',*,*,#14518,.T.);
#20303=ORIENTED_EDGE('',*,*,#14512,.T.);
#20304=ORIENTED_EDGE('',*,*,#14515,.T.);
#20305=ORIENTED_EDGE('',*,*,#14626,.F.);
#20306=ORIENTED_EDGE('',*,*,#14526,.T.);
#20307=ORIENTED_EDGE('',*,*,#14520,.T.);
#20308=ORIENTED_EDGE('',*,*,#14523,.T.);
#20309=ORIENTED_EDGE('',*,*,#14627,.F.);
#20310=ORIENTED_EDGE('',*,*,#14534,.T.);
#20311=ORIENTED_EDGE('',*,*,#14528,.T.);
#20312=ORIENTED_EDGE('',*,*,#14531,.T.);
#20313=ORIENTED_EDGE('',*,*,#14628,.F.);
#20314=ORIENTED_EDGE('',*,*,#14542,.T.);
#20315=ORIENTED_EDGE('',*,*,#14536,.T.);
#20316=ORIENTED_EDGE('',*,*,#14539,.T.);
#20317=ORIENTED_EDGE('',*,*,#14629,.F.);
#20318=ORIENTED_EDGE('',*,*,#14550,.T.);
#20319=ORIENTED_EDGE('',*,*,#14544,.T.);
#20320=ORIENTED_EDGE('',*,*,#14547,.T.);
#20321=ORIENTED_EDGE('',*,*,#14630,.F.);
#20322=ORIENTED_EDGE('',*,*,#14558,.T.);
#20323=ORIENTED_EDGE('',*,*,#14552,.T.);
#20324=ORIENTED_EDGE('',*,*,#14555,.T.);
#20325=ORIENTED_EDGE('',*,*,#14631,.F.);
#20326=ORIENTED_EDGE('',*,*,#14566,.T.);
#20327=ORIENTED_EDGE('',*,*,#14560,.T.);
#20328=ORIENTED_EDGE('',*,*,#14563,.T.);
#20329=ORIENTED_EDGE('',*,*,#14632,.F.);
#20330=ORIENTED_EDGE('',*,*,#14574,.T.);
#20331=ORIENTED_EDGE('',*,*,#14568,.T.);
#20332=ORIENTED_EDGE('',*,*,#14571,.T.);
#20333=ORIENTED_EDGE('',*,*,#14633,.F.);
#20334=ORIENTED_EDGE('',*,*,#14582,.T.);
#20335=ORIENTED_EDGE('',*,*,#14576,.T.);
#20336=ORIENTED_EDGE('',*,*,#14579,.T.);
#20337=ORIENTED_EDGE('',*,*,#14634,.F.);
#20338=ORIENTED_EDGE('',*,*,#14590,.T.);
#20339=ORIENTED_EDGE('',*,*,#14584,.T.);
#20340=ORIENTED_EDGE('',*,*,#14587,.T.);
#20341=ORIENTED_EDGE('',*,*,#14635,.F.);
#20342=ORIENTED_EDGE('',*,*,#14598,.T.);
#20343=ORIENTED_EDGE('',*,*,#14592,.T.);
#20344=ORIENTED_EDGE('',*,*,#14595,.T.);
#20345=ORIENTED_EDGE('',*,*,#14636,.F.);
#20346=ORIENTED_EDGE('',*,*,#14637,.T.);
#20347=ORIENTED_EDGE('',*,*,#14638,.T.);
#20348=ORIENTED_EDGE('',*,*,#14639,.T.);
#20349=ORIENTED_EDGE('',*,*,#14640,.F.);
#20350=ORIENTED_EDGE('',*,*,#14639,.F.);
#20351=ORIENTED_EDGE('',*,*,#14641,.F.);
#20352=ORIENTED_EDGE('',*,*,#14642,.T.);
#20353=ORIENTED_EDGE('',*,*,#14643,.F.);
#20354=ORIENTED_EDGE('',*,*,#14644,.F.);
#20355=ORIENTED_EDGE('',*,*,#14642,.F.);
#20356=ORIENTED_EDGE('',*,*,#14645,.F.);
#20357=ORIENTED_EDGE('',*,*,#14637,.F.);
#20358=ORIENTED_EDGE('',*,*,#14638,.F.);
#20359=ORIENTED_EDGE('',*,*,#14645,.T.);
#20360=ORIENTED_EDGE('',*,*,#14641,.T.);
#20361=ORIENTED_EDGE('',*,*,#14646,.F.);
#20362=ORIENTED_EDGE('',*,*,#14647,.T.);
#20363=ORIENTED_EDGE('',*,*,#14463,.T.);
#20364=ORIENTED_EDGE('',*,*,#14616,.T.);
#20365=ORIENTED_EDGE('',*,*,#14452,.T.);
#20366=ORIENTED_EDGE('',*,*,#14454,.T.);
#20367=ORIENTED_EDGE('',*,*,#14615,.T.);
#20368=ORIENTED_EDGE('',*,*,#14444,.T.);
#20369=ORIENTED_EDGE('',*,*,#14446,.T.);
#20370=ORIENTED_EDGE('',*,*,#14614,.T.);
#20371=ORIENTED_EDGE('',*,*,#14436,.T.);
#20372=ORIENTED_EDGE('',*,*,#14438,.T.);
#20373=ORIENTED_EDGE('',*,*,#14613,.T.);
#20374=ORIENTED_EDGE('',*,*,#14428,.T.);
#20375=ORIENTED_EDGE('',*,*,#14430,.T.);
#20376=ORIENTED_EDGE('',*,*,#14612,.T.);
#20377=ORIENTED_EDGE('',*,*,#14420,.T.);
#20378=ORIENTED_EDGE('',*,*,#14422,.T.);
#20379=ORIENTED_EDGE('',*,*,#14611,.T.);
#20380=ORIENTED_EDGE('',*,*,#14412,.T.);
#20381=ORIENTED_EDGE('',*,*,#14414,.T.);
#20382=ORIENTED_EDGE('',*,*,#14610,.T.);
#20383=ORIENTED_EDGE('',*,*,#14404,.T.);
#20384=ORIENTED_EDGE('',*,*,#14406,.T.);
#20385=ORIENTED_EDGE('',*,*,#14609,.T.);
#20386=ORIENTED_EDGE('',*,*,#14396,.T.);
#20387=ORIENTED_EDGE('',*,*,#14398,.T.);
#20388=ORIENTED_EDGE('',*,*,#14608,.T.);
#20389=ORIENTED_EDGE('',*,*,#14388,.T.);
#20390=ORIENTED_EDGE('',*,*,#14390,.T.);
#20391=ORIENTED_EDGE('',*,*,#14607,.T.);
#20392=ORIENTED_EDGE('',*,*,#14380,.T.);
#20393=ORIENTED_EDGE('',*,*,#14382,.T.);
#20394=ORIENTED_EDGE('',*,*,#14606,.T.);
#20395=ORIENTED_EDGE('',*,*,#14372,.T.);
#20396=ORIENTED_EDGE('',*,*,#14374,.T.);
#20397=ORIENTED_EDGE('',*,*,#14605,.T.);
#20398=ORIENTED_EDGE('',*,*,#14364,.T.);
#20399=ORIENTED_EDGE('',*,*,#14366,.T.);
#20400=ORIENTED_EDGE('',*,*,#14604,.T.);
#20401=ORIENTED_EDGE('',*,*,#14356,.T.);
#20402=ORIENTED_EDGE('',*,*,#14358,.T.);
#20403=ORIENTED_EDGE('',*,*,#14603,.T.);
#20404=ORIENTED_EDGE('',*,*,#14348,.T.);
#20405=ORIENTED_EDGE('',*,*,#14350,.T.);
#20406=ORIENTED_EDGE('',*,*,#14602,.T.);
#20407=ORIENTED_EDGE('',*,*,#14340,.T.);
#20408=ORIENTED_EDGE('',*,*,#14342,.T.);
#20409=ORIENTED_EDGE('',*,*,#14601,.T.);
#20410=ORIENTED_EDGE('',*,*,#14332,.T.);
#20411=ORIENTED_EDGE('',*,*,#14334,.T.);
#20412=ORIENTED_EDGE('',*,*,#14600,.T.);
#20413=ORIENTED_EDGE('',*,*,#14324,.T.);
#20414=ORIENTED_EDGE('',*,*,#14326,.T.);
#20415=ORIENTED_EDGE('',*,*,#14640,.T.);
#20416=ORIENTED_EDGE('',*,*,#14643,.T.);
#20417=ORIENTED_EDGE('',*,*,#14644,.T.);
#20418=ORIENTED_EDGE('',*,*,#14636,.T.);
#20419=ORIENTED_EDGE('',*,*,#14597,.T.);
#20420=ORIENTED_EDGE('',*,*,#14599,.T.);
#20421=ORIENTED_EDGE('',*,*,#14635,.T.);
#20422=ORIENTED_EDGE('',*,*,#14589,.T.);
#20423=ORIENTED_EDGE('',*,*,#14591,.T.);
#20424=ORIENTED_EDGE('',*,*,#14634,.T.);
#20425=ORIENTED_EDGE('',*,*,#14581,.T.);
#20426=ORIENTED_EDGE('',*,*,#14583,.T.);
#20427=ORIENTED_EDGE('',*,*,#14633,.T.);
#20428=ORIENTED_EDGE('',*,*,#14573,.T.);
#20429=ORIENTED_EDGE('',*,*,#14575,.T.);
#20430=ORIENTED_EDGE('',*,*,#14632,.T.);
#20431=ORIENTED_EDGE('',*,*,#14565,.T.);
#20432=ORIENTED_EDGE('',*,*,#14567,.T.);
#20433=ORIENTED_EDGE('',*,*,#14631,.T.);
#20434=ORIENTED_EDGE('',*,*,#14557,.T.);
#20435=ORIENTED_EDGE('',*,*,#14559,.T.);
#20436=ORIENTED_EDGE('',*,*,#14630,.T.);
#20437=ORIENTED_EDGE('',*,*,#14549,.T.);
#20438=ORIENTED_EDGE('',*,*,#14551,.T.);
#20439=ORIENTED_EDGE('',*,*,#14629,.T.);
#20440=ORIENTED_EDGE('',*,*,#14541,.T.);
#20441=ORIENTED_EDGE('',*,*,#14543,.T.);
#20442=ORIENTED_EDGE('',*,*,#14628,.T.);
#20443=ORIENTED_EDGE('',*,*,#14533,.T.);
#20444=ORIENTED_EDGE('',*,*,#14535,.T.);
#20445=ORIENTED_EDGE('',*,*,#14627,.T.);
#20446=ORIENTED_EDGE('',*,*,#14525,.T.);
#20447=ORIENTED_EDGE('',*,*,#14527,.T.);
#20448=ORIENTED_EDGE('',*,*,#14626,.T.);
#20449=ORIENTED_EDGE('',*,*,#14517,.T.);
#20450=ORIENTED_EDGE('',*,*,#14519,.T.);
#20451=ORIENTED_EDGE('',*,*,#14625,.T.);
#20452=ORIENTED_EDGE('',*,*,#14509,.T.);
#20453=ORIENTED_EDGE('',*,*,#14511,.T.);
#20454=ORIENTED_EDGE('',*,*,#14624,.T.);
#20455=ORIENTED_EDGE('',*,*,#14501,.T.);
#20456=ORIENTED_EDGE('',*,*,#14503,.T.);
#20457=ORIENTED_EDGE('',*,*,#14623,.T.);
#20458=ORIENTED_EDGE('',*,*,#14493,.T.);
#20459=ORIENTED_EDGE('',*,*,#14495,.T.);
#20460=ORIENTED_EDGE('',*,*,#14622,.T.);
#20461=ORIENTED_EDGE('',*,*,#14485,.T.);
#20462=ORIENTED_EDGE('',*,*,#14487,.T.);
#20463=ORIENTED_EDGE('',*,*,#14621,.T.);
#20464=ORIENTED_EDGE('',*,*,#14477,.T.);
#20465=ORIENTED_EDGE('',*,*,#14479,.T.);
#20466=ORIENTED_EDGE('',*,*,#14620,.T.);
#20467=ORIENTED_EDGE('',*,*,#14469,.T.);
#20468=ORIENTED_EDGE('',*,*,#14471,.T.);
#20469=ORIENTED_EDGE('',*,*,#14619,.T.);
#20470=ORIENTED_EDGE('',*,*,#14461,.T.);
#20471=ORIENTED_EDGE('',*,*,#14647,.F.);
#20472=ORIENTED_EDGE('',*,*,#14648,.T.);
#20473=ORIENTED_EDGE('',*,*,#14649,.F.);
#20474=ORIENTED_EDGE('',*,*,#14648,.F.);
#20475=ORIENTED_EDGE('',*,*,#14650,.F.);
#20476=ORIENTED_EDGE('',*,*,#14651,.T.);
#20477=ORIENTED_EDGE('',*,*,#14652,.T.);
#20478=ORIENTED_EDGE('',*,*,#14653,.F.);
#20479=ORIENTED_EDGE('',*,*,#14654,.F.);
#20480=ORIENTED_EDGE('',*,*,#14655,.T.);
#20481=ORIENTED_EDGE('',*,*,#14656,.T.);
#20482=ORIENTED_EDGE('',*,*,#14651,.F.);
#20483=ORIENTED_EDGE('',*,*,#14657,.F.);
#20484=ORIENTED_EDGE('',*,*,#14658,.T.);
#20485=ORIENTED_EDGE('',*,*,#14659,.T.);
#20486=ORIENTED_EDGE('',*,*,#14655,.F.);
#20487=ORIENTED_EDGE('',*,*,#14660,.F.);
#20488=ORIENTED_EDGE('',*,*,#14661,.T.);
#20489=ORIENTED_EDGE('',*,*,#14662,.T.);
#20490=ORIENTED_EDGE('',*,*,#14658,.F.);
#20491=ORIENTED_EDGE('',*,*,#14663,.F.);
#20492=ORIENTED_EDGE('',*,*,#14664,.T.);
#20493=ORIENTED_EDGE('',*,*,#14665,.T.);
#20494=ORIENTED_EDGE('',*,*,#14661,.F.);
#20495=ORIENTED_EDGE('',*,*,#14666,.F.);
#20496=ORIENTED_EDGE('',*,*,#14653,.T.);
#20497=ORIENTED_EDGE('',*,*,#14667,.T.);
#20498=ORIENTED_EDGE('',*,*,#14664,.F.);
#20499=ORIENTED_EDGE('',*,*,#14667,.F.);
#20500=ORIENTED_EDGE('',*,*,#14652,.F.);
#20501=ORIENTED_EDGE('',*,*,#14656,.F.);
#20502=ORIENTED_EDGE('',*,*,#14659,.F.);
#20503=ORIENTED_EDGE('',*,*,#14662,.F.);
#20504=ORIENTED_EDGE('',*,*,#14665,.F.);
#20505=ORIENTED_EDGE('',*,*,#14649,.T.);
#20506=ORIENTED_EDGE('',*,*,#14668,.F.);
#20507=ORIENTED_EDGE('',*,*,#14136,.F.);
#20508=ORIENTED_EDGE('',*,*,#14669,.T.);
#20509=ORIENTED_EDGE('',*,*,#14668,.T.);
#20510=ORIENTED_EDGE('',*,*,#14669,.F.);
#20511=ORIENTED_EDGE('',*,*,#14217,.T.);
#20512=ORIENTED_EDGE('',*,*,#14313,.T.);
#20513=ORIENTED_EDGE('',*,*,#14670,.F.);
#20514=ORIENTED_EDGE('',*,*,#14318,.T.);
#20515=ORIENTED_EDGE('',*,*,#14671,.F.);
#20516=ORIENTED_EDGE('',*,*,#14672,.T.);
#20517=ORIENTED_EDGE('',*,*,#14310,.T.);
#20518=ORIENTED_EDGE('',*,*,#14670,.T.);
#20519=ORIENTED_EDGE('',*,*,#14311,.T.);
#20520=ORIENTED_EDGE('',*,*,#14672,.F.);
#20521=ORIENTED_EDGE('',*,*,#14618,.F.);
#20522=ORIENTED_EDGE('',*,*,#14671,.T.);
#20523=ORIENTED_EDGE('',*,*,#14646,.T.);
#20524=ORIENTED_EDGE('',*,*,#14650,.T.);
#20525=ORIENTED_EDGE('',*,*,#14666,.T.);
#20526=ORIENTED_EDGE('',*,*,#14663,.T.);
#20527=ORIENTED_EDGE('',*,*,#14660,.T.);
#20528=ORIENTED_EDGE('',*,*,#14657,.T.);
#20529=ORIENTED_EDGE('',*,*,#14654,.T.);
#20530=ORIENTED_EDGE('',*,*,#14673,.F.);
#20531=ORIENTED_EDGE('',*,*,#14674,.T.);
#20532=ORIENTED_EDGE('',*,*,#14675,.T.);
#20533=ORIENTED_EDGE('',*,*,#14676,.T.);
#20534=ORIENTED_EDGE('',*,*,#14677,.T.);
#20535=ORIENTED_EDGE('',*,*,#14676,.F.);
#20536=ORIENTED_EDGE('',*,*,#14678,.T.);
#20537=ORIENTED_EDGE('',*,*,#14679,.T.);
#20538=ORIENTED_EDGE('',*,*,#14680,.F.);
#20539=ORIENTED_EDGE('',*,*,#14681,.T.);
#20540=ORIENTED_EDGE('',*,*,#14673,.T.);
#20541=ORIENTED_EDGE('',*,*,#14682,.T.);
#20542=ORIENTED_EDGE('',*,*,#14683,.F.);
#20543=ORIENTED_EDGE('',*,*,#14684,.T.);
#20544=ORIENTED_EDGE('',*,*,#14680,.T.);
#20545=ORIENTED_EDGE('',*,*,#14685,.T.);
#20546=ORIENTED_EDGE('',*,*,#14686,.F.);
#20547=ORIENTED_EDGE('',*,*,#14687,.T.);
#20548=ORIENTED_EDGE('',*,*,#14683,.T.);
#20549=ORIENTED_EDGE('',*,*,#14688,.T.);
#20550=ORIENTED_EDGE('',*,*,#14689,.F.);
#20551=ORIENTED_EDGE('',*,*,#14690,.T.);
#20552=ORIENTED_EDGE('',*,*,#14686,.T.);
#20553=ORIENTED_EDGE('',*,*,#14691,.T.);
#20554=ORIENTED_EDGE('',*,*,#14692,.F.);
#20555=ORIENTED_EDGE('',*,*,#14693,.T.);
#20556=ORIENTED_EDGE('',*,*,#14689,.T.);
#20557=ORIENTED_EDGE('',*,*,#14694,.T.);
#20558=ORIENTED_EDGE('',*,*,#14695,.F.);
#20559=ORIENTED_EDGE('',*,*,#14696,.T.);
#20560=ORIENTED_EDGE('',*,*,#14692,.T.);
#20561=ORIENTED_EDGE('',*,*,#14697,.T.);
#20562=ORIENTED_EDGE('',*,*,#14698,.F.);
#20563=ORIENTED_EDGE('',*,*,#14699,.T.);
#20564=ORIENTED_EDGE('',*,*,#14695,.T.);
#20565=ORIENTED_EDGE('',*,*,#14700,.T.);
#20566=ORIENTED_EDGE('',*,*,#14701,.F.);
#20567=ORIENTED_EDGE('',*,*,#14702,.T.);
#20568=ORIENTED_EDGE('',*,*,#14698,.T.);
#20569=ORIENTED_EDGE('',*,*,#14703,.T.);
#20570=ORIENTED_EDGE('',*,*,#14704,.F.);
#20571=ORIENTED_EDGE('',*,*,#14705,.T.);
#20572=ORIENTED_EDGE('',*,*,#14701,.T.);
#20573=ORIENTED_EDGE('',*,*,#14706,.T.);
#20574=ORIENTED_EDGE('',*,*,#14707,.F.);
#20575=ORIENTED_EDGE('',*,*,#14708,.T.);
#20576=ORIENTED_EDGE('',*,*,#14704,.T.);
#20577=ORIENTED_EDGE('',*,*,#14709,.T.);
#20578=ORIENTED_EDGE('',*,*,#14710,.F.);
#20579=ORIENTED_EDGE('',*,*,#14711,.T.);
#20580=ORIENTED_EDGE('',*,*,#14707,.T.);
#20581=ORIENTED_EDGE('',*,*,#14712,.T.);
#20582=ORIENTED_EDGE('',*,*,#14713,.F.);
#20583=ORIENTED_EDGE('',*,*,#14714,.T.);
#20584=ORIENTED_EDGE('',*,*,#14710,.T.);
#20585=ORIENTED_EDGE('',*,*,#14715,.T.);
#20586=ORIENTED_EDGE('',*,*,#14716,.F.);
#20587=ORIENTED_EDGE('',*,*,#14717,.T.);
#20588=ORIENTED_EDGE('',*,*,#14713,.T.);
#20589=ORIENTED_EDGE('',*,*,#14718,.T.);
#20590=ORIENTED_EDGE('',*,*,#14719,.F.);
#20591=ORIENTED_EDGE('',*,*,#14720,.T.);
#20592=ORIENTED_EDGE('',*,*,#14716,.T.);
#20593=ORIENTED_EDGE('',*,*,#14721,.T.);
#20594=ORIENTED_EDGE('',*,*,#14722,.F.);
#20595=ORIENTED_EDGE('',*,*,#14723,.T.);
#20596=ORIENTED_EDGE('',*,*,#14719,.T.);
#20597=ORIENTED_EDGE('',*,*,#14724,.T.);
#20598=ORIENTED_EDGE('',*,*,#14725,.F.);
#20599=ORIENTED_EDGE('',*,*,#14726,.T.);
#20600=ORIENTED_EDGE('',*,*,#14722,.T.);
#20601=ORIENTED_EDGE('',*,*,#14727,.T.);
#20602=ORIENTED_EDGE('',*,*,#14728,.F.);
#20603=ORIENTED_EDGE('',*,*,#14729,.T.);
#20604=ORIENTED_EDGE('',*,*,#14725,.T.);
#20605=ORIENTED_EDGE('',*,*,#14730,.T.);
#20606=ORIENTED_EDGE('',*,*,#14731,.F.);
#20607=ORIENTED_EDGE('',*,*,#14732,.T.);
#20608=ORIENTED_EDGE('',*,*,#14728,.T.);
#20609=ORIENTED_EDGE('',*,*,#14733,.T.);
#20610=ORIENTED_EDGE('',*,*,#14734,.F.);
#20611=ORIENTED_EDGE('',*,*,#14735,.T.);
#20612=ORIENTED_EDGE('',*,*,#14731,.T.);
#20613=ORIENTED_EDGE('',*,*,#14736,.T.);
#20614=ORIENTED_EDGE('',*,*,#14737,.F.);
#20615=ORIENTED_EDGE('',*,*,#14738,.T.);
#20616=ORIENTED_EDGE('',*,*,#14734,.T.);
#20617=ORIENTED_EDGE('',*,*,#14739,.T.);
#20618=ORIENTED_EDGE('',*,*,#14740,.F.);
#20619=ORIENTED_EDGE('',*,*,#14741,.T.);
#20620=ORIENTED_EDGE('',*,*,#14737,.T.);
#20621=ORIENTED_EDGE('',*,*,#14742,.T.);
#20622=ORIENTED_EDGE('',*,*,#14743,.F.);
#20623=ORIENTED_EDGE('',*,*,#14744,.T.);
#20624=ORIENTED_EDGE('',*,*,#14740,.T.);
#20625=ORIENTED_EDGE('',*,*,#14745,.T.);
#20626=ORIENTED_EDGE('',*,*,#14746,.F.);
#20627=ORIENTED_EDGE('',*,*,#14747,.T.);
#20628=ORIENTED_EDGE('',*,*,#14748,.F.);
#20629=ORIENTED_EDGE('',*,*,#14749,.F.);
#20630=ORIENTED_EDGE('',*,*,#14750,.F.);
#20631=ORIENTED_EDGE('',*,*,#14751,.T.);
#20632=ORIENTED_EDGE('',*,*,#14746,.T.);
#20633=ORIENTED_EDGE('',*,*,#14752,.F.);
#20634=ORIENTED_EDGE('',*,*,#14753,.F.);
#20635=ORIENTED_EDGE('',*,*,#14754,.T.);
#20636=ORIENTED_EDGE('',*,*,#14750,.T.);
#20637=ORIENTED_EDGE('',*,*,#14755,.F.);
#20638=ORIENTED_EDGE('',*,*,#14756,.F.);
#20639=ORIENTED_EDGE('',*,*,#14757,.T.);
#20640=ORIENTED_EDGE('',*,*,#14753,.T.);
#20641=ORIENTED_EDGE('',*,*,#14758,.F.);
#20642=ORIENTED_EDGE('',*,*,#14759,.F.);
#20643=ORIENTED_EDGE('',*,*,#14760,.T.);
#20644=ORIENTED_EDGE('',*,*,#14756,.T.);
#20645=ORIENTED_EDGE('',*,*,#14761,.F.);
#20646=ORIENTED_EDGE('',*,*,#14762,.F.);
#20647=ORIENTED_EDGE('',*,*,#14763,.T.);
#20648=ORIENTED_EDGE('',*,*,#14759,.T.);
#20649=ORIENTED_EDGE('',*,*,#14764,.F.);
#20650=ORIENTED_EDGE('',*,*,#14765,.F.);
#20651=ORIENTED_EDGE('',*,*,#14766,.T.);
#20652=ORIENTED_EDGE('',*,*,#14762,.T.);
#20653=ORIENTED_EDGE('',*,*,#14767,.F.);
#20654=ORIENTED_EDGE('',*,*,#14768,.F.);
#20655=ORIENTED_EDGE('',*,*,#14769,.T.);
#20656=ORIENTED_EDGE('',*,*,#14765,.T.);
#20657=ORIENTED_EDGE('',*,*,#14770,.F.);
#20658=ORIENTED_EDGE('',*,*,#14771,.F.);
#20659=ORIENTED_EDGE('',*,*,#14772,.T.);
#20660=ORIENTED_EDGE('',*,*,#14768,.T.);
#20661=ORIENTED_EDGE('',*,*,#14773,.F.);
#20662=ORIENTED_EDGE('',*,*,#14774,.F.);
#20663=ORIENTED_EDGE('',*,*,#14775,.T.);
#20664=ORIENTED_EDGE('',*,*,#14771,.T.);
#20665=ORIENTED_EDGE('',*,*,#14776,.F.);
#20666=ORIENTED_EDGE('',*,*,#14777,.F.);
#20667=ORIENTED_EDGE('',*,*,#14778,.T.);
#20668=ORIENTED_EDGE('',*,*,#14774,.T.);
#20669=ORIENTED_EDGE('',*,*,#14779,.F.);
#20670=ORIENTED_EDGE('',*,*,#14780,.F.);
#20671=ORIENTED_EDGE('',*,*,#14781,.T.);
#20672=ORIENTED_EDGE('',*,*,#14777,.T.);
#20673=ORIENTED_EDGE('',*,*,#14782,.F.);
#20674=ORIENTED_EDGE('',*,*,#14783,.F.);
#20675=ORIENTED_EDGE('',*,*,#14784,.T.);
#20676=ORIENTED_EDGE('',*,*,#14780,.T.);
#20677=ORIENTED_EDGE('',*,*,#14785,.F.);
#20678=ORIENTED_EDGE('',*,*,#14786,.F.);
#20679=ORIENTED_EDGE('',*,*,#14787,.T.);
#20680=ORIENTED_EDGE('',*,*,#14783,.T.);
#20681=ORIENTED_EDGE('',*,*,#14788,.F.);
#20682=ORIENTED_EDGE('',*,*,#14789,.F.);
#20683=ORIENTED_EDGE('',*,*,#14790,.T.);
#20684=ORIENTED_EDGE('',*,*,#14786,.T.);
#20685=ORIENTED_EDGE('',*,*,#14791,.F.);
#20686=ORIENTED_EDGE('',*,*,#14792,.F.);
#20687=ORIENTED_EDGE('',*,*,#14793,.T.);
#20688=ORIENTED_EDGE('',*,*,#14789,.T.);
#20689=ORIENTED_EDGE('',*,*,#14794,.F.);
#20690=ORIENTED_EDGE('',*,*,#14795,.F.);
#20691=ORIENTED_EDGE('',*,*,#14796,.T.);
#20692=ORIENTED_EDGE('',*,*,#14792,.T.);
#20693=ORIENTED_EDGE('',*,*,#14797,.F.);
#20694=ORIENTED_EDGE('',*,*,#14798,.F.);
#20695=ORIENTED_EDGE('',*,*,#14799,.T.);
#20696=ORIENTED_EDGE('',*,*,#14795,.T.);
#20697=ORIENTED_EDGE('',*,*,#14800,.F.);
#20698=ORIENTED_EDGE('',*,*,#14801,.F.);
#20699=ORIENTED_EDGE('',*,*,#14802,.T.);
#20700=ORIENTED_EDGE('',*,*,#14798,.T.);
#20701=ORIENTED_EDGE('',*,*,#14803,.F.);
#20702=ORIENTED_EDGE('',*,*,#14804,.F.);
#20703=ORIENTED_EDGE('',*,*,#14805,.T.);
#20704=ORIENTED_EDGE('',*,*,#14801,.T.);
#20705=ORIENTED_EDGE('',*,*,#14806,.F.);
#20706=ORIENTED_EDGE('',*,*,#14807,.F.);
#20707=ORIENTED_EDGE('',*,*,#14808,.T.);
#20708=ORIENTED_EDGE('',*,*,#14804,.T.);
#20709=ORIENTED_EDGE('',*,*,#14809,.F.);
#20710=ORIENTED_EDGE('',*,*,#14810,.F.);
#20711=ORIENTED_EDGE('',*,*,#14811,.T.);
#20712=ORIENTED_EDGE('',*,*,#14807,.T.);
#20713=ORIENTED_EDGE('',*,*,#14812,.F.);
#20714=ORIENTED_EDGE('',*,*,#14813,.F.);
#20715=ORIENTED_EDGE('',*,*,#14814,.T.);
#20716=ORIENTED_EDGE('',*,*,#14810,.T.);
#20717=ORIENTED_EDGE('',*,*,#14815,.F.);
#20718=ORIENTED_EDGE('',*,*,#14816,.F.);
#20719=ORIENTED_EDGE('',*,*,#14817,.F.);
#20720=ORIENTED_EDGE('',*,*,#14818,.T.);
#20721=ORIENTED_EDGE('',*,*,#14813,.T.);
#20722=ORIENTED_EDGE('',*,*,#14819,.F.);
#20723=ORIENTED_EDGE('',*,*,#14748,.T.);
#20724=ORIENTED_EDGE('',*,*,#14820,.T.);
#20725=ORIENTED_EDGE('',*,*,#14821,.F.);
#20726=ORIENTED_EDGE('',*,*,#14822,.F.);
#20727=ORIENTED_EDGE('',*,*,#14823,.T.);
#20728=ORIENTED_EDGE('',*,*,#14823,.F.);
#20729=ORIENTED_EDGE('',*,*,#14824,.F.);
#20730=ORIENTED_EDGE('',*,*,#14745,.F.);
#20731=ORIENTED_EDGE('',*,*,#14742,.F.);
#20732=ORIENTED_EDGE('',*,*,#14739,.F.);
#20733=ORIENTED_EDGE('',*,*,#14736,.F.);
#20734=ORIENTED_EDGE('',*,*,#14733,.F.);
#20735=ORIENTED_EDGE('',*,*,#14730,.F.);
#20736=ORIENTED_EDGE('',*,*,#14727,.F.);
#20737=ORIENTED_EDGE('',*,*,#14724,.F.);
#20738=ORIENTED_EDGE('',*,*,#14721,.F.);
#20739=ORIENTED_EDGE('',*,*,#14718,.F.);
#20740=ORIENTED_EDGE('',*,*,#14715,.F.);
#20741=ORIENTED_EDGE('',*,*,#14712,.F.);
#20742=ORIENTED_EDGE('',*,*,#14709,.F.);
#20743=ORIENTED_EDGE('',*,*,#14706,.F.);
#20744=ORIENTED_EDGE('',*,*,#14703,.F.);
#20745=ORIENTED_EDGE('',*,*,#14700,.F.);
#20746=ORIENTED_EDGE('',*,*,#14697,.F.);
#20747=ORIENTED_EDGE('',*,*,#14694,.F.);
#20748=ORIENTED_EDGE('',*,*,#14691,.F.);
#20749=ORIENTED_EDGE('',*,*,#14688,.F.);
#20750=ORIENTED_EDGE('',*,*,#14685,.F.);
#20751=ORIENTED_EDGE('',*,*,#14682,.F.);
#20752=ORIENTED_EDGE('',*,*,#14679,.F.);
#20753=ORIENTED_EDGE('',*,*,#14825,.F.);
#20754=ORIENTED_EDGE('',*,*,#14826,.T.);
#20755=ORIENTED_EDGE('',*,*,#14819,.T.);
#20756=ORIENTED_EDGE('',*,*,#14815,.T.);
#20757=ORIENTED_EDGE('',*,*,#14812,.T.);
#20758=ORIENTED_EDGE('',*,*,#14809,.T.);
#20759=ORIENTED_EDGE('',*,*,#14806,.T.);
#20760=ORIENTED_EDGE('',*,*,#14803,.T.);
#20761=ORIENTED_EDGE('',*,*,#14800,.T.);
#20762=ORIENTED_EDGE('',*,*,#14797,.T.);
#20763=ORIENTED_EDGE('',*,*,#14794,.T.);
#20764=ORIENTED_EDGE('',*,*,#14791,.T.);
#20765=ORIENTED_EDGE('',*,*,#14788,.T.);
#20766=ORIENTED_EDGE('',*,*,#14785,.T.);
#20767=ORIENTED_EDGE('',*,*,#14782,.T.);
#20768=ORIENTED_EDGE('',*,*,#14779,.T.);
#20769=ORIENTED_EDGE('',*,*,#14776,.T.);
#20770=ORIENTED_EDGE('',*,*,#14773,.T.);
#20771=ORIENTED_EDGE('',*,*,#14770,.T.);
#20772=ORIENTED_EDGE('',*,*,#14767,.T.);
#20773=ORIENTED_EDGE('',*,*,#14764,.T.);
#20774=ORIENTED_EDGE('',*,*,#14761,.T.);
#20775=ORIENTED_EDGE('',*,*,#14758,.T.);
#20776=ORIENTED_EDGE('',*,*,#14755,.T.);
#20777=ORIENTED_EDGE('',*,*,#14752,.T.);
#20778=ORIENTED_EDGE('',*,*,#14749,.T.);
#20779=ORIENTED_EDGE('',*,*,#14675,.F.);
#20780=ORIENTED_EDGE('',*,*,#14827,.T.);
#20781=ORIENTED_EDGE('',*,*,#14817,.T.);
#20782=ORIENTED_EDGE('',*,*,#14828,.T.);
#20783=ORIENTED_EDGE('',*,*,#14825,.T.);
#20784=ORIENTED_EDGE('',*,*,#14678,.F.);
#20785=ORIENTED_EDGE('',*,*,#14816,.T.);
#20786=ORIENTED_EDGE('',*,*,#14826,.F.);
#20787=ORIENTED_EDGE('',*,*,#14828,.F.);
#20788=ORIENTED_EDGE('',*,*,#14820,.F.);
#20789=ORIENTED_EDGE('',*,*,#14747,.F.);
#20790=ORIENTED_EDGE('',*,*,#14751,.F.);
#20791=ORIENTED_EDGE('',*,*,#14754,.F.);
#20792=ORIENTED_EDGE('',*,*,#14757,.F.);
#20793=ORIENTED_EDGE('',*,*,#14760,.F.);
#20794=ORIENTED_EDGE('',*,*,#14763,.F.);
#20795=ORIENTED_EDGE('',*,*,#14766,.F.);
#20796=ORIENTED_EDGE('',*,*,#14769,.F.);
#20797=ORIENTED_EDGE('',*,*,#14772,.F.);
#20798=ORIENTED_EDGE('',*,*,#14775,.F.);
#20799=ORIENTED_EDGE('',*,*,#14778,.F.);
#20800=ORIENTED_EDGE('',*,*,#14781,.F.);
#20801=ORIENTED_EDGE('',*,*,#14784,.F.);
#20802=ORIENTED_EDGE('',*,*,#14787,.F.);
#20803=ORIENTED_EDGE('',*,*,#14790,.F.);
#20804=ORIENTED_EDGE('',*,*,#14793,.F.);
#20805=ORIENTED_EDGE('',*,*,#14796,.F.);
#20806=ORIENTED_EDGE('',*,*,#14799,.F.);
#20807=ORIENTED_EDGE('',*,*,#14802,.F.);
#20808=ORIENTED_EDGE('',*,*,#14805,.F.);
#20809=ORIENTED_EDGE('',*,*,#14808,.F.);
#20810=ORIENTED_EDGE('',*,*,#14811,.F.);
#20811=ORIENTED_EDGE('',*,*,#14814,.F.);
#20812=ORIENTED_EDGE('',*,*,#14818,.F.);
#20813=ORIENTED_EDGE('',*,*,#14827,.F.);
#20814=ORIENTED_EDGE('',*,*,#14674,.F.);
#20815=ORIENTED_EDGE('',*,*,#14681,.F.);
#20816=ORIENTED_EDGE('',*,*,#14684,.F.);
#20817=ORIENTED_EDGE('',*,*,#14687,.F.);
#20818=ORIENTED_EDGE('',*,*,#14690,.F.);
#20819=ORIENTED_EDGE('',*,*,#14693,.F.);
#20820=ORIENTED_EDGE('',*,*,#14696,.F.);
#20821=ORIENTED_EDGE('',*,*,#14699,.F.);
#20822=ORIENTED_EDGE('',*,*,#14702,.F.);
#20823=ORIENTED_EDGE('',*,*,#14705,.F.);
#20824=ORIENTED_EDGE('',*,*,#14708,.F.);
#20825=ORIENTED_EDGE('',*,*,#14711,.F.);
#20826=ORIENTED_EDGE('',*,*,#14714,.F.);
#20827=ORIENTED_EDGE('',*,*,#14717,.F.);
#20828=ORIENTED_EDGE('',*,*,#14720,.F.);
#20829=ORIENTED_EDGE('',*,*,#14723,.F.);
#20830=ORIENTED_EDGE('',*,*,#14726,.F.);
#20831=ORIENTED_EDGE('',*,*,#14729,.F.);
#20832=ORIENTED_EDGE('',*,*,#14732,.F.);
#20833=ORIENTED_EDGE('',*,*,#14735,.F.);
#20834=ORIENTED_EDGE('',*,*,#14738,.F.);
#20835=ORIENTED_EDGE('',*,*,#14741,.F.);
#20836=ORIENTED_EDGE('',*,*,#14744,.F.);
#20837=ORIENTED_EDGE('',*,*,#14829,.F.);
#20838=ORIENTED_EDGE('',*,*,#14830,.F.);
#20839=ORIENTED_EDGE('',*,*,#14831,.T.);
#20840=ORIENTED_EDGE('',*,*,#14832,.T.);
#20841=ORIENTED_EDGE('',*,*,#14833,.F.);
#20842=ORIENTED_EDGE('',*,*,#14832,.F.);
#20843=ORIENTED_EDGE('',*,*,#14834,.T.);
#20844=ORIENTED_EDGE('',*,*,#14835,.F.);
#20845=ORIENTED_EDGE('',*,*,#14836,.F.);
#20846=ORIENTED_EDGE('',*,*,#14837,.F.);
#20847=ORIENTED_EDGE('',*,*,#14834,.F.);
#20848=ORIENTED_EDGE('',*,*,#14831,.F.);
#20849=ORIENTED_EDGE('',*,*,#14838,.F.);
#20850=ORIENTED_EDGE('',*,*,#14839,.T.);
#20851=ORIENTED_EDGE('',*,*,#14840,.T.);
#20852=ORIENTED_EDGE('',*,*,#14841,.F.);
#20853=ORIENTED_EDGE('',*,*,#14840,.F.);
#20854=ORIENTED_EDGE('',*,*,#14842,.T.);
#20855=ORIENTED_EDGE('',*,*,#14843,.F.);
#20856=ORIENTED_EDGE('',*,*,#14844,.F.);
#20857=ORIENTED_EDGE('',*,*,#14845,.F.);
#20858=ORIENTED_EDGE('',*,*,#14842,.F.);
#20859=ORIENTED_EDGE('',*,*,#14839,.F.);
#20860=ORIENTED_EDGE('',*,*,#14846,.F.);
#20861=ORIENTED_EDGE('',*,*,#14847,.T.);
#20862=ORIENTED_EDGE('',*,*,#14848,.T.);
#20863=ORIENTED_EDGE('',*,*,#14849,.F.);
#20864=ORIENTED_EDGE('',*,*,#14848,.F.);
#20865=ORIENTED_EDGE('',*,*,#14850,.T.);
#20866=ORIENTED_EDGE('',*,*,#14851,.F.);
#20867=ORIENTED_EDGE('',*,*,#14852,.F.);
#20868=ORIENTED_EDGE('',*,*,#14853,.F.);
#20869=ORIENTED_EDGE('',*,*,#14850,.F.);
#20870=ORIENTED_EDGE('',*,*,#14847,.F.);
#20871=ORIENTED_EDGE('',*,*,#14854,.F.);
#20872=ORIENTED_EDGE('',*,*,#14855,.T.);
#20873=ORIENTED_EDGE('',*,*,#14856,.T.);
#20874=ORIENTED_EDGE('',*,*,#14857,.F.);
#20875=ORIENTED_EDGE('',*,*,#14856,.F.);
#20876=ORIENTED_EDGE('',*,*,#14858,.T.);
#20877=ORIENTED_EDGE('',*,*,#14859,.F.);
#20878=ORIENTED_EDGE('',*,*,#14860,.F.);
#20879=ORIENTED_EDGE('',*,*,#14861,.F.);
#20880=ORIENTED_EDGE('',*,*,#14858,.F.);
#20881=ORIENTED_EDGE('',*,*,#14855,.F.);
#20882=ORIENTED_EDGE('',*,*,#14862,.F.);
#20883=ORIENTED_EDGE('',*,*,#14863,.T.);
#20884=ORIENTED_EDGE('',*,*,#14864,.T.);
#20885=ORIENTED_EDGE('',*,*,#14865,.F.);
#20886=ORIENTED_EDGE('',*,*,#14864,.F.);
#20887=ORIENTED_EDGE('',*,*,#14866,.T.);
#20888=ORIENTED_EDGE('',*,*,#14867,.F.);
#20889=ORIENTED_EDGE('',*,*,#14868,.F.);
#20890=ORIENTED_EDGE('',*,*,#14869,.F.);
#20891=ORIENTED_EDGE('',*,*,#14866,.F.);
#20892=ORIENTED_EDGE('',*,*,#14863,.F.);
#20893=ORIENTED_EDGE('',*,*,#14870,.F.);
#20894=ORIENTED_EDGE('',*,*,#14871,.T.);
#20895=ORIENTED_EDGE('',*,*,#14872,.T.);
#20896=ORIENTED_EDGE('',*,*,#14873,.F.);
#20897=ORIENTED_EDGE('',*,*,#14872,.F.);
#20898=ORIENTED_EDGE('',*,*,#14874,.T.);
#20899=ORIENTED_EDGE('',*,*,#14875,.F.);
#20900=ORIENTED_EDGE('',*,*,#14876,.F.);
#20901=ORIENTED_EDGE('',*,*,#14877,.F.);
#20902=ORIENTED_EDGE('',*,*,#14874,.F.);
#20903=ORIENTED_EDGE('',*,*,#14871,.F.);
#20904=ORIENTED_EDGE('',*,*,#14878,.F.);
#20905=ORIENTED_EDGE('',*,*,#14879,.T.);
#20906=ORIENTED_EDGE('',*,*,#14880,.T.);
#20907=ORIENTED_EDGE('',*,*,#14881,.F.);
#20908=ORIENTED_EDGE('',*,*,#14880,.F.);
#20909=ORIENTED_EDGE('',*,*,#14882,.T.);
#20910=ORIENTED_EDGE('',*,*,#14883,.F.);
#20911=ORIENTED_EDGE('',*,*,#14884,.F.);
#20912=ORIENTED_EDGE('',*,*,#14885,.F.);
#20913=ORIENTED_EDGE('',*,*,#14882,.F.);
#20914=ORIENTED_EDGE('',*,*,#14879,.F.);
#20915=ORIENTED_EDGE('',*,*,#14886,.F.);
#20916=ORIENTED_EDGE('',*,*,#14887,.T.);
#20917=ORIENTED_EDGE('',*,*,#14888,.T.);
#20918=ORIENTED_EDGE('',*,*,#14889,.F.);
#20919=ORIENTED_EDGE('',*,*,#14888,.F.);
#20920=ORIENTED_EDGE('',*,*,#14890,.T.);
#20921=ORIENTED_EDGE('',*,*,#14891,.F.);
#20922=ORIENTED_EDGE('',*,*,#14892,.F.);
#20923=ORIENTED_EDGE('',*,*,#14893,.F.);
#20924=ORIENTED_EDGE('',*,*,#14890,.F.);
#20925=ORIENTED_EDGE('',*,*,#14887,.F.);
#20926=ORIENTED_EDGE('',*,*,#14894,.F.);
#20927=ORIENTED_EDGE('',*,*,#14895,.T.);
#20928=ORIENTED_EDGE('',*,*,#14896,.T.);
#20929=ORIENTED_EDGE('',*,*,#14897,.F.);
#20930=ORIENTED_EDGE('',*,*,#14896,.F.);
#20931=ORIENTED_EDGE('',*,*,#14898,.T.);
#20932=ORIENTED_EDGE('',*,*,#14899,.F.);
#20933=ORIENTED_EDGE('',*,*,#14900,.F.);
#20934=ORIENTED_EDGE('',*,*,#14901,.F.);
#20935=ORIENTED_EDGE('',*,*,#14898,.F.);
#20936=ORIENTED_EDGE('',*,*,#14895,.F.);
#20937=ORIENTED_EDGE('',*,*,#14902,.F.);
#20938=ORIENTED_EDGE('',*,*,#14903,.T.);
#20939=ORIENTED_EDGE('',*,*,#14904,.T.);
#20940=ORIENTED_EDGE('',*,*,#14905,.F.);
#20941=ORIENTED_EDGE('',*,*,#14904,.F.);
#20942=ORIENTED_EDGE('',*,*,#14906,.T.);
#20943=ORIENTED_EDGE('',*,*,#14907,.F.);
#20944=ORIENTED_EDGE('',*,*,#14908,.F.);
#20945=ORIENTED_EDGE('',*,*,#14909,.F.);
#20946=ORIENTED_EDGE('',*,*,#14906,.F.);
#20947=ORIENTED_EDGE('',*,*,#14903,.F.);
#20948=ORIENTED_EDGE('',*,*,#14910,.F.);
#20949=ORIENTED_EDGE('',*,*,#14911,.T.);
#20950=ORIENTED_EDGE('',*,*,#14912,.T.);
#20951=ORIENTED_EDGE('',*,*,#14913,.F.);
#20952=ORIENTED_EDGE('',*,*,#14912,.F.);
#20953=ORIENTED_EDGE('',*,*,#14914,.T.);
#20954=ORIENTED_EDGE('',*,*,#14915,.F.);
#20955=ORIENTED_EDGE('',*,*,#14916,.F.);
#20956=ORIENTED_EDGE('',*,*,#14917,.F.);
#20957=ORIENTED_EDGE('',*,*,#14914,.F.);
#20958=ORIENTED_EDGE('',*,*,#14911,.F.);
#20959=ORIENTED_EDGE('',*,*,#14918,.F.);
#20960=ORIENTED_EDGE('',*,*,#14919,.T.);
#20961=ORIENTED_EDGE('',*,*,#14920,.T.);
#20962=ORIENTED_EDGE('',*,*,#14921,.F.);
#20963=ORIENTED_EDGE('',*,*,#14920,.F.);
#20964=ORIENTED_EDGE('',*,*,#14922,.T.);
#20965=ORIENTED_EDGE('',*,*,#14923,.F.);
#20966=ORIENTED_EDGE('',*,*,#14924,.F.);
#20967=ORIENTED_EDGE('',*,*,#14925,.F.);
#20968=ORIENTED_EDGE('',*,*,#14922,.F.);
#20969=ORIENTED_EDGE('',*,*,#14919,.F.);
#20970=ORIENTED_EDGE('',*,*,#14926,.F.);
#20971=ORIENTED_EDGE('',*,*,#14927,.T.);
#20972=ORIENTED_EDGE('',*,*,#14928,.T.);
#20973=ORIENTED_EDGE('',*,*,#14929,.F.);
#20974=ORIENTED_EDGE('',*,*,#14928,.F.);
#20975=ORIENTED_EDGE('',*,*,#14930,.T.);
#20976=ORIENTED_EDGE('',*,*,#14931,.F.);
#20977=ORIENTED_EDGE('',*,*,#14932,.F.);
#20978=ORIENTED_EDGE('',*,*,#14933,.F.);
#20979=ORIENTED_EDGE('',*,*,#14930,.F.);
#20980=ORIENTED_EDGE('',*,*,#14927,.F.);
#20981=ORIENTED_EDGE('',*,*,#14934,.F.);
#20982=ORIENTED_EDGE('',*,*,#14935,.T.);
#20983=ORIENTED_EDGE('',*,*,#14936,.T.);
#20984=ORIENTED_EDGE('',*,*,#14937,.F.);
#20985=ORIENTED_EDGE('',*,*,#14936,.F.);
#20986=ORIENTED_EDGE('',*,*,#14938,.T.);
#20987=ORIENTED_EDGE('',*,*,#14939,.F.);
#20988=ORIENTED_EDGE('',*,*,#14940,.F.);
#20989=ORIENTED_EDGE('',*,*,#14941,.F.);
#20990=ORIENTED_EDGE('',*,*,#14938,.F.);
#20991=ORIENTED_EDGE('',*,*,#14935,.F.);
#20992=ORIENTED_EDGE('',*,*,#14942,.F.);
#20993=ORIENTED_EDGE('',*,*,#14943,.T.);
#20994=ORIENTED_EDGE('',*,*,#14944,.T.);
#20995=ORIENTED_EDGE('',*,*,#14945,.F.);
#20996=ORIENTED_EDGE('',*,*,#14944,.F.);
#20997=ORIENTED_EDGE('',*,*,#14946,.T.);
#20998=ORIENTED_EDGE('',*,*,#14947,.F.);
#20999=ORIENTED_EDGE('',*,*,#14948,.F.);
#21000=ORIENTED_EDGE('',*,*,#14949,.F.);
#21001=ORIENTED_EDGE('',*,*,#14946,.F.);
#21002=ORIENTED_EDGE('',*,*,#14943,.F.);
#21003=ORIENTED_EDGE('',*,*,#14950,.F.);
#21004=ORIENTED_EDGE('',*,*,#14951,.T.);
#21005=ORIENTED_EDGE('',*,*,#14952,.T.);
#21006=ORIENTED_EDGE('',*,*,#14953,.F.);
#21007=ORIENTED_EDGE('',*,*,#14952,.F.);
#21008=ORIENTED_EDGE('',*,*,#14954,.T.);
#21009=ORIENTED_EDGE('',*,*,#14955,.F.);
#21010=ORIENTED_EDGE('',*,*,#14956,.F.);
#21011=ORIENTED_EDGE('',*,*,#14957,.F.);
#21012=ORIENTED_EDGE('',*,*,#14954,.F.);
#21013=ORIENTED_EDGE('',*,*,#14951,.F.);
#21014=ORIENTED_EDGE('',*,*,#14958,.F.);
#21015=ORIENTED_EDGE('',*,*,#14959,.T.);
#21016=ORIENTED_EDGE('',*,*,#14960,.T.);
#21017=ORIENTED_EDGE('',*,*,#14961,.F.);
#21018=ORIENTED_EDGE('',*,*,#14960,.F.);
#21019=ORIENTED_EDGE('',*,*,#14962,.T.);
#21020=ORIENTED_EDGE('',*,*,#14963,.F.);
#21021=ORIENTED_EDGE('',*,*,#14964,.F.);
#21022=ORIENTED_EDGE('',*,*,#14965,.F.);
#21023=ORIENTED_EDGE('',*,*,#14962,.F.);
#21024=ORIENTED_EDGE('',*,*,#14959,.F.);
#21025=ORIENTED_EDGE('',*,*,#14966,.F.);
#21026=ORIENTED_EDGE('',*,*,#14967,.T.);
#21027=ORIENTED_EDGE('',*,*,#14968,.T.);
#21028=ORIENTED_EDGE('',*,*,#14969,.F.);
#21029=ORIENTED_EDGE('',*,*,#14970,.F.);
#21030=ORIENTED_EDGE('',*,*,#14968,.F.);
#21031=ORIENTED_EDGE('',*,*,#14971,.T.);
#21032=ORIENTED_EDGE('',*,*,#14972,.F.);
#21033=ORIENTED_EDGE('',*,*,#14973,.F.);
#21034=ORIENTED_EDGE('',*,*,#14974,.F.);
#21035=ORIENTED_EDGE('',*,*,#14971,.F.);
#21036=ORIENTED_EDGE('',*,*,#14967,.F.);
#21037=ORIENTED_EDGE('',*,*,#14975,.F.);
#21038=ORIENTED_EDGE('',*,*,#14976,.T.);
#21039=ORIENTED_EDGE('',*,*,#14977,.T.);
#21040=ORIENTED_EDGE('',*,*,#14978,.F.);
#21041=ORIENTED_EDGE('',*,*,#14977,.F.);
#21042=ORIENTED_EDGE('',*,*,#14979,.T.);
#21043=ORIENTED_EDGE('',*,*,#14980,.F.);
#21044=ORIENTED_EDGE('',*,*,#14981,.F.);
#21045=ORIENTED_EDGE('',*,*,#14982,.F.);
#21046=ORIENTED_EDGE('',*,*,#14979,.F.);
#21047=ORIENTED_EDGE('',*,*,#14976,.F.);
#21048=ORIENTED_EDGE('',*,*,#14983,.F.);
#21049=ORIENTED_EDGE('',*,*,#14984,.T.);
#21050=ORIENTED_EDGE('',*,*,#14985,.T.);
#21051=ORIENTED_EDGE('',*,*,#14986,.F.);
#21052=ORIENTED_EDGE('',*,*,#14985,.F.);
#21053=ORIENTED_EDGE('',*,*,#14987,.T.);
#21054=ORIENTED_EDGE('',*,*,#14988,.F.);
#21055=ORIENTED_EDGE('',*,*,#14989,.F.);
#21056=ORIENTED_EDGE('',*,*,#14990,.F.);
#21057=ORIENTED_EDGE('',*,*,#14987,.F.);
#21058=ORIENTED_EDGE('',*,*,#14984,.F.);
#21059=ORIENTED_EDGE('',*,*,#14991,.F.);
#21060=ORIENTED_EDGE('',*,*,#14992,.T.);
#21061=ORIENTED_EDGE('',*,*,#14993,.T.);
#21062=ORIENTED_EDGE('',*,*,#14994,.F.);
#21063=ORIENTED_EDGE('',*,*,#14993,.F.);
#21064=ORIENTED_EDGE('',*,*,#14995,.T.);
#21065=ORIENTED_EDGE('',*,*,#14996,.F.);
#21066=ORIENTED_EDGE('',*,*,#14997,.F.);
#21067=ORIENTED_EDGE('',*,*,#14998,.F.);
#21068=ORIENTED_EDGE('',*,*,#14995,.F.);
#21069=ORIENTED_EDGE('',*,*,#14992,.F.);
#21070=ORIENTED_EDGE('',*,*,#14999,.F.);
#21071=ORIENTED_EDGE('',*,*,#15000,.T.);
#21072=ORIENTED_EDGE('',*,*,#15001,.T.);
#21073=ORIENTED_EDGE('',*,*,#15002,.F.);
#21074=ORIENTED_EDGE('',*,*,#15001,.F.);
#21075=ORIENTED_EDGE('',*,*,#15003,.T.);
#21076=ORIENTED_EDGE('',*,*,#15004,.F.);
#21077=ORIENTED_EDGE('',*,*,#15005,.F.);
#21078=ORIENTED_EDGE('',*,*,#15006,.F.);
#21079=ORIENTED_EDGE('',*,*,#15003,.F.);
#21080=ORIENTED_EDGE('',*,*,#15000,.F.);
#21081=ORIENTED_EDGE('',*,*,#15007,.F.);
#21082=ORIENTED_EDGE('',*,*,#15008,.T.);
#21083=ORIENTED_EDGE('',*,*,#15009,.T.);
#21084=ORIENTED_EDGE('',*,*,#15010,.F.);
#21085=ORIENTED_EDGE('',*,*,#15009,.F.);
#21086=ORIENTED_EDGE('',*,*,#15011,.T.);
#21087=ORIENTED_EDGE('',*,*,#15012,.F.);
#21088=ORIENTED_EDGE('',*,*,#15013,.F.);
#21089=ORIENTED_EDGE('',*,*,#15014,.F.);
#21090=ORIENTED_EDGE('',*,*,#15011,.F.);
#21091=ORIENTED_EDGE('',*,*,#15008,.F.);
#21092=ORIENTED_EDGE('',*,*,#15015,.F.);
#21093=ORIENTED_EDGE('',*,*,#15016,.T.);
#21094=ORIENTED_EDGE('',*,*,#15017,.T.);
#21095=ORIENTED_EDGE('',*,*,#15018,.F.);
#21096=ORIENTED_EDGE('',*,*,#15017,.F.);
#21097=ORIENTED_EDGE('',*,*,#15019,.T.);
#21098=ORIENTED_EDGE('',*,*,#15020,.F.);
#21099=ORIENTED_EDGE('',*,*,#15021,.F.);
#21100=ORIENTED_EDGE('',*,*,#15022,.F.);
#21101=ORIENTED_EDGE('',*,*,#15019,.F.);
#21102=ORIENTED_EDGE('',*,*,#15016,.F.);
#21103=ORIENTED_EDGE('',*,*,#15023,.F.);
#21104=ORIENTED_EDGE('',*,*,#15024,.T.);
#21105=ORIENTED_EDGE('',*,*,#15025,.T.);
#21106=ORIENTED_EDGE('',*,*,#15026,.F.);
#21107=ORIENTED_EDGE('',*,*,#15025,.F.);
#21108=ORIENTED_EDGE('',*,*,#15027,.T.);
#21109=ORIENTED_EDGE('',*,*,#15028,.F.);
#21110=ORIENTED_EDGE('',*,*,#15029,.F.);
#21111=ORIENTED_EDGE('',*,*,#15030,.F.);
#21112=ORIENTED_EDGE('',*,*,#15027,.F.);
#21113=ORIENTED_EDGE('',*,*,#15024,.F.);
#21114=ORIENTED_EDGE('',*,*,#15031,.F.);
#21115=ORIENTED_EDGE('',*,*,#15032,.T.);
#21116=ORIENTED_EDGE('',*,*,#15033,.T.);
#21117=ORIENTED_EDGE('',*,*,#15034,.F.);
#21118=ORIENTED_EDGE('',*,*,#15033,.F.);
#21119=ORIENTED_EDGE('',*,*,#15035,.T.);
#21120=ORIENTED_EDGE('',*,*,#15036,.F.);
#21121=ORIENTED_EDGE('',*,*,#15037,.F.);
#21122=ORIENTED_EDGE('',*,*,#15038,.F.);
#21123=ORIENTED_EDGE('',*,*,#15035,.F.);
#21124=ORIENTED_EDGE('',*,*,#15032,.F.);
#21125=ORIENTED_EDGE('',*,*,#15039,.F.);
#21126=ORIENTED_EDGE('',*,*,#15040,.T.);
#21127=ORIENTED_EDGE('',*,*,#15041,.T.);
#21128=ORIENTED_EDGE('',*,*,#15042,.F.);
#21129=ORIENTED_EDGE('',*,*,#15041,.F.);
#21130=ORIENTED_EDGE('',*,*,#15043,.T.);
#21131=ORIENTED_EDGE('',*,*,#15044,.F.);
#21132=ORIENTED_EDGE('',*,*,#15045,.F.);
#21133=ORIENTED_EDGE('',*,*,#15046,.F.);
#21134=ORIENTED_EDGE('',*,*,#15043,.F.);
#21135=ORIENTED_EDGE('',*,*,#15040,.F.);
#21136=ORIENTED_EDGE('',*,*,#15047,.F.);
#21137=ORIENTED_EDGE('',*,*,#15048,.T.);
#21138=ORIENTED_EDGE('',*,*,#15049,.T.);
#21139=ORIENTED_EDGE('',*,*,#15050,.F.);
#21140=ORIENTED_EDGE('',*,*,#15049,.F.);
#21141=ORIENTED_EDGE('',*,*,#15051,.T.);
#21142=ORIENTED_EDGE('',*,*,#15052,.F.);
#21143=ORIENTED_EDGE('',*,*,#15053,.F.);
#21144=ORIENTED_EDGE('',*,*,#15054,.F.);
#21145=ORIENTED_EDGE('',*,*,#15051,.F.);
#21146=ORIENTED_EDGE('',*,*,#15048,.F.);
#21147=ORIENTED_EDGE('',*,*,#15055,.F.);
#21148=ORIENTED_EDGE('',*,*,#15056,.T.);
#21149=ORIENTED_EDGE('',*,*,#15057,.T.);
#21150=ORIENTED_EDGE('',*,*,#15058,.F.);
#21151=ORIENTED_EDGE('',*,*,#15057,.F.);
#21152=ORIENTED_EDGE('',*,*,#15059,.T.);
#21153=ORIENTED_EDGE('',*,*,#15060,.F.);
#21154=ORIENTED_EDGE('',*,*,#15061,.F.);
#21155=ORIENTED_EDGE('',*,*,#15062,.F.);
#21156=ORIENTED_EDGE('',*,*,#15059,.F.);
#21157=ORIENTED_EDGE('',*,*,#15056,.F.);
#21158=ORIENTED_EDGE('',*,*,#15063,.F.);
#21159=ORIENTED_EDGE('',*,*,#15064,.T.);
#21160=ORIENTED_EDGE('',*,*,#15065,.T.);
#21161=ORIENTED_EDGE('',*,*,#15066,.F.);
#21162=ORIENTED_EDGE('',*,*,#15065,.F.);
#21163=ORIENTED_EDGE('',*,*,#15067,.T.);
#21164=ORIENTED_EDGE('',*,*,#15068,.F.);
#21165=ORIENTED_EDGE('',*,*,#15069,.F.);
#21166=ORIENTED_EDGE('',*,*,#15070,.F.);
#21167=ORIENTED_EDGE('',*,*,#15067,.F.);
#21168=ORIENTED_EDGE('',*,*,#15064,.F.);
#21169=ORIENTED_EDGE('',*,*,#15071,.F.);
#21170=ORIENTED_EDGE('',*,*,#15072,.T.);
#21171=ORIENTED_EDGE('',*,*,#15073,.T.);
#21172=ORIENTED_EDGE('',*,*,#15074,.F.);
#21173=ORIENTED_EDGE('',*,*,#15073,.F.);
#21174=ORIENTED_EDGE('',*,*,#15075,.T.);
#21175=ORIENTED_EDGE('',*,*,#15076,.F.);
#21176=ORIENTED_EDGE('',*,*,#15077,.F.);
#21177=ORIENTED_EDGE('',*,*,#15078,.F.);
#21178=ORIENTED_EDGE('',*,*,#15075,.F.);
#21179=ORIENTED_EDGE('',*,*,#15072,.F.);
#21180=ORIENTED_EDGE('',*,*,#15079,.F.);
#21181=ORIENTED_EDGE('',*,*,#15080,.T.);
#21182=ORIENTED_EDGE('',*,*,#15081,.T.);
#21183=ORIENTED_EDGE('',*,*,#15082,.F.);
#21184=ORIENTED_EDGE('',*,*,#15081,.F.);
#21185=ORIENTED_EDGE('',*,*,#15083,.T.);
#21186=ORIENTED_EDGE('',*,*,#15084,.F.);
#21187=ORIENTED_EDGE('',*,*,#15085,.F.);
#21188=ORIENTED_EDGE('',*,*,#15086,.F.);
#21189=ORIENTED_EDGE('',*,*,#15083,.F.);
#21190=ORIENTED_EDGE('',*,*,#15080,.F.);
#21191=ORIENTED_EDGE('',*,*,#15087,.F.);
#21192=ORIENTED_EDGE('',*,*,#15088,.T.);
#21193=ORIENTED_EDGE('',*,*,#15089,.T.);
#21194=ORIENTED_EDGE('',*,*,#15090,.F.);
#21195=ORIENTED_EDGE('',*,*,#15089,.F.);
#21196=ORIENTED_EDGE('',*,*,#15091,.T.);
#21197=ORIENTED_EDGE('',*,*,#15092,.F.);
#21198=ORIENTED_EDGE('',*,*,#15093,.F.);
#21199=ORIENTED_EDGE('',*,*,#15094,.F.);
#21200=ORIENTED_EDGE('',*,*,#15091,.F.);
#21201=ORIENTED_EDGE('',*,*,#15088,.F.);
#21202=ORIENTED_EDGE('',*,*,#15095,.F.);
#21203=ORIENTED_EDGE('',*,*,#15096,.T.);
#21204=ORIENTED_EDGE('',*,*,#15097,.T.);
#21205=ORIENTED_EDGE('',*,*,#15098,.F.);
#21206=ORIENTED_EDGE('',*,*,#15097,.F.);
#21207=ORIENTED_EDGE('',*,*,#15099,.T.);
#21208=ORIENTED_EDGE('',*,*,#15100,.F.);
#21209=ORIENTED_EDGE('',*,*,#15101,.F.);
#21210=ORIENTED_EDGE('',*,*,#15102,.F.);
#21211=ORIENTED_EDGE('',*,*,#15099,.F.);
#21212=ORIENTED_EDGE('',*,*,#15096,.F.);
#21213=ORIENTED_EDGE('',*,*,#15103,.F.);
#21214=ORIENTED_EDGE('',*,*,#15104,.T.);
#21215=ORIENTED_EDGE('',*,*,#15105,.T.);
#21216=ORIENTED_EDGE('',*,*,#15106,.F.);
#21217=ORIENTED_EDGE('',*,*,#15105,.F.);
#21218=ORIENTED_EDGE('',*,*,#15107,.T.);
#21219=ORIENTED_EDGE('',*,*,#15108,.F.);
#21220=ORIENTED_EDGE('',*,*,#15109,.F.);
#21221=ORIENTED_EDGE('',*,*,#15110,.F.);
#21222=ORIENTED_EDGE('',*,*,#15107,.F.);
#21223=ORIENTED_EDGE('',*,*,#15104,.F.);
#21224=ORIENTED_EDGE('',*,*,#14836,.T.);
#21225=ORIENTED_EDGE('',*,*,#14830,.T.);
#21226=ORIENTED_EDGE('',*,*,#14833,.T.);
#21227=ORIENTED_EDGE('',*,*,#15111,.F.);
#21228=ORIENTED_EDGE('',*,*,#14844,.T.);
#21229=ORIENTED_EDGE('',*,*,#14838,.T.);
#21230=ORIENTED_EDGE('',*,*,#14841,.T.);
#21231=ORIENTED_EDGE('',*,*,#15112,.F.);
#21232=ORIENTED_EDGE('',*,*,#14852,.T.);
#21233=ORIENTED_EDGE('',*,*,#14846,.T.);
#21234=ORIENTED_EDGE('',*,*,#14849,.T.);
#21235=ORIENTED_EDGE('',*,*,#15113,.F.);
#21236=ORIENTED_EDGE('',*,*,#14860,.T.);
#21237=ORIENTED_EDGE('',*,*,#14854,.T.);
#21238=ORIENTED_EDGE('',*,*,#14857,.T.);
#21239=ORIENTED_EDGE('',*,*,#15114,.F.);
#21240=ORIENTED_EDGE('',*,*,#14868,.T.);
#21241=ORIENTED_EDGE('',*,*,#14862,.T.);
#21242=ORIENTED_EDGE('',*,*,#14865,.T.);
#21243=ORIENTED_EDGE('',*,*,#15115,.F.);
#21244=ORIENTED_EDGE('',*,*,#14876,.T.);
#21245=ORIENTED_EDGE('',*,*,#14870,.T.);
#21246=ORIENTED_EDGE('',*,*,#14873,.T.);
#21247=ORIENTED_EDGE('',*,*,#15116,.F.);
#21248=ORIENTED_EDGE('',*,*,#14884,.T.);
#21249=ORIENTED_EDGE('',*,*,#14878,.T.);
#21250=ORIENTED_EDGE('',*,*,#14881,.T.);
#21251=ORIENTED_EDGE('',*,*,#15117,.F.);
#21252=ORIENTED_EDGE('',*,*,#14892,.T.);
#21253=ORIENTED_EDGE('',*,*,#14886,.T.);
#21254=ORIENTED_EDGE('',*,*,#14889,.T.);
#21255=ORIENTED_EDGE('',*,*,#15118,.F.);
#21256=ORIENTED_EDGE('',*,*,#14900,.T.);
#21257=ORIENTED_EDGE('',*,*,#14894,.T.);
#21258=ORIENTED_EDGE('',*,*,#14897,.T.);
#21259=ORIENTED_EDGE('',*,*,#15119,.F.);
#21260=ORIENTED_EDGE('',*,*,#14908,.T.);
#21261=ORIENTED_EDGE('',*,*,#14902,.T.);
#21262=ORIENTED_EDGE('',*,*,#14905,.T.);
#21263=ORIENTED_EDGE('',*,*,#15120,.F.);
#21264=ORIENTED_EDGE('',*,*,#14916,.T.);
#21265=ORIENTED_EDGE('',*,*,#14910,.T.);
#21266=ORIENTED_EDGE('',*,*,#14913,.T.);
#21267=ORIENTED_EDGE('',*,*,#15121,.F.);
#21268=ORIENTED_EDGE('',*,*,#14924,.T.);
#21269=ORIENTED_EDGE('',*,*,#14918,.T.);
#21270=ORIENTED_EDGE('',*,*,#14921,.T.);
#21271=ORIENTED_EDGE('',*,*,#15122,.F.);
#21272=ORIENTED_EDGE('',*,*,#14932,.T.);
#21273=ORIENTED_EDGE('',*,*,#14926,.T.);
#21274=ORIENTED_EDGE('',*,*,#14929,.T.);
#21275=ORIENTED_EDGE('',*,*,#15123,.F.);
#21276=ORIENTED_EDGE('',*,*,#14940,.T.);
#21277=ORIENTED_EDGE('',*,*,#14934,.T.);
#21278=ORIENTED_EDGE('',*,*,#14937,.T.);
#21279=ORIENTED_EDGE('',*,*,#15124,.F.);
#21280=ORIENTED_EDGE('',*,*,#14948,.T.);
#21281=ORIENTED_EDGE('',*,*,#14942,.T.);
#21282=ORIENTED_EDGE('',*,*,#14945,.T.);
#21283=ORIENTED_EDGE('',*,*,#15125,.F.);
#21284=ORIENTED_EDGE('',*,*,#14956,.T.);
#21285=ORIENTED_EDGE('',*,*,#14950,.T.);
#21286=ORIENTED_EDGE('',*,*,#14953,.T.);
#21287=ORIENTED_EDGE('',*,*,#15126,.F.);
#21288=ORIENTED_EDGE('',*,*,#14964,.T.);
#21289=ORIENTED_EDGE('',*,*,#14958,.T.);
#21290=ORIENTED_EDGE('',*,*,#14961,.T.);
#21291=ORIENTED_EDGE('',*,*,#15127,.F.);
#21292=ORIENTED_EDGE('',*,*,#14973,.T.);
#21293=ORIENTED_EDGE('',*,*,#14966,.T.);
#21294=ORIENTED_EDGE('',*,*,#15128,.T.);
#21295=ORIENTED_EDGE('',*,*,#15129,.T.);
#21296=ORIENTED_EDGE('',*,*,#15128,.F.);
#21297=ORIENTED_EDGE('',*,*,#14969,.T.);
#21298=ORIENTED_EDGE('',*,*,#14970,.T.);
#21299=ORIENTED_EDGE('',*,*,#15130,.F.);
#21300=ORIENTED_EDGE('',*,*,#14981,.T.);
#21301=ORIENTED_EDGE('',*,*,#14975,.T.);
#21302=ORIENTED_EDGE('',*,*,#14978,.T.);
#21303=ORIENTED_EDGE('',*,*,#15131,.F.);
#21304=ORIENTED_EDGE('',*,*,#14989,.T.);
#21305=ORIENTED_EDGE('',*,*,#14983,.T.);
#21306=ORIENTED_EDGE('',*,*,#14986,.T.);
#21307=ORIENTED_EDGE('',*,*,#15132,.F.);
#21308=ORIENTED_EDGE('',*,*,#14997,.T.);
#21309=ORIENTED_EDGE('',*,*,#14991,.T.);
#21310=ORIENTED_EDGE('',*,*,#14994,.T.);
#21311=ORIENTED_EDGE('',*,*,#15133,.F.);
#21312=ORIENTED_EDGE('',*,*,#15005,.T.);
#21313=ORIENTED_EDGE('',*,*,#14999,.T.);
#21314=ORIENTED_EDGE('',*,*,#15002,.T.);
#21315=ORIENTED_EDGE('',*,*,#15134,.F.);
#21316=ORIENTED_EDGE('',*,*,#15013,.T.);
#21317=ORIENTED_EDGE('',*,*,#15007,.T.);
#21318=ORIENTED_EDGE('',*,*,#15010,.T.);
#21319=ORIENTED_EDGE('',*,*,#15135,.F.);
#21320=ORIENTED_EDGE('',*,*,#15021,.T.);
#21321=ORIENTED_EDGE('',*,*,#15015,.T.);
#21322=ORIENTED_EDGE('',*,*,#15018,.T.);
#21323=ORIENTED_EDGE('',*,*,#15136,.F.);
#21324=ORIENTED_EDGE('',*,*,#15029,.T.);
#21325=ORIENTED_EDGE('',*,*,#15023,.T.);
#21326=ORIENTED_EDGE('',*,*,#15026,.T.);
#21327=ORIENTED_EDGE('',*,*,#15137,.F.);
#21328=ORIENTED_EDGE('',*,*,#15037,.T.);
#21329=ORIENTED_EDGE('',*,*,#15031,.T.);
#21330=ORIENTED_EDGE('',*,*,#15034,.T.);
#21331=ORIENTED_EDGE('',*,*,#15138,.F.);
#21332=ORIENTED_EDGE('',*,*,#15045,.T.);
#21333=ORIENTED_EDGE('',*,*,#15039,.T.);
#21334=ORIENTED_EDGE('',*,*,#15042,.T.);
#21335=ORIENTED_EDGE('',*,*,#15139,.F.);
#21336=ORIENTED_EDGE('',*,*,#15053,.T.);
#21337=ORIENTED_EDGE('',*,*,#15047,.T.);
#21338=ORIENTED_EDGE('',*,*,#15050,.T.);
#21339=ORIENTED_EDGE('',*,*,#15140,.F.);
#21340=ORIENTED_EDGE('',*,*,#15061,.T.);
#21341=ORIENTED_EDGE('',*,*,#15055,.T.);
#21342=ORIENTED_EDGE('',*,*,#15058,.T.);
#21343=ORIENTED_EDGE('',*,*,#15141,.F.);
#21344=ORIENTED_EDGE('',*,*,#15069,.T.);
#21345=ORIENTED_EDGE('',*,*,#15063,.T.);
#21346=ORIENTED_EDGE('',*,*,#15066,.T.);
#21347=ORIENTED_EDGE('',*,*,#15142,.F.);
#21348=ORIENTED_EDGE('',*,*,#15077,.T.);
#21349=ORIENTED_EDGE('',*,*,#15071,.T.);
#21350=ORIENTED_EDGE('',*,*,#15074,.T.);
#21351=ORIENTED_EDGE('',*,*,#15143,.F.);
#21352=ORIENTED_EDGE('',*,*,#15085,.T.);
#21353=ORIENTED_EDGE('',*,*,#15079,.T.);
#21354=ORIENTED_EDGE('',*,*,#15082,.T.);
#21355=ORIENTED_EDGE('',*,*,#15144,.F.);
#21356=ORIENTED_EDGE('',*,*,#15093,.T.);
#21357=ORIENTED_EDGE('',*,*,#15087,.T.);
#21358=ORIENTED_EDGE('',*,*,#15090,.T.);
#21359=ORIENTED_EDGE('',*,*,#15145,.F.);
#21360=ORIENTED_EDGE('',*,*,#15101,.T.);
#21361=ORIENTED_EDGE('',*,*,#15095,.T.);
#21362=ORIENTED_EDGE('',*,*,#15098,.T.);
#21363=ORIENTED_EDGE('',*,*,#15146,.F.);
#21364=ORIENTED_EDGE('',*,*,#15109,.T.);
#21365=ORIENTED_EDGE('',*,*,#15103,.T.);
#21366=ORIENTED_EDGE('',*,*,#15106,.T.);
#21367=ORIENTED_EDGE('',*,*,#15147,.F.);
#21368=ORIENTED_EDGE('',*,*,#15148,.T.);
#21369=ORIENTED_EDGE('',*,*,#15149,.T.);
#21370=ORIENTED_EDGE('',*,*,#15150,.T.);
#21371=ORIENTED_EDGE('',*,*,#15151,.F.);
#21372=ORIENTED_EDGE('',*,*,#15150,.F.);
#21373=ORIENTED_EDGE('',*,*,#15152,.F.);
#21374=ORIENTED_EDGE('',*,*,#15153,.T.);
#21375=ORIENTED_EDGE('',*,*,#15154,.F.);
#21376=ORIENTED_EDGE('',*,*,#15155,.F.);
#21377=ORIENTED_EDGE('',*,*,#15153,.F.);
#21378=ORIENTED_EDGE('',*,*,#15156,.F.);
#21379=ORIENTED_EDGE('',*,*,#15148,.F.);
#21380=ORIENTED_EDGE('',*,*,#15149,.F.);
#21381=ORIENTED_EDGE('',*,*,#15156,.T.);
#21382=ORIENTED_EDGE('',*,*,#15152,.T.);
#21383=ORIENTED_EDGE('',*,*,#15157,.F.);
#21384=ORIENTED_EDGE('',*,*,#15158,.T.);
#21385=ORIENTED_EDGE('',*,*,#14974,.T.);
#21386=ORIENTED_EDGE('',*,*,#15127,.T.);
#21387=ORIENTED_EDGE('',*,*,#14963,.T.);
#21388=ORIENTED_EDGE('',*,*,#14965,.T.);
#21389=ORIENTED_EDGE('',*,*,#15126,.T.);
#21390=ORIENTED_EDGE('',*,*,#14955,.T.);
#21391=ORIENTED_EDGE('',*,*,#14957,.T.);
#21392=ORIENTED_EDGE('',*,*,#15125,.T.);
#21393=ORIENTED_EDGE('',*,*,#14947,.T.);
#21394=ORIENTED_EDGE('',*,*,#14949,.T.);
#21395=ORIENTED_EDGE('',*,*,#15124,.T.);
#21396=ORIENTED_EDGE('',*,*,#14939,.T.);
#21397=ORIENTED_EDGE('',*,*,#14941,.T.);
#21398=ORIENTED_EDGE('',*,*,#15123,.T.);
#21399=ORIENTED_EDGE('',*,*,#14931,.T.);
#21400=ORIENTED_EDGE('',*,*,#14933,.T.);
#21401=ORIENTED_EDGE('',*,*,#15122,.T.);
#21402=ORIENTED_EDGE('',*,*,#14923,.T.);
#21403=ORIENTED_EDGE('',*,*,#14925,.T.);
#21404=ORIENTED_EDGE('',*,*,#15121,.T.);
#21405=ORIENTED_EDGE('',*,*,#14915,.T.);
#21406=ORIENTED_EDGE('',*,*,#14917,.T.);
#21407=ORIENTED_EDGE('',*,*,#15120,.T.);
#21408=ORIENTED_EDGE('',*,*,#14907,.T.);
#21409=ORIENTED_EDGE('',*,*,#14909,.T.);
#21410=ORIENTED_EDGE('',*,*,#15119,.T.);
#21411=ORIENTED_EDGE('',*,*,#14899,.T.);
#21412=ORIENTED_EDGE('',*,*,#14901,.T.);
#21413=ORIENTED_EDGE('',*,*,#15118,.T.);
#21414=ORIENTED_EDGE('',*,*,#14891,.T.);
#21415=ORIENTED_EDGE('',*,*,#14893,.T.);
#21416=ORIENTED_EDGE('',*,*,#15117,.T.);
#21417=ORIENTED_EDGE('',*,*,#14883,.T.);
#21418=ORIENTED_EDGE('',*,*,#14885,.T.);
#21419=ORIENTED_EDGE('',*,*,#15116,.T.);
#21420=ORIENTED_EDGE('',*,*,#14875,.T.);
#21421=ORIENTED_EDGE('',*,*,#14877,.T.);
#21422=ORIENTED_EDGE('',*,*,#15115,.T.);
#21423=ORIENTED_EDGE('',*,*,#14867,.T.);
#21424=ORIENTED_EDGE('',*,*,#14869,.T.);
#21425=ORIENTED_EDGE('',*,*,#15114,.T.);
#21426=ORIENTED_EDGE('',*,*,#14859,.T.);
#21427=ORIENTED_EDGE('',*,*,#14861,.T.);
#21428=ORIENTED_EDGE('',*,*,#15113,.T.);
#21429=ORIENTED_EDGE('',*,*,#14851,.T.);
#21430=ORIENTED_EDGE('',*,*,#14853,.T.);
#21431=ORIENTED_EDGE('',*,*,#15112,.T.);
#21432=ORIENTED_EDGE('',*,*,#14843,.T.);
#21433=ORIENTED_EDGE('',*,*,#14845,.T.);
#21434=ORIENTED_EDGE('',*,*,#15111,.T.);
#21435=ORIENTED_EDGE('',*,*,#14835,.T.);
#21436=ORIENTED_EDGE('',*,*,#14837,.T.);
#21437=ORIENTED_EDGE('',*,*,#15151,.T.);
#21438=ORIENTED_EDGE('',*,*,#15154,.T.);
#21439=ORIENTED_EDGE('',*,*,#15155,.T.);
#21440=ORIENTED_EDGE('',*,*,#15147,.T.);
#21441=ORIENTED_EDGE('',*,*,#15108,.T.);
#21442=ORIENTED_EDGE('',*,*,#15110,.T.);
#21443=ORIENTED_EDGE('',*,*,#15146,.T.);
#21444=ORIENTED_EDGE('',*,*,#15100,.T.);
#21445=ORIENTED_EDGE('',*,*,#15102,.T.);
#21446=ORIENTED_EDGE('',*,*,#15145,.T.);
#21447=ORIENTED_EDGE('',*,*,#15092,.T.);
#21448=ORIENTED_EDGE('',*,*,#15094,.T.);
#21449=ORIENTED_EDGE('',*,*,#15144,.T.);
#21450=ORIENTED_EDGE('',*,*,#15084,.T.);
#21451=ORIENTED_EDGE('',*,*,#15086,.T.);
#21452=ORIENTED_EDGE('',*,*,#15143,.T.);
#21453=ORIENTED_EDGE('',*,*,#15076,.T.);
#21454=ORIENTED_EDGE('',*,*,#15078,.T.);
#21455=ORIENTED_EDGE('',*,*,#15142,.T.);
#21456=ORIENTED_EDGE('',*,*,#15068,.T.);
#21457=ORIENTED_EDGE('',*,*,#15070,.T.);
#21458=ORIENTED_EDGE('',*,*,#15141,.T.);
#21459=ORIENTED_EDGE('',*,*,#15060,.T.);
#21460=ORIENTED_EDGE('',*,*,#15062,.T.);
#21461=ORIENTED_EDGE('',*,*,#15140,.T.);
#21462=ORIENTED_EDGE('',*,*,#15052,.T.);
#21463=ORIENTED_EDGE('',*,*,#15054,.T.);
#21464=ORIENTED_EDGE('',*,*,#15139,.T.);
#21465=ORIENTED_EDGE('',*,*,#15044,.T.);
#21466=ORIENTED_EDGE('',*,*,#15046,.T.);
#21467=ORIENTED_EDGE('',*,*,#15138,.T.);
#21468=ORIENTED_EDGE('',*,*,#15036,.T.);
#21469=ORIENTED_EDGE('',*,*,#15038,.T.);
#21470=ORIENTED_EDGE('',*,*,#15137,.T.);
#21471=ORIENTED_EDGE('',*,*,#15028,.T.);
#21472=ORIENTED_EDGE('',*,*,#15030,.T.);
#21473=ORIENTED_EDGE('',*,*,#15136,.T.);
#21474=ORIENTED_EDGE('',*,*,#15020,.T.);
#21475=ORIENTED_EDGE('',*,*,#15022,.T.);
#21476=ORIENTED_EDGE('',*,*,#15135,.T.);
#21477=ORIENTED_EDGE('',*,*,#15012,.T.);
#21478=ORIENTED_EDGE('',*,*,#15014,.T.);
#21479=ORIENTED_EDGE('',*,*,#15134,.T.);
#21480=ORIENTED_EDGE('',*,*,#15004,.T.);
#21481=ORIENTED_EDGE('',*,*,#15006,.T.);
#21482=ORIENTED_EDGE('',*,*,#15133,.T.);
#21483=ORIENTED_EDGE('',*,*,#14996,.T.);
#21484=ORIENTED_EDGE('',*,*,#14998,.T.);
#21485=ORIENTED_EDGE('',*,*,#15132,.T.);
#21486=ORIENTED_EDGE('',*,*,#14988,.T.);
#21487=ORIENTED_EDGE('',*,*,#14990,.T.);
#21488=ORIENTED_EDGE('',*,*,#15131,.T.);
#21489=ORIENTED_EDGE('',*,*,#14980,.T.);
#21490=ORIENTED_EDGE('',*,*,#14982,.T.);
#21491=ORIENTED_EDGE('',*,*,#15130,.T.);
#21492=ORIENTED_EDGE('',*,*,#14972,.T.);
#21493=ORIENTED_EDGE('',*,*,#15158,.F.);
#21494=ORIENTED_EDGE('',*,*,#15159,.T.);
#21495=ORIENTED_EDGE('',*,*,#15160,.F.);
#21496=ORIENTED_EDGE('',*,*,#15159,.F.);
#21497=ORIENTED_EDGE('',*,*,#15161,.F.);
#21498=ORIENTED_EDGE('',*,*,#15162,.T.);
#21499=ORIENTED_EDGE('',*,*,#15163,.T.);
#21500=ORIENTED_EDGE('',*,*,#15164,.F.);
#21501=ORIENTED_EDGE('',*,*,#15165,.F.);
#21502=ORIENTED_EDGE('',*,*,#15166,.T.);
#21503=ORIENTED_EDGE('',*,*,#15167,.T.);
#21504=ORIENTED_EDGE('',*,*,#15162,.F.);
#21505=ORIENTED_EDGE('',*,*,#15168,.F.);
#21506=ORIENTED_EDGE('',*,*,#15169,.T.);
#21507=ORIENTED_EDGE('',*,*,#15170,.T.);
#21508=ORIENTED_EDGE('',*,*,#15166,.F.);
#21509=ORIENTED_EDGE('',*,*,#15171,.F.);
#21510=ORIENTED_EDGE('',*,*,#15172,.T.);
#21511=ORIENTED_EDGE('',*,*,#15173,.T.);
#21512=ORIENTED_EDGE('',*,*,#15169,.F.);
#21513=ORIENTED_EDGE('',*,*,#15174,.F.);
#21514=ORIENTED_EDGE('',*,*,#15175,.T.);
#21515=ORIENTED_EDGE('',*,*,#15176,.T.);
#21516=ORIENTED_EDGE('',*,*,#15172,.F.);
#21517=ORIENTED_EDGE('',*,*,#15177,.F.);
#21518=ORIENTED_EDGE('',*,*,#15164,.T.);
#21519=ORIENTED_EDGE('',*,*,#15178,.T.);
#21520=ORIENTED_EDGE('',*,*,#15175,.F.);
#21521=ORIENTED_EDGE('',*,*,#15178,.F.);
#21522=ORIENTED_EDGE('',*,*,#15163,.F.);
#21523=ORIENTED_EDGE('',*,*,#15167,.F.);
#21524=ORIENTED_EDGE('',*,*,#15170,.F.);
#21525=ORIENTED_EDGE('',*,*,#15173,.F.);
#21526=ORIENTED_EDGE('',*,*,#15176,.F.);
#21527=ORIENTED_EDGE('',*,*,#15160,.T.);
#21528=ORIENTED_EDGE('',*,*,#15179,.F.);
#21529=ORIENTED_EDGE('',*,*,#14677,.F.);
#21530=ORIENTED_EDGE('',*,*,#15180,.T.);
#21531=ORIENTED_EDGE('',*,*,#15179,.T.);
#21532=ORIENTED_EDGE('',*,*,#15180,.F.);
#21533=ORIENTED_EDGE('',*,*,#14743,.T.);
#21534=ORIENTED_EDGE('',*,*,#14824,.T.);
#21535=ORIENTED_EDGE('',*,*,#15181,.F.);
#21536=ORIENTED_EDGE('',*,*,#14829,.T.);
#21537=ORIENTED_EDGE('',*,*,#15182,.F.);
#21538=ORIENTED_EDGE('',*,*,#15183,.T.);
#21539=ORIENTED_EDGE('',*,*,#14821,.T.);
#21540=ORIENTED_EDGE('',*,*,#15181,.T.);
#21541=ORIENTED_EDGE('',*,*,#14822,.T.);
#21542=ORIENTED_EDGE('',*,*,#15183,.F.);
#21543=ORIENTED_EDGE('',*,*,#15129,.F.);
#21544=ORIENTED_EDGE('',*,*,#15182,.T.);
#21545=ORIENTED_EDGE('',*,*,#15157,.T.);
#21546=ORIENTED_EDGE('',*,*,#15161,.T.);
#21547=ORIENTED_EDGE('',*,*,#15177,.T.);
#21548=ORIENTED_EDGE('',*,*,#15174,.T.);
#21549=ORIENTED_EDGE('',*,*,#15171,.T.);
#21550=ORIENTED_EDGE('',*,*,#15168,.T.);
#21551=ORIENTED_EDGE('',*,*,#15165,.T.);
#21552=ORIENTED_EDGE('',*,*,#15184,.F.);
#21553=ORIENTED_EDGE('',*,*,#15185,.T.);
#21554=ORIENTED_EDGE('',*,*,#15186,.T.);
#21555=ORIENTED_EDGE('',*,*,#15187,.T.);
#21556=ORIENTED_EDGE('',*,*,#15188,.T.);
#21557=ORIENTED_EDGE('',*,*,#15187,.F.);
#21558=ORIENTED_EDGE('',*,*,#15189,.T.);
#21559=ORIENTED_EDGE('',*,*,#15190,.T.);
#21560=ORIENTED_EDGE('',*,*,#15191,.F.);
#21561=ORIENTED_EDGE('',*,*,#15192,.T.);
#21562=ORIENTED_EDGE('',*,*,#15184,.T.);
#21563=ORIENTED_EDGE('',*,*,#15193,.T.);
#21564=ORIENTED_EDGE('',*,*,#15194,.F.);
#21565=ORIENTED_EDGE('',*,*,#15195,.T.);
#21566=ORIENTED_EDGE('',*,*,#15191,.T.);
#21567=ORIENTED_EDGE('',*,*,#15196,.T.);
#21568=ORIENTED_EDGE('',*,*,#15197,.F.);
#21569=ORIENTED_EDGE('',*,*,#15198,.T.);
#21570=ORIENTED_EDGE('',*,*,#15194,.T.);
#21571=ORIENTED_EDGE('',*,*,#15199,.T.);
#21572=ORIENTED_EDGE('',*,*,#15200,.F.);
#21573=ORIENTED_EDGE('',*,*,#15201,.T.);
#21574=ORIENTED_EDGE('',*,*,#15197,.T.);
#21575=ORIENTED_EDGE('',*,*,#15202,.T.);
#21576=ORIENTED_EDGE('',*,*,#15203,.F.);
#21577=ORIENTED_EDGE('',*,*,#15204,.T.);
#21578=ORIENTED_EDGE('',*,*,#15200,.T.);
#21579=ORIENTED_EDGE('',*,*,#15205,.T.);
#21580=ORIENTED_EDGE('',*,*,#15206,.F.);
#21581=ORIENTED_EDGE('',*,*,#15207,.T.);
#21582=ORIENTED_EDGE('',*,*,#15203,.T.);
#21583=ORIENTED_EDGE('',*,*,#15208,.T.);
#21584=ORIENTED_EDGE('',*,*,#15209,.F.);
#21585=ORIENTED_EDGE('',*,*,#15210,.T.);
#21586=ORIENTED_EDGE('',*,*,#15206,.T.);
#21587=ORIENTED_EDGE('',*,*,#15211,.T.);
#21588=ORIENTED_EDGE('',*,*,#15212,.F.);
#21589=ORIENTED_EDGE('',*,*,#15213,.T.);
#21590=ORIENTED_EDGE('',*,*,#15209,.T.);
#21591=ORIENTED_EDGE('',*,*,#15214,.T.);
#21592=ORIENTED_EDGE('',*,*,#15215,.F.);
#21593=ORIENTED_EDGE('',*,*,#15216,.T.);
#21594=ORIENTED_EDGE('',*,*,#15212,.T.);
#21595=ORIENTED_EDGE('',*,*,#15217,.T.);
#21596=ORIENTED_EDGE('',*,*,#15218,.F.);
#21597=ORIENTED_EDGE('',*,*,#15219,.T.);
#21598=ORIENTED_EDGE('',*,*,#15215,.T.);
#21599=ORIENTED_EDGE('',*,*,#15220,.T.);
#21600=ORIENTED_EDGE('',*,*,#15221,.F.);
#21601=ORIENTED_EDGE('',*,*,#15222,.T.);
#21602=ORIENTED_EDGE('',*,*,#15218,.T.);
#21603=ORIENTED_EDGE('',*,*,#15223,.T.);
#21604=ORIENTED_EDGE('',*,*,#15224,.F.);
#21605=ORIENTED_EDGE('',*,*,#15225,.T.);
#21606=ORIENTED_EDGE('',*,*,#15226,.F.);
#21607=ORIENTED_EDGE('',*,*,#15227,.F.);
#21608=ORIENTED_EDGE('',*,*,#15228,.F.);
#21609=ORIENTED_EDGE('',*,*,#15229,.T.);
#21610=ORIENTED_EDGE('',*,*,#15224,.T.);
#21611=ORIENTED_EDGE('',*,*,#15230,.F.);
#21612=ORIENTED_EDGE('',*,*,#15231,.F.);
#21613=ORIENTED_EDGE('',*,*,#15232,.T.);
#21614=ORIENTED_EDGE('',*,*,#15228,.T.);
#21615=ORIENTED_EDGE('',*,*,#15233,.F.);
#21616=ORIENTED_EDGE('',*,*,#15234,.F.);
#21617=ORIENTED_EDGE('',*,*,#15235,.T.);
#21618=ORIENTED_EDGE('',*,*,#15231,.T.);
#21619=ORIENTED_EDGE('',*,*,#15236,.F.);
#21620=ORIENTED_EDGE('',*,*,#15237,.F.);
#21621=ORIENTED_EDGE('',*,*,#15238,.T.);
#21622=ORIENTED_EDGE('',*,*,#15234,.T.);
#21623=ORIENTED_EDGE('',*,*,#15239,.F.);
#21624=ORIENTED_EDGE('',*,*,#15240,.F.);
#21625=ORIENTED_EDGE('',*,*,#15241,.T.);
#21626=ORIENTED_EDGE('',*,*,#15237,.T.);
#21627=ORIENTED_EDGE('',*,*,#15242,.F.);
#21628=ORIENTED_EDGE('',*,*,#15243,.F.);
#21629=ORIENTED_EDGE('',*,*,#15244,.T.);
#21630=ORIENTED_EDGE('',*,*,#15240,.T.);
#21631=ORIENTED_EDGE('',*,*,#15245,.F.);
#21632=ORIENTED_EDGE('',*,*,#15246,.F.);
#21633=ORIENTED_EDGE('',*,*,#15247,.T.);
#21634=ORIENTED_EDGE('',*,*,#15243,.T.);
#21635=ORIENTED_EDGE('',*,*,#15248,.F.);
#21636=ORIENTED_EDGE('',*,*,#15249,.F.);
#21637=ORIENTED_EDGE('',*,*,#15250,.T.);
#21638=ORIENTED_EDGE('',*,*,#15246,.T.);
#21639=ORIENTED_EDGE('',*,*,#15251,.F.);
#21640=ORIENTED_EDGE('',*,*,#15252,.F.);
#21641=ORIENTED_EDGE('',*,*,#15253,.T.);
#21642=ORIENTED_EDGE('',*,*,#15249,.T.);
#21643=ORIENTED_EDGE('',*,*,#15254,.F.);
#21644=ORIENTED_EDGE('',*,*,#15255,.F.);
#21645=ORIENTED_EDGE('',*,*,#15256,.T.);
#21646=ORIENTED_EDGE('',*,*,#15252,.T.);
#21647=ORIENTED_EDGE('',*,*,#15257,.F.);
#21648=ORIENTED_EDGE('',*,*,#15258,.F.);
#21649=ORIENTED_EDGE('',*,*,#15259,.F.);
#21650=ORIENTED_EDGE('',*,*,#15260,.T.);
#21651=ORIENTED_EDGE('',*,*,#15255,.T.);
#21652=ORIENTED_EDGE('',*,*,#15261,.F.);
#21653=ORIENTED_EDGE('',*,*,#15226,.T.);
#21654=ORIENTED_EDGE('',*,*,#15262,.T.);
#21655=ORIENTED_EDGE('',*,*,#15263,.F.);
#21656=ORIENTED_EDGE('',*,*,#15264,.F.);
#21657=ORIENTED_EDGE('',*,*,#15265,.T.);
#21658=ORIENTED_EDGE('',*,*,#15265,.F.);
#21659=ORIENTED_EDGE('',*,*,#15266,.F.);
#21660=ORIENTED_EDGE('',*,*,#15223,.F.);
#21661=ORIENTED_EDGE('',*,*,#15220,.F.);
#21662=ORIENTED_EDGE('',*,*,#15217,.F.);
#21663=ORIENTED_EDGE('',*,*,#15214,.F.);
#21664=ORIENTED_EDGE('',*,*,#15211,.F.);
#21665=ORIENTED_EDGE('',*,*,#15208,.F.);
#21666=ORIENTED_EDGE('',*,*,#15205,.F.);
#21667=ORIENTED_EDGE('',*,*,#15202,.F.);
#21668=ORIENTED_EDGE('',*,*,#15199,.F.);
#21669=ORIENTED_EDGE('',*,*,#15196,.F.);
#21670=ORIENTED_EDGE('',*,*,#15193,.F.);
#21671=ORIENTED_EDGE('',*,*,#15190,.F.);
#21672=ORIENTED_EDGE('',*,*,#15267,.F.);
#21673=ORIENTED_EDGE('',*,*,#15268,.T.);
#21674=ORIENTED_EDGE('',*,*,#15261,.T.);
#21675=ORIENTED_EDGE('',*,*,#15257,.T.);
#21676=ORIENTED_EDGE('',*,*,#15254,.T.);
#21677=ORIENTED_EDGE('',*,*,#15251,.T.);
#21678=ORIENTED_EDGE('',*,*,#15248,.T.);
#21679=ORIENTED_EDGE('',*,*,#15245,.T.);
#21680=ORIENTED_EDGE('',*,*,#15242,.T.);
#21681=ORIENTED_EDGE('',*,*,#15239,.T.);
#21682=ORIENTED_EDGE('',*,*,#15236,.T.);
#21683=ORIENTED_EDGE('',*,*,#15233,.T.);
#21684=ORIENTED_EDGE('',*,*,#15230,.T.);
#21685=ORIENTED_EDGE('',*,*,#15227,.T.);
#21686=ORIENTED_EDGE('',*,*,#15186,.F.);
#21687=ORIENTED_EDGE('',*,*,#15269,.T.);
#21688=ORIENTED_EDGE('',*,*,#15259,.T.);
#21689=ORIENTED_EDGE('',*,*,#15270,.T.);
#21690=ORIENTED_EDGE('',*,*,#15267,.T.);
#21691=ORIENTED_EDGE('',*,*,#15189,.F.);
#21692=ORIENTED_EDGE('',*,*,#15258,.T.);
#21693=ORIENTED_EDGE('',*,*,#15268,.F.);
#21694=ORIENTED_EDGE('',*,*,#15270,.F.);
#21695=ORIENTED_EDGE('',*,*,#15262,.F.);
#21696=ORIENTED_EDGE('',*,*,#15225,.F.);
#21697=ORIENTED_EDGE('',*,*,#15229,.F.);
#21698=ORIENTED_EDGE('',*,*,#15232,.F.);
#21699=ORIENTED_EDGE('',*,*,#15235,.F.);
#21700=ORIENTED_EDGE('',*,*,#15238,.F.);
#21701=ORIENTED_EDGE('',*,*,#15241,.F.);
#21702=ORIENTED_EDGE('',*,*,#15244,.F.);
#21703=ORIENTED_EDGE('',*,*,#15247,.F.);
#21704=ORIENTED_EDGE('',*,*,#15250,.F.);
#21705=ORIENTED_EDGE('',*,*,#15253,.F.);
#21706=ORIENTED_EDGE('',*,*,#15256,.F.);
#21707=ORIENTED_EDGE('',*,*,#15260,.F.);
#21708=ORIENTED_EDGE('',*,*,#15269,.F.);
#21709=ORIENTED_EDGE('',*,*,#15185,.F.);
#21710=ORIENTED_EDGE('',*,*,#15192,.F.);
#21711=ORIENTED_EDGE('',*,*,#15195,.F.);
#21712=ORIENTED_EDGE('',*,*,#15198,.F.);
#21713=ORIENTED_EDGE('',*,*,#15201,.F.);
#21714=ORIENTED_EDGE('',*,*,#15204,.F.);
#21715=ORIENTED_EDGE('',*,*,#15207,.F.);
#21716=ORIENTED_EDGE('',*,*,#15210,.F.);
#21717=ORIENTED_EDGE('',*,*,#15213,.F.);
#21718=ORIENTED_EDGE('',*,*,#15216,.F.);
#21719=ORIENTED_EDGE('',*,*,#15219,.F.);
#21720=ORIENTED_EDGE('',*,*,#15222,.F.);
#21721=ORIENTED_EDGE('',*,*,#15271,.F.);
#21722=ORIENTED_EDGE('',*,*,#15221,.T.);
#21723=ORIENTED_EDGE('',*,*,#15266,.T.);
#21724=ORIENTED_EDGE('',*,*,#15272,.F.);
#21725=ORIENTED_EDGE('',*,*,#15271,.T.);
#21726=ORIENTED_EDGE('',*,*,#15273,.F.);
#21727=ORIENTED_EDGE('',*,*,#15274,.T.);
#21728=ORIENTED_EDGE('',*,*,#15275,.T.);
#21729=ORIENTED_EDGE('',*,*,#15276,.F.);
#21730=ORIENTED_EDGE('',*,*,#15275,.F.);
#21731=ORIENTED_EDGE('',*,*,#15277,.T.);
#21732=ORIENTED_EDGE('',*,*,#15278,.F.);
#21733=ORIENTED_EDGE('',*,*,#15279,.F.);
#21734=ORIENTED_EDGE('',*,*,#15280,.F.);
#21735=ORIENTED_EDGE('',*,*,#15277,.F.);
#21736=ORIENTED_EDGE('',*,*,#15274,.F.);
#21737=ORIENTED_EDGE('',*,*,#15281,.F.);
#21738=ORIENTED_EDGE('',*,*,#15282,.T.);
#21739=ORIENTED_EDGE('',*,*,#15283,.T.);
#21740=ORIENTED_EDGE('',*,*,#15284,.F.);
#21741=ORIENTED_EDGE('',*,*,#15283,.F.);
#21742=ORIENTED_EDGE('',*,*,#15285,.T.);
#21743=ORIENTED_EDGE('',*,*,#15286,.F.);
#21744=ORIENTED_EDGE('',*,*,#15287,.F.);
#21745=ORIENTED_EDGE('',*,*,#15288,.F.);
#21746=ORIENTED_EDGE('',*,*,#15285,.F.);
#21747=ORIENTED_EDGE('',*,*,#15282,.F.);
#21748=ORIENTED_EDGE('',*,*,#15289,.F.);
#21749=ORIENTED_EDGE('',*,*,#15290,.T.);
#21750=ORIENTED_EDGE('',*,*,#15291,.T.);
#21751=ORIENTED_EDGE('',*,*,#15292,.F.);
#21752=ORIENTED_EDGE('',*,*,#15291,.F.);
#21753=ORIENTED_EDGE('',*,*,#15293,.T.);
#21754=ORIENTED_EDGE('',*,*,#15294,.F.);
#21755=ORIENTED_EDGE('',*,*,#15295,.F.);
#21756=ORIENTED_EDGE('',*,*,#15296,.F.);
#21757=ORIENTED_EDGE('',*,*,#15293,.F.);
#21758=ORIENTED_EDGE('',*,*,#15290,.F.);
#21759=ORIENTED_EDGE('',*,*,#15297,.F.);
#21760=ORIENTED_EDGE('',*,*,#15298,.T.);
#21761=ORIENTED_EDGE('',*,*,#15299,.T.);
#21762=ORIENTED_EDGE('',*,*,#15300,.F.);
#21763=ORIENTED_EDGE('',*,*,#15299,.F.);
#21764=ORIENTED_EDGE('',*,*,#15301,.T.);
#21765=ORIENTED_EDGE('',*,*,#15302,.F.);
#21766=ORIENTED_EDGE('',*,*,#15303,.F.);
#21767=ORIENTED_EDGE('',*,*,#15304,.F.);
#21768=ORIENTED_EDGE('',*,*,#15301,.F.);
#21769=ORIENTED_EDGE('',*,*,#15298,.F.);
#21770=ORIENTED_EDGE('',*,*,#15305,.F.);
#21771=ORIENTED_EDGE('',*,*,#15306,.T.);
#21772=ORIENTED_EDGE('',*,*,#15307,.T.);
#21773=ORIENTED_EDGE('',*,*,#15308,.F.);
#21774=ORIENTED_EDGE('',*,*,#15307,.F.);
#21775=ORIENTED_EDGE('',*,*,#15309,.T.);
#21776=ORIENTED_EDGE('',*,*,#15310,.F.);
#21777=ORIENTED_EDGE('',*,*,#15311,.F.);
#21778=ORIENTED_EDGE('',*,*,#15312,.F.);
#21779=ORIENTED_EDGE('',*,*,#15309,.F.);
#21780=ORIENTED_EDGE('',*,*,#15306,.F.);
#21781=ORIENTED_EDGE('',*,*,#15313,.F.);
#21782=ORIENTED_EDGE('',*,*,#15314,.T.);
#21783=ORIENTED_EDGE('',*,*,#15315,.T.);
#21784=ORIENTED_EDGE('',*,*,#15316,.F.);
#21785=ORIENTED_EDGE('',*,*,#15315,.F.);
#21786=ORIENTED_EDGE('',*,*,#15317,.T.);
#21787=ORIENTED_EDGE('',*,*,#15318,.F.);
#21788=ORIENTED_EDGE('',*,*,#15319,.F.);
#21789=ORIENTED_EDGE('',*,*,#15320,.F.);
#21790=ORIENTED_EDGE('',*,*,#15317,.F.);
#21791=ORIENTED_EDGE('',*,*,#15314,.F.);
#21792=ORIENTED_EDGE('',*,*,#15321,.F.);
#21793=ORIENTED_EDGE('',*,*,#15322,.T.);
#21794=ORIENTED_EDGE('',*,*,#15323,.T.);
#21795=ORIENTED_EDGE('',*,*,#15324,.F.);
#21796=ORIENTED_EDGE('',*,*,#15323,.F.);
#21797=ORIENTED_EDGE('',*,*,#15325,.T.);
#21798=ORIENTED_EDGE('',*,*,#15326,.F.);
#21799=ORIENTED_EDGE('',*,*,#15327,.F.);
#21800=ORIENTED_EDGE('',*,*,#15328,.F.);
#21801=ORIENTED_EDGE('',*,*,#15325,.F.);
#21802=ORIENTED_EDGE('',*,*,#15322,.F.);
#21803=ORIENTED_EDGE('',*,*,#15329,.F.);
#21804=ORIENTED_EDGE('',*,*,#15330,.T.);
#21805=ORIENTED_EDGE('',*,*,#15331,.T.);
#21806=ORIENTED_EDGE('',*,*,#15332,.F.);
#21807=ORIENTED_EDGE('',*,*,#15331,.F.);
#21808=ORIENTED_EDGE('',*,*,#15333,.T.);
#21809=ORIENTED_EDGE('',*,*,#15334,.F.);
#21810=ORIENTED_EDGE('',*,*,#15335,.F.);
#21811=ORIENTED_EDGE('',*,*,#15336,.F.);
#21812=ORIENTED_EDGE('',*,*,#15333,.F.);
#21813=ORIENTED_EDGE('',*,*,#15330,.F.);
#21814=ORIENTED_EDGE('',*,*,#15337,.F.);
#21815=ORIENTED_EDGE('',*,*,#15338,.T.);
#21816=ORIENTED_EDGE('',*,*,#15339,.T.);
#21817=ORIENTED_EDGE('',*,*,#15340,.F.);
#21818=ORIENTED_EDGE('',*,*,#15339,.F.);
#21819=ORIENTED_EDGE('',*,*,#15341,.T.);
#21820=ORIENTED_EDGE('',*,*,#15342,.F.);
#21821=ORIENTED_EDGE('',*,*,#15343,.F.);
#21822=ORIENTED_EDGE('',*,*,#15344,.F.);
#21823=ORIENTED_EDGE('',*,*,#15341,.F.);
#21824=ORIENTED_EDGE('',*,*,#15338,.F.);
#21825=ORIENTED_EDGE('',*,*,#15345,.F.);
#21826=ORIENTED_EDGE('',*,*,#15346,.T.);
#21827=ORIENTED_EDGE('',*,*,#15347,.T.);
#21828=ORIENTED_EDGE('',*,*,#15348,.F.);
#21829=ORIENTED_EDGE('',*,*,#15347,.F.);
#21830=ORIENTED_EDGE('',*,*,#15349,.T.);
#21831=ORIENTED_EDGE('',*,*,#15350,.F.);
#21832=ORIENTED_EDGE('',*,*,#15351,.F.);
#21833=ORIENTED_EDGE('',*,*,#15352,.F.);
#21834=ORIENTED_EDGE('',*,*,#15349,.F.);
#21835=ORIENTED_EDGE('',*,*,#15346,.F.);
#21836=ORIENTED_EDGE('',*,*,#15353,.F.);
#21837=ORIENTED_EDGE('',*,*,#15354,.T.);
#21838=ORIENTED_EDGE('',*,*,#15355,.T.);
#21839=ORIENTED_EDGE('',*,*,#15356,.F.);
#21840=ORIENTED_EDGE('',*,*,#15355,.F.);
#21841=ORIENTED_EDGE('',*,*,#15357,.T.);
#21842=ORIENTED_EDGE('',*,*,#15358,.F.);
#21843=ORIENTED_EDGE('',*,*,#15359,.F.);
#21844=ORIENTED_EDGE('',*,*,#15360,.F.);
#21845=ORIENTED_EDGE('',*,*,#15357,.F.);
#21846=ORIENTED_EDGE('',*,*,#15354,.F.);
#21847=ORIENTED_EDGE('',*,*,#15361,.F.);
#21848=ORIENTED_EDGE('',*,*,#15362,.T.);
#21849=ORIENTED_EDGE('',*,*,#15363,.T.);
#21850=ORIENTED_EDGE('',*,*,#15364,.F.);
#21851=ORIENTED_EDGE('',*,*,#15363,.F.);
#21852=ORIENTED_EDGE('',*,*,#15365,.T.);
#21853=ORIENTED_EDGE('',*,*,#15366,.F.);
#21854=ORIENTED_EDGE('',*,*,#15367,.F.);
#21855=ORIENTED_EDGE('',*,*,#15368,.F.);
#21856=ORIENTED_EDGE('',*,*,#15365,.F.);
#21857=ORIENTED_EDGE('',*,*,#15362,.F.);
#21858=ORIENTED_EDGE('',*,*,#15369,.F.);
#21859=ORIENTED_EDGE('',*,*,#15370,.T.);
#21860=ORIENTED_EDGE('',*,*,#15371,.T.);
#21861=ORIENTED_EDGE('',*,*,#15372,.F.);
#21862=ORIENTED_EDGE('',*,*,#15371,.F.);
#21863=ORIENTED_EDGE('',*,*,#15373,.T.);
#21864=ORIENTED_EDGE('',*,*,#15374,.F.);
#21865=ORIENTED_EDGE('',*,*,#15375,.F.);
#21866=ORIENTED_EDGE('',*,*,#15376,.F.);
#21867=ORIENTED_EDGE('',*,*,#15373,.F.);
#21868=ORIENTED_EDGE('',*,*,#15370,.F.);
#21869=ORIENTED_EDGE('',*,*,#15377,.F.);
#21870=ORIENTED_EDGE('',*,*,#15378,.T.);
#21871=ORIENTED_EDGE('',*,*,#15379,.T.);
#21872=ORIENTED_EDGE('',*,*,#15380,.F.);
#21873=ORIENTED_EDGE('',*,*,#15379,.F.);
#21874=ORIENTED_EDGE('',*,*,#15381,.T.);
#21875=ORIENTED_EDGE('',*,*,#15382,.F.);
#21876=ORIENTED_EDGE('',*,*,#15383,.F.);
#21877=ORIENTED_EDGE('',*,*,#15384,.F.);
#21878=ORIENTED_EDGE('',*,*,#15381,.F.);
#21879=ORIENTED_EDGE('',*,*,#15378,.F.);
#21880=ORIENTED_EDGE('',*,*,#15385,.F.);
#21881=ORIENTED_EDGE('',*,*,#15386,.T.);
#21882=ORIENTED_EDGE('',*,*,#15387,.T.);
#21883=ORIENTED_EDGE('',*,*,#15388,.F.);
#21884=ORIENTED_EDGE('',*,*,#15387,.F.);
#21885=ORIENTED_EDGE('',*,*,#15389,.T.);
#21886=ORIENTED_EDGE('',*,*,#15390,.F.);
#21887=ORIENTED_EDGE('',*,*,#15391,.F.);
#21888=ORIENTED_EDGE('',*,*,#15392,.F.);
#21889=ORIENTED_EDGE('',*,*,#15389,.F.);
#21890=ORIENTED_EDGE('',*,*,#15386,.F.);
#21891=ORIENTED_EDGE('',*,*,#15393,.F.);
#21892=ORIENTED_EDGE('',*,*,#15394,.T.);
#21893=ORIENTED_EDGE('',*,*,#15395,.T.);
#21894=ORIENTED_EDGE('',*,*,#15396,.F.);
#21895=ORIENTED_EDGE('',*,*,#15395,.F.);
#21896=ORIENTED_EDGE('',*,*,#15397,.T.);
#21897=ORIENTED_EDGE('',*,*,#15398,.F.);
#21898=ORIENTED_EDGE('',*,*,#15399,.F.);
#21899=ORIENTED_EDGE('',*,*,#15400,.F.);
#21900=ORIENTED_EDGE('',*,*,#15397,.F.);
#21901=ORIENTED_EDGE('',*,*,#15394,.F.);
#21902=ORIENTED_EDGE('',*,*,#15401,.F.);
#21903=ORIENTED_EDGE('',*,*,#15402,.T.);
#21904=ORIENTED_EDGE('',*,*,#15403,.T.);
#21905=ORIENTED_EDGE('',*,*,#15404,.F.);
#21906=ORIENTED_EDGE('',*,*,#15403,.F.);
#21907=ORIENTED_EDGE('',*,*,#15405,.T.);
#21908=ORIENTED_EDGE('',*,*,#15406,.F.);
#21909=ORIENTED_EDGE('',*,*,#15407,.F.);
#21910=ORIENTED_EDGE('',*,*,#15408,.F.);
#21911=ORIENTED_EDGE('',*,*,#15405,.F.);
#21912=ORIENTED_EDGE('',*,*,#15402,.F.);
#21913=ORIENTED_EDGE('',*,*,#15409,.F.);
#21914=ORIENTED_EDGE('',*,*,#15410,.T.);
#21915=ORIENTED_EDGE('',*,*,#15411,.T.);
#21916=ORIENTED_EDGE('',*,*,#15412,.F.);
#21917=ORIENTED_EDGE('',*,*,#15413,.F.);
#21918=ORIENTED_EDGE('',*,*,#15411,.F.);
#21919=ORIENTED_EDGE('',*,*,#15414,.T.);
#21920=ORIENTED_EDGE('',*,*,#15415,.F.);
#21921=ORIENTED_EDGE('',*,*,#15416,.F.);
#21922=ORIENTED_EDGE('',*,*,#15417,.F.);
#21923=ORIENTED_EDGE('',*,*,#15414,.F.);
#21924=ORIENTED_EDGE('',*,*,#15410,.F.);
#21925=ORIENTED_EDGE('',*,*,#15418,.F.);
#21926=ORIENTED_EDGE('',*,*,#15419,.T.);
#21927=ORIENTED_EDGE('',*,*,#15420,.T.);
#21928=ORIENTED_EDGE('',*,*,#15421,.F.);
#21929=ORIENTED_EDGE('',*,*,#15420,.F.);
#21930=ORIENTED_EDGE('',*,*,#15422,.T.);
#21931=ORIENTED_EDGE('',*,*,#15423,.F.);
#21932=ORIENTED_EDGE('',*,*,#15424,.F.);
#21933=ORIENTED_EDGE('',*,*,#15425,.F.);
#21934=ORIENTED_EDGE('',*,*,#15422,.F.);
#21935=ORIENTED_EDGE('',*,*,#15419,.F.);
#21936=ORIENTED_EDGE('',*,*,#15426,.F.);
#21937=ORIENTED_EDGE('',*,*,#15427,.T.);
#21938=ORIENTED_EDGE('',*,*,#15428,.T.);
#21939=ORIENTED_EDGE('',*,*,#15429,.F.);
#21940=ORIENTED_EDGE('',*,*,#15428,.F.);
#21941=ORIENTED_EDGE('',*,*,#15430,.T.);
#21942=ORIENTED_EDGE('',*,*,#15431,.F.);
#21943=ORIENTED_EDGE('',*,*,#15432,.F.);
#21944=ORIENTED_EDGE('',*,*,#15433,.F.);
#21945=ORIENTED_EDGE('',*,*,#15430,.F.);
#21946=ORIENTED_EDGE('',*,*,#15427,.F.);
#21947=ORIENTED_EDGE('',*,*,#15434,.F.);
#21948=ORIENTED_EDGE('',*,*,#15435,.T.);
#21949=ORIENTED_EDGE('',*,*,#15436,.T.);
#21950=ORIENTED_EDGE('',*,*,#15437,.F.);
#21951=ORIENTED_EDGE('',*,*,#15436,.F.);
#21952=ORIENTED_EDGE('',*,*,#15438,.T.);
#21953=ORIENTED_EDGE('',*,*,#15439,.F.);
#21954=ORIENTED_EDGE('',*,*,#15440,.F.);
#21955=ORIENTED_EDGE('',*,*,#15441,.F.);
#21956=ORIENTED_EDGE('',*,*,#15438,.F.);
#21957=ORIENTED_EDGE('',*,*,#15435,.F.);
#21958=ORIENTED_EDGE('',*,*,#15442,.F.);
#21959=ORIENTED_EDGE('',*,*,#15443,.T.);
#21960=ORIENTED_EDGE('',*,*,#15444,.T.);
#21961=ORIENTED_EDGE('',*,*,#15445,.F.);
#21962=ORIENTED_EDGE('',*,*,#15444,.F.);
#21963=ORIENTED_EDGE('',*,*,#15446,.T.);
#21964=ORIENTED_EDGE('',*,*,#15447,.F.);
#21965=ORIENTED_EDGE('',*,*,#15448,.F.);
#21966=ORIENTED_EDGE('',*,*,#15449,.F.);
#21967=ORIENTED_EDGE('',*,*,#15446,.F.);
#21968=ORIENTED_EDGE('',*,*,#15443,.F.);
#21969=ORIENTED_EDGE('',*,*,#15450,.F.);
#21970=ORIENTED_EDGE('',*,*,#15451,.T.);
#21971=ORIENTED_EDGE('',*,*,#15452,.T.);
#21972=ORIENTED_EDGE('',*,*,#15453,.F.);
#21973=ORIENTED_EDGE('',*,*,#15452,.F.);
#21974=ORIENTED_EDGE('',*,*,#15454,.T.);
#21975=ORIENTED_EDGE('',*,*,#15455,.F.);
#21976=ORIENTED_EDGE('',*,*,#15456,.F.);
#21977=ORIENTED_EDGE('',*,*,#15457,.F.);
#21978=ORIENTED_EDGE('',*,*,#15454,.F.);
#21979=ORIENTED_EDGE('',*,*,#15451,.F.);
#21980=ORIENTED_EDGE('',*,*,#15458,.F.);
#21981=ORIENTED_EDGE('',*,*,#15459,.T.);
#21982=ORIENTED_EDGE('',*,*,#15460,.T.);
#21983=ORIENTED_EDGE('',*,*,#15461,.F.);
#21984=ORIENTED_EDGE('',*,*,#15460,.F.);
#21985=ORIENTED_EDGE('',*,*,#15462,.T.);
#21986=ORIENTED_EDGE('',*,*,#15463,.F.);
#21987=ORIENTED_EDGE('',*,*,#15464,.F.);
#21988=ORIENTED_EDGE('',*,*,#15465,.F.);
#21989=ORIENTED_EDGE('',*,*,#15462,.F.);
#21990=ORIENTED_EDGE('',*,*,#15459,.F.);
#21991=ORIENTED_EDGE('',*,*,#15466,.F.);
#21992=ORIENTED_EDGE('',*,*,#15467,.T.);
#21993=ORIENTED_EDGE('',*,*,#15468,.T.);
#21994=ORIENTED_EDGE('',*,*,#15469,.F.);
#21995=ORIENTED_EDGE('',*,*,#15468,.F.);
#21996=ORIENTED_EDGE('',*,*,#15470,.T.);
#21997=ORIENTED_EDGE('',*,*,#15471,.F.);
#21998=ORIENTED_EDGE('',*,*,#15472,.F.);
#21999=ORIENTED_EDGE('',*,*,#15473,.F.);
#22000=ORIENTED_EDGE('',*,*,#15470,.F.);
#22001=ORIENTED_EDGE('',*,*,#15467,.F.);
#22002=ORIENTED_EDGE('',*,*,#15474,.F.);
#22003=ORIENTED_EDGE('',*,*,#15475,.T.);
#22004=ORIENTED_EDGE('',*,*,#15476,.T.);
#22005=ORIENTED_EDGE('',*,*,#15477,.F.);
#22006=ORIENTED_EDGE('',*,*,#15476,.F.);
#22007=ORIENTED_EDGE('',*,*,#15478,.T.);
#22008=ORIENTED_EDGE('',*,*,#15479,.F.);
#22009=ORIENTED_EDGE('',*,*,#15480,.F.);
#22010=ORIENTED_EDGE('',*,*,#15481,.F.);
#22011=ORIENTED_EDGE('',*,*,#15478,.F.);
#22012=ORIENTED_EDGE('',*,*,#15475,.F.);
#22013=ORIENTED_EDGE('',*,*,#15482,.F.);
#22014=ORIENTED_EDGE('',*,*,#15483,.T.);
#22015=ORIENTED_EDGE('',*,*,#15484,.T.);
#22016=ORIENTED_EDGE('',*,*,#15485,.F.);
#22017=ORIENTED_EDGE('',*,*,#15484,.F.);
#22018=ORIENTED_EDGE('',*,*,#15486,.T.);
#22019=ORIENTED_EDGE('',*,*,#15487,.F.);
#22020=ORIENTED_EDGE('',*,*,#15488,.F.);
#22021=ORIENTED_EDGE('',*,*,#15489,.F.);
#22022=ORIENTED_EDGE('',*,*,#15486,.F.);
#22023=ORIENTED_EDGE('',*,*,#15483,.F.);
#22024=ORIENTED_EDGE('',*,*,#15490,.F.);
#22025=ORIENTED_EDGE('',*,*,#15491,.T.);
#22026=ORIENTED_EDGE('',*,*,#15492,.T.);
#22027=ORIENTED_EDGE('',*,*,#15493,.F.);
#22028=ORIENTED_EDGE('',*,*,#15492,.F.);
#22029=ORIENTED_EDGE('',*,*,#15494,.T.);
#22030=ORIENTED_EDGE('',*,*,#15495,.F.);
#22031=ORIENTED_EDGE('',*,*,#15496,.F.);
#22032=ORIENTED_EDGE('',*,*,#15497,.F.);
#22033=ORIENTED_EDGE('',*,*,#15494,.F.);
#22034=ORIENTED_EDGE('',*,*,#15491,.F.);
#22035=ORIENTED_EDGE('',*,*,#15498,.F.);
#22036=ORIENTED_EDGE('',*,*,#15499,.T.);
#22037=ORIENTED_EDGE('',*,*,#15500,.T.);
#22038=ORIENTED_EDGE('',*,*,#15501,.F.);
#22039=ORIENTED_EDGE('',*,*,#15500,.F.);
#22040=ORIENTED_EDGE('',*,*,#15502,.T.);
#22041=ORIENTED_EDGE('',*,*,#15503,.F.);
#22042=ORIENTED_EDGE('',*,*,#15504,.F.);
#22043=ORIENTED_EDGE('',*,*,#15505,.F.);
#22044=ORIENTED_EDGE('',*,*,#15502,.F.);
#22045=ORIENTED_EDGE('',*,*,#15499,.F.);
#22046=ORIENTED_EDGE('',*,*,#15506,.F.);
#22047=ORIENTED_EDGE('',*,*,#15507,.T.);
#22048=ORIENTED_EDGE('',*,*,#15508,.T.);
#22049=ORIENTED_EDGE('',*,*,#15509,.F.);
#22050=ORIENTED_EDGE('',*,*,#15508,.F.);
#22051=ORIENTED_EDGE('',*,*,#15510,.T.);
#22052=ORIENTED_EDGE('',*,*,#15511,.F.);
#22053=ORIENTED_EDGE('',*,*,#15512,.F.);
#22054=ORIENTED_EDGE('',*,*,#15513,.F.);
#22055=ORIENTED_EDGE('',*,*,#15510,.F.);
#22056=ORIENTED_EDGE('',*,*,#15507,.F.);
#22057=ORIENTED_EDGE('',*,*,#15514,.F.);
#22058=ORIENTED_EDGE('',*,*,#15515,.T.);
#22059=ORIENTED_EDGE('',*,*,#15516,.T.);
#22060=ORIENTED_EDGE('',*,*,#15517,.F.);
#22061=ORIENTED_EDGE('',*,*,#15516,.F.);
#22062=ORIENTED_EDGE('',*,*,#15518,.T.);
#22063=ORIENTED_EDGE('',*,*,#15519,.F.);
#22064=ORIENTED_EDGE('',*,*,#15520,.F.);
#22065=ORIENTED_EDGE('',*,*,#15521,.F.);
#22066=ORIENTED_EDGE('',*,*,#15518,.F.);
#22067=ORIENTED_EDGE('',*,*,#15515,.F.);
#22068=ORIENTED_EDGE('',*,*,#15522,.F.);
#22069=ORIENTED_EDGE('',*,*,#15523,.T.);
#22070=ORIENTED_EDGE('',*,*,#15524,.T.);
#22071=ORIENTED_EDGE('',*,*,#15525,.F.);
#22072=ORIENTED_EDGE('',*,*,#15524,.F.);
#22073=ORIENTED_EDGE('',*,*,#15526,.T.);
#22074=ORIENTED_EDGE('',*,*,#15527,.F.);
#22075=ORIENTED_EDGE('',*,*,#15528,.F.);
#22076=ORIENTED_EDGE('',*,*,#15529,.F.);
#22077=ORIENTED_EDGE('',*,*,#15526,.F.);
#22078=ORIENTED_EDGE('',*,*,#15523,.F.);
#22079=ORIENTED_EDGE('',*,*,#15530,.F.);
#22080=ORIENTED_EDGE('',*,*,#15531,.T.);
#22081=ORIENTED_EDGE('',*,*,#15532,.T.);
#22082=ORIENTED_EDGE('',*,*,#15533,.F.);
#22083=ORIENTED_EDGE('',*,*,#15532,.F.);
#22084=ORIENTED_EDGE('',*,*,#15534,.T.);
#22085=ORIENTED_EDGE('',*,*,#15535,.F.);
#22086=ORIENTED_EDGE('',*,*,#15536,.F.);
#22087=ORIENTED_EDGE('',*,*,#15537,.F.);
#22088=ORIENTED_EDGE('',*,*,#15534,.F.);
#22089=ORIENTED_EDGE('',*,*,#15531,.F.);
#22090=ORIENTED_EDGE('',*,*,#15538,.F.);
#22091=ORIENTED_EDGE('',*,*,#15539,.T.);
#22092=ORIENTED_EDGE('',*,*,#15540,.T.);
#22093=ORIENTED_EDGE('',*,*,#15541,.F.);
#22094=ORIENTED_EDGE('',*,*,#15540,.F.);
#22095=ORIENTED_EDGE('',*,*,#15542,.T.);
#22096=ORIENTED_EDGE('',*,*,#15543,.F.);
#22097=ORIENTED_EDGE('',*,*,#15544,.F.);
#22098=ORIENTED_EDGE('',*,*,#15545,.F.);
#22099=ORIENTED_EDGE('',*,*,#15542,.F.);
#22100=ORIENTED_EDGE('',*,*,#15539,.F.);
#22101=ORIENTED_EDGE('',*,*,#15546,.F.);
#22102=ORIENTED_EDGE('',*,*,#15547,.T.);
#22103=ORIENTED_EDGE('',*,*,#15548,.T.);
#22104=ORIENTED_EDGE('',*,*,#15549,.F.);
#22105=ORIENTED_EDGE('',*,*,#15548,.F.);
#22106=ORIENTED_EDGE('',*,*,#15550,.T.);
#22107=ORIENTED_EDGE('',*,*,#15551,.F.);
#22108=ORIENTED_EDGE('',*,*,#15552,.F.);
#22109=ORIENTED_EDGE('',*,*,#15553,.F.);
#22110=ORIENTED_EDGE('',*,*,#15550,.F.);
#22111=ORIENTED_EDGE('',*,*,#15547,.F.);
#22112=ORIENTED_EDGE('',*,*,#15279,.T.);
#22113=ORIENTED_EDGE('',*,*,#15273,.T.);
#22114=ORIENTED_EDGE('',*,*,#15276,.T.);
#22115=ORIENTED_EDGE('',*,*,#15554,.F.);
#22116=ORIENTED_EDGE('',*,*,#15287,.T.);
#22117=ORIENTED_EDGE('',*,*,#15281,.T.);
#22118=ORIENTED_EDGE('',*,*,#15284,.T.);
#22119=ORIENTED_EDGE('',*,*,#15555,.F.);
#22120=ORIENTED_EDGE('',*,*,#15295,.T.);
#22121=ORIENTED_EDGE('',*,*,#15289,.T.);
#22122=ORIENTED_EDGE('',*,*,#15292,.T.);
#22123=ORIENTED_EDGE('',*,*,#15556,.F.);
#22124=ORIENTED_EDGE('',*,*,#15303,.T.);
#22125=ORIENTED_EDGE('',*,*,#15297,.T.);
#22126=ORIENTED_EDGE('',*,*,#15300,.T.);
#22127=ORIENTED_EDGE('',*,*,#15557,.F.);
#22128=ORIENTED_EDGE('',*,*,#15311,.T.);
#22129=ORIENTED_EDGE('',*,*,#15305,.T.);
#22130=ORIENTED_EDGE('',*,*,#15308,.T.);
#22131=ORIENTED_EDGE('',*,*,#15558,.F.);
#22132=ORIENTED_EDGE('',*,*,#15319,.T.);
#22133=ORIENTED_EDGE('',*,*,#15313,.T.);
#22134=ORIENTED_EDGE('',*,*,#15316,.T.);
#22135=ORIENTED_EDGE('',*,*,#15559,.F.);
#22136=ORIENTED_EDGE('',*,*,#15327,.T.);
#22137=ORIENTED_EDGE('',*,*,#15321,.T.);
#22138=ORIENTED_EDGE('',*,*,#15324,.T.);
#22139=ORIENTED_EDGE('',*,*,#15560,.F.);
#22140=ORIENTED_EDGE('',*,*,#15335,.T.);
#22141=ORIENTED_EDGE('',*,*,#15329,.T.);
#22142=ORIENTED_EDGE('',*,*,#15332,.T.);
#22143=ORIENTED_EDGE('',*,*,#15561,.F.);
#22144=ORIENTED_EDGE('',*,*,#15343,.T.);
#22145=ORIENTED_EDGE('',*,*,#15337,.T.);
#22146=ORIENTED_EDGE('',*,*,#15340,.T.);
#22147=ORIENTED_EDGE('',*,*,#15562,.F.);
#22148=ORIENTED_EDGE('',*,*,#15351,.T.);
#22149=ORIENTED_EDGE('',*,*,#15345,.T.);
#22150=ORIENTED_EDGE('',*,*,#15348,.T.);
#22151=ORIENTED_EDGE('',*,*,#15563,.F.);
#22152=ORIENTED_EDGE('',*,*,#15359,.T.);
#22153=ORIENTED_EDGE('',*,*,#15353,.T.);
#22154=ORIENTED_EDGE('',*,*,#15356,.T.);
#22155=ORIENTED_EDGE('',*,*,#15564,.F.);
#22156=ORIENTED_EDGE('',*,*,#15367,.T.);
#22157=ORIENTED_EDGE('',*,*,#15361,.T.);
#22158=ORIENTED_EDGE('',*,*,#15364,.T.);
#22159=ORIENTED_EDGE('',*,*,#15565,.F.);
#22160=ORIENTED_EDGE('',*,*,#15375,.T.);
#22161=ORIENTED_EDGE('',*,*,#15369,.T.);
#22162=ORIENTED_EDGE('',*,*,#15372,.T.);
#22163=ORIENTED_EDGE('',*,*,#15566,.F.);
#22164=ORIENTED_EDGE('',*,*,#15383,.T.);
#22165=ORIENTED_EDGE('',*,*,#15377,.T.);
#22166=ORIENTED_EDGE('',*,*,#15380,.T.);
#22167=ORIENTED_EDGE('',*,*,#15567,.F.);
#22168=ORIENTED_EDGE('',*,*,#15391,.T.);
#22169=ORIENTED_EDGE('',*,*,#15385,.T.);
#22170=ORIENTED_EDGE('',*,*,#15388,.T.);
#22171=ORIENTED_EDGE('',*,*,#15568,.F.);
#22172=ORIENTED_EDGE('',*,*,#15399,.T.);
#22173=ORIENTED_EDGE('',*,*,#15393,.T.);
#22174=ORIENTED_EDGE('',*,*,#15396,.T.);
#22175=ORIENTED_EDGE('',*,*,#15569,.F.);
#22176=ORIENTED_EDGE('',*,*,#15407,.T.);
#22177=ORIENTED_EDGE('',*,*,#15401,.T.);
#22178=ORIENTED_EDGE('',*,*,#15404,.T.);
#22179=ORIENTED_EDGE('',*,*,#15570,.F.);
#22180=ORIENTED_EDGE('',*,*,#15416,.T.);
#22181=ORIENTED_EDGE('',*,*,#15409,.T.);
#22182=ORIENTED_EDGE('',*,*,#15571,.T.);
#22183=ORIENTED_EDGE('',*,*,#15572,.T.);
#22184=ORIENTED_EDGE('',*,*,#15571,.F.);
#22185=ORIENTED_EDGE('',*,*,#15412,.T.);
#22186=ORIENTED_EDGE('',*,*,#15413,.T.);
#22187=ORIENTED_EDGE('',*,*,#15573,.F.);
#22188=ORIENTED_EDGE('',*,*,#15424,.T.);
#22189=ORIENTED_EDGE('',*,*,#15418,.T.);
#22190=ORIENTED_EDGE('',*,*,#15421,.T.);
#22191=ORIENTED_EDGE('',*,*,#15574,.F.);
#22192=ORIENTED_EDGE('',*,*,#15432,.T.);
#22193=ORIENTED_EDGE('',*,*,#15426,.T.);
#22194=ORIENTED_EDGE('',*,*,#15429,.T.);
#22195=ORIENTED_EDGE('',*,*,#15575,.F.);
#22196=ORIENTED_EDGE('',*,*,#15440,.T.);
#22197=ORIENTED_EDGE('',*,*,#15434,.T.);
#22198=ORIENTED_EDGE('',*,*,#15437,.T.);
#22199=ORIENTED_EDGE('',*,*,#15576,.F.);
#22200=ORIENTED_EDGE('',*,*,#15448,.T.);
#22201=ORIENTED_EDGE('',*,*,#15442,.T.);
#22202=ORIENTED_EDGE('',*,*,#15445,.T.);
#22203=ORIENTED_EDGE('',*,*,#15577,.F.);
#22204=ORIENTED_EDGE('',*,*,#15456,.T.);
#22205=ORIENTED_EDGE('',*,*,#15450,.T.);
#22206=ORIENTED_EDGE('',*,*,#15453,.T.);
#22207=ORIENTED_EDGE('',*,*,#15578,.F.);
#22208=ORIENTED_EDGE('',*,*,#15464,.T.);
#22209=ORIENTED_EDGE('',*,*,#15458,.T.);
#22210=ORIENTED_EDGE('',*,*,#15461,.T.);
#22211=ORIENTED_EDGE('',*,*,#15579,.F.);
#22212=ORIENTED_EDGE('',*,*,#15472,.T.);
#22213=ORIENTED_EDGE('',*,*,#15466,.T.);
#22214=ORIENTED_EDGE('',*,*,#15469,.T.);
#22215=ORIENTED_EDGE('',*,*,#15580,.F.);
#22216=ORIENTED_EDGE('',*,*,#15480,.T.);
#22217=ORIENTED_EDGE('',*,*,#15474,.T.);
#22218=ORIENTED_EDGE('',*,*,#15477,.T.);
#22219=ORIENTED_EDGE('',*,*,#15581,.F.);
#22220=ORIENTED_EDGE('',*,*,#15488,.T.);
#22221=ORIENTED_EDGE('',*,*,#15482,.T.);
#22222=ORIENTED_EDGE('',*,*,#15485,.T.);
#22223=ORIENTED_EDGE('',*,*,#15582,.F.);
#22224=ORIENTED_EDGE('',*,*,#15496,.T.);
#22225=ORIENTED_EDGE('',*,*,#15490,.T.);
#22226=ORIENTED_EDGE('',*,*,#15493,.T.);
#22227=ORIENTED_EDGE('',*,*,#15583,.F.);
#22228=ORIENTED_EDGE('',*,*,#15504,.T.);
#22229=ORIENTED_EDGE('',*,*,#15498,.T.);
#22230=ORIENTED_EDGE('',*,*,#15501,.T.);
#22231=ORIENTED_EDGE('',*,*,#15584,.F.);
#22232=ORIENTED_EDGE('',*,*,#15512,.T.);
#22233=ORIENTED_EDGE('',*,*,#15506,.T.);
#22234=ORIENTED_EDGE('',*,*,#15509,.T.);
#22235=ORIENTED_EDGE('',*,*,#15585,.F.);
#22236=ORIENTED_EDGE('',*,*,#15520,.T.);
#22237=ORIENTED_EDGE('',*,*,#15514,.T.);
#22238=ORIENTED_EDGE('',*,*,#15517,.T.);
#22239=ORIENTED_EDGE('',*,*,#15586,.F.);
#22240=ORIENTED_EDGE('',*,*,#15528,.T.);
#22241=ORIENTED_EDGE('',*,*,#15522,.T.);
#22242=ORIENTED_EDGE('',*,*,#15525,.T.);
#22243=ORIENTED_EDGE('',*,*,#15587,.F.);
#22244=ORIENTED_EDGE('',*,*,#15536,.T.);
#22245=ORIENTED_EDGE('',*,*,#15530,.T.);
#22246=ORIENTED_EDGE('',*,*,#15533,.T.);
#22247=ORIENTED_EDGE('',*,*,#15588,.F.);
#22248=ORIENTED_EDGE('',*,*,#15544,.T.);
#22249=ORIENTED_EDGE('',*,*,#15538,.T.);
#22250=ORIENTED_EDGE('',*,*,#15541,.T.);
#22251=ORIENTED_EDGE('',*,*,#15589,.F.);
#22252=ORIENTED_EDGE('',*,*,#15552,.T.);
#22253=ORIENTED_EDGE('',*,*,#15546,.T.);
#22254=ORIENTED_EDGE('',*,*,#15549,.T.);
#22255=ORIENTED_EDGE('',*,*,#15590,.F.);
#22256=ORIENTED_EDGE('',*,*,#15591,.T.);
#22257=ORIENTED_EDGE('',*,*,#15592,.T.);
#22258=ORIENTED_EDGE('',*,*,#15593,.T.);
#22259=ORIENTED_EDGE('',*,*,#15594,.F.);
#22260=ORIENTED_EDGE('',*,*,#15593,.F.);
#22261=ORIENTED_EDGE('',*,*,#15595,.F.);
#22262=ORIENTED_EDGE('',*,*,#15596,.T.);
#22263=ORIENTED_EDGE('',*,*,#15597,.F.);
#22264=ORIENTED_EDGE('',*,*,#15598,.F.);
#22265=ORIENTED_EDGE('',*,*,#15596,.F.);
#22266=ORIENTED_EDGE('',*,*,#15599,.F.);
#22267=ORIENTED_EDGE('',*,*,#15591,.F.);
#22268=ORIENTED_EDGE('',*,*,#15592,.F.);
#22269=ORIENTED_EDGE('',*,*,#15599,.T.);
#22270=ORIENTED_EDGE('',*,*,#15595,.T.);
#22271=ORIENTED_EDGE('',*,*,#15600,.F.);
#22272=ORIENTED_EDGE('',*,*,#15601,.T.);
#22273=ORIENTED_EDGE('',*,*,#15417,.T.);
#22274=ORIENTED_EDGE('',*,*,#15570,.T.);
#22275=ORIENTED_EDGE('',*,*,#15406,.T.);
#22276=ORIENTED_EDGE('',*,*,#15408,.T.);
#22277=ORIENTED_EDGE('',*,*,#15569,.T.);
#22278=ORIENTED_EDGE('',*,*,#15398,.T.);
#22279=ORIENTED_EDGE('',*,*,#15400,.T.);
#22280=ORIENTED_EDGE('',*,*,#15568,.T.);
#22281=ORIENTED_EDGE('',*,*,#15390,.T.);
#22282=ORIENTED_EDGE('',*,*,#15392,.T.);
#22283=ORIENTED_EDGE('',*,*,#15567,.T.);
#22284=ORIENTED_EDGE('',*,*,#15382,.T.);
#22285=ORIENTED_EDGE('',*,*,#15384,.T.);
#22286=ORIENTED_EDGE('',*,*,#15566,.T.);
#22287=ORIENTED_EDGE('',*,*,#15374,.T.);
#22288=ORIENTED_EDGE('',*,*,#15376,.T.);
#22289=ORIENTED_EDGE('',*,*,#15565,.T.);
#22290=ORIENTED_EDGE('',*,*,#15366,.T.);
#22291=ORIENTED_EDGE('',*,*,#15368,.T.);
#22292=ORIENTED_EDGE('',*,*,#15564,.T.);
#22293=ORIENTED_EDGE('',*,*,#15358,.T.);
#22294=ORIENTED_EDGE('',*,*,#15360,.T.);
#22295=ORIENTED_EDGE('',*,*,#15563,.T.);
#22296=ORIENTED_EDGE('',*,*,#15350,.T.);
#22297=ORIENTED_EDGE('',*,*,#15352,.T.);
#22298=ORIENTED_EDGE('',*,*,#15562,.T.);
#22299=ORIENTED_EDGE('',*,*,#15342,.T.);
#22300=ORIENTED_EDGE('',*,*,#15344,.T.);
#22301=ORIENTED_EDGE('',*,*,#15561,.T.);
#22302=ORIENTED_EDGE('',*,*,#15334,.T.);
#22303=ORIENTED_EDGE('',*,*,#15336,.T.);
#22304=ORIENTED_EDGE('',*,*,#15560,.T.);
#22305=ORIENTED_EDGE('',*,*,#15326,.T.);
#22306=ORIENTED_EDGE('',*,*,#15328,.T.);
#22307=ORIENTED_EDGE('',*,*,#15559,.T.);
#22308=ORIENTED_EDGE('',*,*,#15318,.T.);
#22309=ORIENTED_EDGE('',*,*,#15320,.T.);
#22310=ORIENTED_EDGE('',*,*,#15558,.T.);
#22311=ORIENTED_EDGE('',*,*,#15310,.T.);
#22312=ORIENTED_EDGE('',*,*,#15312,.T.);
#22313=ORIENTED_EDGE('',*,*,#15557,.T.);
#22314=ORIENTED_EDGE('',*,*,#15302,.T.);
#22315=ORIENTED_EDGE('',*,*,#15304,.T.);
#22316=ORIENTED_EDGE('',*,*,#15556,.T.);
#22317=ORIENTED_EDGE('',*,*,#15294,.T.);
#22318=ORIENTED_EDGE('',*,*,#15296,.T.);
#22319=ORIENTED_EDGE('',*,*,#15555,.T.);
#22320=ORIENTED_EDGE('',*,*,#15286,.T.);
#22321=ORIENTED_EDGE('',*,*,#15288,.T.);
#22322=ORIENTED_EDGE('',*,*,#15554,.T.);
#22323=ORIENTED_EDGE('',*,*,#15278,.T.);
#22324=ORIENTED_EDGE('',*,*,#15280,.T.);
#22325=ORIENTED_EDGE('',*,*,#15594,.T.);
#22326=ORIENTED_EDGE('',*,*,#15597,.T.);
#22327=ORIENTED_EDGE('',*,*,#15598,.T.);
#22328=ORIENTED_EDGE('',*,*,#15590,.T.);
#22329=ORIENTED_EDGE('',*,*,#15551,.T.);
#22330=ORIENTED_EDGE('',*,*,#15553,.T.);
#22331=ORIENTED_EDGE('',*,*,#15589,.T.);
#22332=ORIENTED_EDGE('',*,*,#15543,.T.);
#22333=ORIENTED_EDGE('',*,*,#15545,.T.);
#22334=ORIENTED_EDGE('',*,*,#15588,.T.);
#22335=ORIENTED_EDGE('',*,*,#15535,.T.);
#22336=ORIENTED_EDGE('',*,*,#15537,.T.);
#22337=ORIENTED_EDGE('',*,*,#15587,.T.);
#22338=ORIENTED_EDGE('',*,*,#15527,.T.);
#22339=ORIENTED_EDGE('',*,*,#15529,.T.);
#22340=ORIENTED_EDGE('',*,*,#15586,.T.);
#22341=ORIENTED_EDGE('',*,*,#15519,.T.);
#22342=ORIENTED_EDGE('',*,*,#15521,.T.);
#22343=ORIENTED_EDGE('',*,*,#15585,.T.);
#22344=ORIENTED_EDGE('',*,*,#15511,.T.);
#22345=ORIENTED_EDGE('',*,*,#15513,.T.);
#22346=ORIENTED_EDGE('',*,*,#15584,.T.);
#22347=ORIENTED_EDGE('',*,*,#15503,.T.);
#22348=ORIENTED_EDGE('',*,*,#15505,.T.);
#22349=ORIENTED_EDGE('',*,*,#15583,.T.);
#22350=ORIENTED_EDGE('',*,*,#15495,.T.);
#22351=ORIENTED_EDGE('',*,*,#15497,.T.);
#22352=ORIENTED_EDGE('',*,*,#15582,.T.);
#22353=ORIENTED_EDGE('',*,*,#15487,.T.);
#22354=ORIENTED_EDGE('',*,*,#15489,.T.);
#22355=ORIENTED_EDGE('',*,*,#15581,.T.);
#22356=ORIENTED_EDGE('',*,*,#15479,.T.);
#22357=ORIENTED_EDGE('',*,*,#15481,.T.);
#22358=ORIENTED_EDGE('',*,*,#15580,.T.);
#22359=ORIENTED_EDGE('',*,*,#15471,.T.);
#22360=ORIENTED_EDGE('',*,*,#15473,.T.);
#22361=ORIENTED_EDGE('',*,*,#15579,.T.);
#22362=ORIENTED_EDGE('',*,*,#15463,.T.);
#22363=ORIENTED_EDGE('',*,*,#15465,.T.);
#22364=ORIENTED_EDGE('',*,*,#15578,.T.);
#22365=ORIENTED_EDGE('',*,*,#15455,.T.);
#22366=ORIENTED_EDGE('',*,*,#15457,.T.);
#22367=ORIENTED_EDGE('',*,*,#15577,.T.);
#22368=ORIENTED_EDGE('',*,*,#15447,.T.);
#22369=ORIENTED_EDGE('',*,*,#15449,.T.);
#22370=ORIENTED_EDGE('',*,*,#15576,.T.);
#22371=ORIENTED_EDGE('',*,*,#15439,.T.);
#22372=ORIENTED_EDGE('',*,*,#15441,.T.);
#22373=ORIENTED_EDGE('',*,*,#15575,.T.);
#22374=ORIENTED_EDGE('',*,*,#15431,.T.);
#22375=ORIENTED_EDGE('',*,*,#15433,.T.);
#22376=ORIENTED_EDGE('',*,*,#15574,.T.);
#22377=ORIENTED_EDGE('',*,*,#15423,.T.);
#22378=ORIENTED_EDGE('',*,*,#15425,.T.);
#22379=ORIENTED_EDGE('',*,*,#15573,.T.);
#22380=ORIENTED_EDGE('',*,*,#15415,.T.);
#22381=ORIENTED_EDGE('',*,*,#15601,.F.);
#22382=ORIENTED_EDGE('',*,*,#15602,.T.);
#22383=ORIENTED_EDGE('',*,*,#15603,.F.);
#22384=ORIENTED_EDGE('',*,*,#15602,.F.);
#22385=ORIENTED_EDGE('',*,*,#15604,.F.);
#22386=ORIENTED_EDGE('',*,*,#15605,.T.);
#22387=ORIENTED_EDGE('',*,*,#15606,.T.);
#22388=ORIENTED_EDGE('',*,*,#15607,.F.);
#22389=ORIENTED_EDGE('',*,*,#15608,.F.);
#22390=ORIENTED_EDGE('',*,*,#15609,.T.);
#22391=ORIENTED_EDGE('',*,*,#15610,.T.);
#22392=ORIENTED_EDGE('',*,*,#15605,.F.);
#22393=ORIENTED_EDGE('',*,*,#15611,.F.);
#22394=ORIENTED_EDGE('',*,*,#15612,.T.);
#22395=ORIENTED_EDGE('',*,*,#15613,.T.);
#22396=ORIENTED_EDGE('',*,*,#15609,.F.);
#22397=ORIENTED_EDGE('',*,*,#15614,.F.);
#22398=ORIENTED_EDGE('',*,*,#15615,.T.);
#22399=ORIENTED_EDGE('',*,*,#15616,.T.);
#22400=ORIENTED_EDGE('',*,*,#15612,.F.);
#22401=ORIENTED_EDGE('',*,*,#15617,.F.);
#22402=ORIENTED_EDGE('',*,*,#15618,.T.);
#22403=ORIENTED_EDGE('',*,*,#15619,.T.);
#22404=ORIENTED_EDGE('',*,*,#15615,.F.);
#22405=ORIENTED_EDGE('',*,*,#15620,.F.);
#22406=ORIENTED_EDGE('',*,*,#15607,.T.);
#22407=ORIENTED_EDGE('',*,*,#15621,.T.);
#22408=ORIENTED_EDGE('',*,*,#15618,.F.);
#22409=ORIENTED_EDGE('',*,*,#15621,.F.);
#22410=ORIENTED_EDGE('',*,*,#15606,.F.);
#22411=ORIENTED_EDGE('',*,*,#15610,.F.);
#22412=ORIENTED_EDGE('',*,*,#15613,.F.);
#22413=ORIENTED_EDGE('',*,*,#15616,.F.);
#22414=ORIENTED_EDGE('',*,*,#15619,.F.);
#22415=ORIENTED_EDGE('',*,*,#15603,.T.);
#22416=ORIENTED_EDGE('',*,*,#15622,.F.);
#22417=ORIENTED_EDGE('',*,*,#15188,.F.);
#22418=ORIENTED_EDGE('',*,*,#15623,.T.);
#22419=ORIENTED_EDGE('',*,*,#15622,.T.);
#22420=ORIENTED_EDGE('',*,*,#15623,.F.);
#22421=ORIENTED_EDGE('',*,*,#15624,.F.);
#22422=ORIENTED_EDGE('',*,*,#15625,.T.);
#22423=ORIENTED_EDGE('',*,*,#15263,.T.);
#22424=ORIENTED_EDGE('',*,*,#15272,.T.);
#22425=ORIENTED_EDGE('',*,*,#15264,.T.);
#22426=ORIENTED_EDGE('',*,*,#15625,.F.);
#22427=ORIENTED_EDGE('',*,*,#15572,.F.);
#22428=ORIENTED_EDGE('',*,*,#15624,.T.);
#22429=ORIENTED_EDGE('',*,*,#15600,.T.);
#22430=ORIENTED_EDGE('',*,*,#15604,.T.);
#22431=ORIENTED_EDGE('',*,*,#15620,.T.);
#22432=ORIENTED_EDGE('',*,*,#15617,.T.);
#22433=ORIENTED_EDGE('',*,*,#15614,.T.);
#22434=ORIENTED_EDGE('',*,*,#15611,.T.);
#22435=ORIENTED_EDGE('',*,*,#15608,.T.);
#22436=ORIENTED_EDGE('',*,*,#15626,.F.);
#22437=ORIENTED_EDGE('',*,*,#15627,.T.);
#22438=ORIENTED_EDGE('',*,*,#15628,.T.);
#22439=ORIENTED_EDGE('',*,*,#15629,.T.);
#22440=ORIENTED_EDGE('',*,*,#15630,.T.);
#22441=ORIENTED_EDGE('',*,*,#15629,.F.);
#22442=ORIENTED_EDGE('',*,*,#15631,.T.);
#22443=ORIENTED_EDGE('',*,*,#15632,.T.);
#22444=ORIENTED_EDGE('',*,*,#15633,.F.);
#22445=ORIENTED_EDGE('',*,*,#15634,.T.);
#22446=ORIENTED_EDGE('',*,*,#15626,.T.);
#22447=ORIENTED_EDGE('',*,*,#15635,.T.);
#22448=ORIENTED_EDGE('',*,*,#15636,.F.);
#22449=ORIENTED_EDGE('',*,*,#15637,.T.);
#22450=ORIENTED_EDGE('',*,*,#15633,.T.);
#22451=ORIENTED_EDGE('',*,*,#15638,.T.);
#22452=ORIENTED_EDGE('',*,*,#15639,.F.);
#22453=ORIENTED_EDGE('',*,*,#15640,.T.);
#22454=ORIENTED_EDGE('',*,*,#15636,.T.);
#22455=ORIENTED_EDGE('',*,*,#15641,.T.);
#22456=ORIENTED_EDGE('',*,*,#15642,.F.);
#22457=ORIENTED_EDGE('',*,*,#15643,.T.);
#22458=ORIENTED_EDGE('',*,*,#15639,.T.);
#22459=ORIENTED_EDGE('',*,*,#15644,.T.);
#22460=ORIENTED_EDGE('',*,*,#15645,.F.);
#22461=ORIENTED_EDGE('',*,*,#15646,.T.);
#22462=ORIENTED_EDGE('',*,*,#15642,.T.);
#22463=ORIENTED_EDGE('',*,*,#15647,.T.);
#22464=ORIENTED_EDGE('',*,*,#15648,.F.);
#22465=ORIENTED_EDGE('',*,*,#15649,.T.);
#22466=ORIENTED_EDGE('',*,*,#15645,.T.);
#22467=ORIENTED_EDGE('',*,*,#15650,.T.);
#22468=ORIENTED_EDGE('',*,*,#15651,.F.);
#22469=ORIENTED_EDGE('',*,*,#15652,.T.);
#22470=ORIENTED_EDGE('',*,*,#15653,.F.);
#22471=ORIENTED_EDGE('',*,*,#15654,.F.);
#22472=ORIENTED_EDGE('',*,*,#15655,.F.);
#22473=ORIENTED_EDGE('',*,*,#15656,.T.);
#22474=ORIENTED_EDGE('',*,*,#15651,.T.);
#22475=ORIENTED_EDGE('',*,*,#15657,.F.);
#22476=ORIENTED_EDGE('',*,*,#15658,.F.);
#22477=ORIENTED_EDGE('',*,*,#15659,.T.);
#22478=ORIENTED_EDGE('',*,*,#15655,.T.);
#22479=ORIENTED_EDGE('',*,*,#15660,.F.);
#22480=ORIENTED_EDGE('',*,*,#15661,.F.);
#22481=ORIENTED_EDGE('',*,*,#15662,.T.);
#22482=ORIENTED_EDGE('',*,*,#15658,.T.);
#22483=ORIENTED_EDGE('',*,*,#15663,.F.);
#22484=ORIENTED_EDGE('',*,*,#15664,.F.);
#22485=ORIENTED_EDGE('',*,*,#15665,.T.);
#22486=ORIENTED_EDGE('',*,*,#15661,.T.);
#22487=ORIENTED_EDGE('',*,*,#15666,.F.);
#22488=ORIENTED_EDGE('',*,*,#15667,.F.);
#22489=ORIENTED_EDGE('',*,*,#15668,.T.);
#22490=ORIENTED_EDGE('',*,*,#15664,.T.);
#22491=ORIENTED_EDGE('',*,*,#15669,.F.);
#22492=ORIENTED_EDGE('',*,*,#15670,.F.);
#22493=ORIENTED_EDGE('',*,*,#15671,.T.);
#22494=ORIENTED_EDGE('',*,*,#15667,.T.);
#22495=ORIENTED_EDGE('',*,*,#15672,.F.);
#22496=ORIENTED_EDGE('',*,*,#15673,.F.);
#22497=ORIENTED_EDGE('',*,*,#15674,.F.);
#22498=ORIENTED_EDGE('',*,*,#15675,.T.);
#22499=ORIENTED_EDGE('',*,*,#15670,.T.);
#22500=ORIENTED_EDGE('',*,*,#15676,.F.);
#22501=ORIENTED_EDGE('',*,*,#15677,.F.);
#22502=ORIENTED_EDGE('',*,*,#15678,.F.);
#22503=ORIENTED_EDGE('',*,*,#15650,.F.);
#22504=ORIENTED_EDGE('',*,*,#15647,.F.);
#22505=ORIENTED_EDGE('',*,*,#15644,.F.);
#22506=ORIENTED_EDGE('',*,*,#15641,.F.);
#22507=ORIENTED_EDGE('',*,*,#15638,.F.);
#22508=ORIENTED_EDGE('',*,*,#15635,.F.);
#22509=ORIENTED_EDGE('',*,*,#15632,.F.);
#22510=ORIENTED_EDGE('',*,*,#15679,.F.);
#22511=ORIENTED_EDGE('',*,*,#15680,.T.);
#22512=ORIENTED_EDGE('',*,*,#15676,.T.);
#22513=ORIENTED_EDGE('',*,*,#15672,.T.);
#22514=ORIENTED_EDGE('',*,*,#15669,.T.);
#22515=ORIENTED_EDGE('',*,*,#15666,.T.);
#22516=ORIENTED_EDGE('',*,*,#15663,.T.);
#22517=ORIENTED_EDGE('',*,*,#15660,.T.);
#22518=ORIENTED_EDGE('',*,*,#15657,.T.);
#22519=ORIENTED_EDGE('',*,*,#15654,.T.);
#22520=ORIENTED_EDGE('',*,*,#15628,.F.);
#22521=ORIENTED_EDGE('',*,*,#15681,.T.);
#22522=ORIENTED_EDGE('',*,*,#15674,.T.);
#22523=ORIENTED_EDGE('',*,*,#15682,.T.);
#22524=ORIENTED_EDGE('',*,*,#15679,.T.);
#22525=ORIENTED_EDGE('',*,*,#15631,.F.);
#22526=ORIENTED_EDGE('',*,*,#15673,.T.);
#22527=ORIENTED_EDGE('',*,*,#15680,.F.);
#22528=ORIENTED_EDGE('',*,*,#15682,.F.);
#22529=ORIENTED_EDGE('',*,*,#15683,.F.);
#22530=ORIENTED_EDGE('',*,*,#15652,.F.);
#22531=ORIENTED_EDGE('',*,*,#15656,.F.);
#22532=ORIENTED_EDGE('',*,*,#15659,.F.);
#22533=ORIENTED_EDGE('',*,*,#15662,.F.);
#22534=ORIENTED_EDGE('',*,*,#15665,.F.);
#22535=ORIENTED_EDGE('',*,*,#15668,.F.);
#22536=ORIENTED_EDGE('',*,*,#15671,.F.);
#22537=ORIENTED_EDGE('',*,*,#15675,.F.);
#22538=ORIENTED_EDGE('',*,*,#15681,.F.);
#22539=ORIENTED_EDGE('',*,*,#15627,.F.);
#22540=ORIENTED_EDGE('',*,*,#15634,.F.);
#22541=ORIENTED_EDGE('',*,*,#15637,.F.);
#22542=ORIENTED_EDGE('',*,*,#15640,.F.);
#22543=ORIENTED_EDGE('',*,*,#15643,.F.);
#22544=ORIENTED_EDGE('',*,*,#15646,.F.);
#22545=ORIENTED_EDGE('',*,*,#15649,.F.);
#22546=ORIENTED_EDGE('',*,*,#15684,.F.);
#22547=ORIENTED_EDGE('',*,*,#15685,.F.);
#22548=ORIENTED_EDGE('',*,*,#15686,.F.);
#22549=ORIENTED_EDGE('',*,*,#15687,.F.);
#22550=ORIENTED_EDGE('',*,*,#15688,.T.);
#22551=ORIENTED_EDGE('',*,*,#15689,.F.);
#22552=ORIENTED_EDGE('',*,*,#15690,.F.);
#22553=ORIENTED_EDGE('',*,*,#15691,.F.);
#22554=ORIENTED_EDGE('',*,*,#15692,.F.);
#22555=ORIENTED_EDGE('',*,*,#15693,.F.);
#22556=ORIENTED_EDGE('',*,*,#15694,.F.);
#22557=ORIENTED_EDGE('',*,*,#15695,.F.);
#22558=ORIENTED_EDGE('',*,*,#15696,.T.);
#22559=ORIENTED_EDGE('',*,*,#15697,.F.);
#22560=ORIENTED_EDGE('',*,*,#15688,.F.);
#22561=ORIENTED_EDGE('',*,*,#15698,.F.);
#22562=ORIENTED_EDGE('',*,*,#15699,.F.);
#22563=ORIENTED_EDGE('',*,*,#15700,.F.);
#22564=ORIENTED_EDGE('',*,*,#15696,.F.);
#22565=ORIENTED_EDGE('',*,*,#15701,.F.);
#22566=ORIENTED_EDGE('',*,*,#15690,.T.);
#22567=ORIENTED_EDGE('',*,*,#15702,.F.);
#22568=ORIENTED_EDGE('',*,*,#15703,.F.);
#22569=ORIENTED_EDGE('',*,*,#15704,.F.);
#22570=ORIENTED_EDGE('',*,*,#15686,.T.);
#22571=ORIENTED_EDGE('',*,*,#15705,.T.);
#22572=ORIENTED_EDGE('',*,*,#15702,.T.);
#22573=ORIENTED_EDGE('',*,*,#15685,.T.);
#22574=ORIENTED_EDGE('',*,*,#15697,.T.);
#22575=ORIENTED_EDGE('',*,*,#15706,.T.);
#22576=ORIENTED_EDGE('',*,*,#15707,.T.);
#22577=ORIENTED_EDGE('',*,*,#15708,.T.);
#22578=ORIENTED_EDGE('',*,*,#15693,.T.);
#22579=ORIENTED_EDGE('',*,*,#15700,.T.);
#22580=ORIENTED_EDGE('',*,*,#15689,.T.);
#22581=ORIENTED_EDGE('',*,*,#15709,.T.);
#22582=ORIENTED_EDGE('',*,*,#15710,.T.);
#22583=ORIENTED_EDGE('',*,*,#15711,.T.);
#22584=ORIENTED_EDGE('',*,*,#15699,.T.);
#22585=ORIENTED_EDGE('',*,*,#15712,.F.);
#22586=ORIENTED_EDGE('',*,*,#15713,.T.);
#22587=ORIENTED_EDGE('',*,*,#15706,.F.);
#22588=ORIENTED_EDGE('',*,*,#15694,.T.);
#22589=ORIENTED_EDGE('',*,*,#15708,.F.);
#22590=ORIENTED_EDGE('',*,*,#15714,.F.);
#22591=ORIENTED_EDGE('',*,*,#15715,.F.);
#22592=ORIENTED_EDGE('',*,*,#15692,.T.);
#22593=ORIENTED_EDGE('',*,*,#15716,.F.);
#22594=ORIENTED_EDGE('',*,*,#15717,.T.);
#22595=ORIENTED_EDGE('',*,*,#15709,.F.);
#22596=ORIENTED_EDGE('',*,*,#15703,.T.);
#22597=ORIENTED_EDGE('',*,*,#15711,.F.);
#22598=ORIENTED_EDGE('',*,*,#15718,.F.);
#22599=ORIENTED_EDGE('',*,*,#15719,.F.);
#22600=ORIENTED_EDGE('',*,*,#15707,.F.);
#22601=ORIENTED_EDGE('',*,*,#15713,.F.);
#22602=ORIENTED_EDGE('',*,*,#15720,.F.);
#22603=ORIENTED_EDGE('',*,*,#15714,.T.);
#22604=ORIENTED_EDGE('',*,*,#15710,.F.);
#22605=ORIENTED_EDGE('',*,*,#15717,.F.);
#22606=ORIENTED_EDGE('',*,*,#15721,.F.);
#22607=ORIENTED_EDGE('',*,*,#15718,.T.);
#22608=ORIENTED_EDGE('',*,*,#15719,.T.);
#22609=ORIENTED_EDGE('',*,*,#15721,.T.);
#22610=ORIENTED_EDGE('',*,*,#15716,.T.);
#22611=ORIENTED_EDGE('',*,*,#15691,.T.);
#22612=ORIENTED_EDGE('',*,*,#15701,.T.);
#22613=ORIENTED_EDGE('',*,*,#15695,.T.);
#22614=ORIENTED_EDGE('',*,*,#15715,.T.);
#22615=ORIENTED_EDGE('',*,*,#15720,.T.);
#22616=ORIENTED_EDGE('',*,*,#15712,.T.);
#22617=ORIENTED_EDGE('',*,*,#15698,.T.);
#22618=ORIENTED_EDGE('',*,*,#15687,.T.);
#22619=ORIENTED_EDGE('',*,*,#15704,.T.);
#22620=ORIENTED_EDGE('',*,*,#15722,.F.);
#22621=ORIENTED_EDGE('',*,*,#15630,.F.);
#22622=ORIENTED_EDGE('',*,*,#15723,.T.);
#22623=ORIENTED_EDGE('',*,*,#15722,.T.);
#22624=ORIENTED_EDGE('',*,*,#15723,.F.);
#22625=ORIENTED_EDGE('',*,*,#15648,.T.);
#22626=ORIENTED_EDGE('',*,*,#15678,.T.);
#22627=ORIENTED_EDGE('',*,*,#15724,.F.);
#22628=ORIENTED_EDGE('',*,*,#15684,.T.);
#22629=ORIENTED_EDGE('',*,*,#15725,.F.);
#22630=ORIENTED_EDGE('',*,*,#15724,.T.);
#22631=ORIENTED_EDGE('',*,*,#15677,.T.);
#22632=ORIENTED_EDGE('',*,*,#15653,.T.);
#22633=ORIENTED_EDGE('',*,*,#15683,.T.);
#22634=ORIENTED_EDGE('',*,*,#15726,.F.);
#22635=ORIENTED_EDGE('',*,*,#15727,.T.);
#22636=ORIENTED_EDGE('',*,*,#15725,.T.);
#22637=ORIENTED_EDGE('',*,*,#15727,.F.);
#22638=ORIENTED_EDGE('',*,*,#15705,.F.);
#22639=ORIENTED_EDGE('',*,*,#15728,.T.);
#22640=ORIENTED_EDGE('',*,*,#15726,.T.);
#22641=ORIENTED_EDGE('',*,*,#15728,.F.);
#22642=ORIENTED_EDGE('',*,*,#15729,.F.);
#22643=ORIENTED_EDGE('',*,*,#15730,.T.);
#22644=ORIENTED_EDGE('',*,*,#15731,.T.);
#22645=ORIENTED_EDGE('',*,*,#15732,.T.);
#22646=ORIENTED_EDGE('',*,*,#15733,.T.);
#22647=ORIENTED_EDGE('',*,*,#15732,.F.);
#22648=ORIENTED_EDGE('',*,*,#15734,.T.);
#22649=ORIENTED_EDGE('',*,*,#15735,.T.);
#22650=ORIENTED_EDGE('',*,*,#15736,.F.);
#22651=ORIENTED_EDGE('',*,*,#15737,.T.);
#22652=ORIENTED_EDGE('',*,*,#15729,.T.);
#22653=ORIENTED_EDGE('',*,*,#15738,.T.);
#22654=ORIENTED_EDGE('',*,*,#15739,.F.);
#22655=ORIENTED_EDGE('',*,*,#15740,.T.);
#22656=ORIENTED_EDGE('',*,*,#15736,.T.);
#22657=ORIENTED_EDGE('',*,*,#15741,.T.);
#22658=ORIENTED_EDGE('',*,*,#15742,.F.);
#22659=ORIENTED_EDGE('',*,*,#15743,.T.);
#22660=ORIENTED_EDGE('',*,*,#15739,.T.);
#22661=ORIENTED_EDGE('',*,*,#15744,.T.);
#22662=ORIENTED_EDGE('',*,*,#15745,.F.);
#22663=ORIENTED_EDGE('',*,*,#15746,.T.);
#22664=ORIENTED_EDGE('',*,*,#15742,.T.);
#22665=ORIENTED_EDGE('',*,*,#15747,.T.);
#22666=ORIENTED_EDGE('',*,*,#15748,.F.);
#22667=ORIENTED_EDGE('',*,*,#15749,.T.);
#22668=ORIENTED_EDGE('',*,*,#15745,.T.);
#22669=ORIENTED_EDGE('',*,*,#15750,.T.);
#22670=ORIENTED_EDGE('',*,*,#15751,.F.);
#22671=ORIENTED_EDGE('',*,*,#15752,.T.);
#22672=ORIENTED_EDGE('',*,*,#15748,.T.);
#22673=ORIENTED_EDGE('',*,*,#15753,.T.);
#22674=ORIENTED_EDGE('',*,*,#15754,.F.);
#22675=ORIENTED_EDGE('',*,*,#15755,.T.);
#22676=ORIENTED_EDGE('',*,*,#15751,.T.);
#22677=ORIENTED_EDGE('',*,*,#15756,.T.);
#22678=ORIENTED_EDGE('',*,*,#15757,.F.);
#22679=ORIENTED_EDGE('',*,*,#15758,.T.);
#22680=ORIENTED_EDGE('',*,*,#15754,.T.);
#22681=ORIENTED_EDGE('',*,*,#15759,.T.);
#22682=ORIENTED_EDGE('',*,*,#15760,.F.);
#22683=ORIENTED_EDGE('',*,*,#15761,.T.);
#22684=ORIENTED_EDGE('',*,*,#15757,.T.);
#22685=ORIENTED_EDGE('',*,*,#15762,.T.);
#22686=ORIENTED_EDGE('',*,*,#15763,.F.);
#22687=ORIENTED_EDGE('',*,*,#15764,.T.);
#22688=ORIENTED_EDGE('',*,*,#15760,.T.);
#22689=ORIENTED_EDGE('',*,*,#15765,.T.);
#22690=ORIENTED_EDGE('',*,*,#15766,.F.);
#22691=ORIENTED_EDGE('',*,*,#15767,.T.);
#22692=ORIENTED_EDGE('',*,*,#15763,.T.);
#22693=ORIENTED_EDGE('',*,*,#15768,.T.);
#22694=ORIENTED_EDGE('',*,*,#15769,.F.);
#22695=ORIENTED_EDGE('',*,*,#15770,.T.);
#22696=ORIENTED_EDGE('',*,*,#15766,.T.);
#22697=ORIENTED_EDGE('',*,*,#15771,.T.);
#22698=ORIENTED_EDGE('',*,*,#15772,.F.);
#22699=ORIENTED_EDGE('',*,*,#15773,.T.);
#22700=ORIENTED_EDGE('',*,*,#15769,.T.);
#22701=ORIENTED_EDGE('',*,*,#15774,.T.);
#22702=ORIENTED_EDGE('',*,*,#15775,.F.);
#22703=ORIENTED_EDGE('',*,*,#15776,.T.);
#22704=ORIENTED_EDGE('',*,*,#15772,.T.);
#22705=ORIENTED_EDGE('',*,*,#15777,.T.);
#22706=ORIENTED_EDGE('',*,*,#15778,.F.);
#22707=ORIENTED_EDGE('',*,*,#15779,.T.);
#22708=ORIENTED_EDGE('',*,*,#15775,.T.);
#22709=ORIENTED_EDGE('',*,*,#15780,.T.);
#22710=ORIENTED_EDGE('',*,*,#15781,.F.);
#22711=ORIENTED_EDGE('',*,*,#15782,.T.);
#22712=ORIENTED_EDGE('',*,*,#15783,.F.);
#22713=ORIENTED_EDGE('',*,*,#15784,.F.);
#22714=ORIENTED_EDGE('',*,*,#15785,.T.);
#22715=ORIENTED_EDGE('',*,*,#15781,.T.);
#22716=ORIENTED_EDGE('',*,*,#15786,.F.);
#22717=ORIENTED_EDGE('',*,*,#15787,.F.);
#22718=ORIENTED_EDGE('',*,*,#15788,.F.);
#22719=ORIENTED_EDGE('',*,*,#15789,.T.);
#22720=ORIENTED_EDGE('',*,*,#15784,.T.);
#22721=ORIENTED_EDGE('',*,*,#15790,.F.);
#22722=ORIENTED_EDGE('',*,*,#15791,.F.);
#22723=ORIENTED_EDGE('',*,*,#15792,.T.);
#22724=ORIENTED_EDGE('',*,*,#15788,.T.);
#22725=ORIENTED_EDGE('',*,*,#15793,.F.);
#22726=ORIENTED_EDGE('',*,*,#15794,.F.);
#22727=ORIENTED_EDGE('',*,*,#15795,.T.);
#22728=ORIENTED_EDGE('',*,*,#15791,.T.);
#22729=ORIENTED_EDGE('',*,*,#15796,.F.);
#22730=ORIENTED_EDGE('',*,*,#15797,.F.);
#22731=ORIENTED_EDGE('',*,*,#15798,.T.);
#22732=ORIENTED_EDGE('',*,*,#15794,.T.);
#22733=ORIENTED_EDGE('',*,*,#15799,.F.);
#22734=ORIENTED_EDGE('',*,*,#15800,.F.);
#22735=ORIENTED_EDGE('',*,*,#15801,.T.);
#22736=ORIENTED_EDGE('',*,*,#15797,.T.);
#22737=ORIENTED_EDGE('',*,*,#15802,.F.);
#22738=ORIENTED_EDGE('',*,*,#15803,.F.);
#22739=ORIENTED_EDGE('',*,*,#15804,.T.);
#22740=ORIENTED_EDGE('',*,*,#15800,.T.);
#22741=ORIENTED_EDGE('',*,*,#15805,.F.);
#22742=ORIENTED_EDGE('',*,*,#15806,.F.);
#22743=ORIENTED_EDGE('',*,*,#15807,.T.);
#22744=ORIENTED_EDGE('',*,*,#15803,.T.);
#22745=ORIENTED_EDGE('',*,*,#15808,.F.);
#22746=ORIENTED_EDGE('',*,*,#15809,.F.);
#22747=ORIENTED_EDGE('',*,*,#15810,.T.);
#22748=ORIENTED_EDGE('',*,*,#15806,.T.);
#22749=ORIENTED_EDGE('',*,*,#15811,.F.);
#22750=ORIENTED_EDGE('',*,*,#15812,.F.);
#22751=ORIENTED_EDGE('',*,*,#15813,.T.);
#22752=ORIENTED_EDGE('',*,*,#15809,.T.);
#22753=ORIENTED_EDGE('',*,*,#15814,.F.);
#22754=ORIENTED_EDGE('',*,*,#15815,.F.);
#22755=ORIENTED_EDGE('',*,*,#15816,.T.);
#22756=ORIENTED_EDGE('',*,*,#15812,.T.);
#22757=ORIENTED_EDGE('',*,*,#15817,.F.);
#22758=ORIENTED_EDGE('',*,*,#15818,.F.);
#22759=ORIENTED_EDGE('',*,*,#15819,.T.);
#22760=ORIENTED_EDGE('',*,*,#15815,.T.);
#22761=ORIENTED_EDGE('',*,*,#15820,.F.);
#22762=ORIENTED_EDGE('',*,*,#15821,.F.);
#22763=ORIENTED_EDGE('',*,*,#15822,.T.);
#22764=ORIENTED_EDGE('',*,*,#15818,.T.);
#22765=ORIENTED_EDGE('',*,*,#15823,.F.);
#22766=ORIENTED_EDGE('',*,*,#15824,.F.);
#22767=ORIENTED_EDGE('',*,*,#15825,.T.);
#22768=ORIENTED_EDGE('',*,*,#15821,.T.);
#22769=ORIENTED_EDGE('',*,*,#15826,.F.);
#22770=ORIENTED_EDGE('',*,*,#15827,.F.);
#22771=ORIENTED_EDGE('',*,*,#15828,.T.);
#22772=ORIENTED_EDGE('',*,*,#15824,.T.);
#22773=ORIENTED_EDGE('',*,*,#15829,.F.);
#22774=ORIENTED_EDGE('',*,*,#15830,.F.);
#22775=ORIENTED_EDGE('',*,*,#15831,.F.);
#22776=ORIENTED_EDGE('',*,*,#15832,.T.);
#22777=ORIENTED_EDGE('',*,*,#15827,.T.);
#22778=ORIENTED_EDGE('',*,*,#15833,.F.);
#22779=ORIENTED_EDGE('',*,*,#15834,.F.);
#22780=ORIENTED_EDGE('',*,*,#15835,.F.);
#22781=ORIENTED_EDGE('',*,*,#15780,.F.);
#22782=ORIENTED_EDGE('',*,*,#15777,.F.);
#22783=ORIENTED_EDGE('',*,*,#15774,.F.);
#22784=ORIENTED_EDGE('',*,*,#15771,.F.);
#22785=ORIENTED_EDGE('',*,*,#15768,.F.);
#22786=ORIENTED_EDGE('',*,*,#15765,.F.);
#22787=ORIENTED_EDGE('',*,*,#15762,.F.);
#22788=ORIENTED_EDGE('',*,*,#15759,.F.);
#22789=ORIENTED_EDGE('',*,*,#15756,.F.);
#22790=ORIENTED_EDGE('',*,*,#15753,.F.);
#22791=ORIENTED_EDGE('',*,*,#15750,.F.);
#22792=ORIENTED_EDGE('',*,*,#15747,.F.);
#22793=ORIENTED_EDGE('',*,*,#15744,.F.);
#22794=ORIENTED_EDGE('',*,*,#15741,.F.);
#22795=ORIENTED_EDGE('',*,*,#15738,.F.);
#22796=ORIENTED_EDGE('',*,*,#15735,.F.);
#22797=ORIENTED_EDGE('',*,*,#15836,.F.);
#22798=ORIENTED_EDGE('',*,*,#15837,.T.);
#22799=ORIENTED_EDGE('',*,*,#15833,.T.);
#22800=ORIENTED_EDGE('',*,*,#15829,.T.);
#22801=ORIENTED_EDGE('',*,*,#15826,.T.);
#22802=ORIENTED_EDGE('',*,*,#15823,.T.);
#22803=ORIENTED_EDGE('',*,*,#15820,.T.);
#22804=ORIENTED_EDGE('',*,*,#15817,.T.);
#22805=ORIENTED_EDGE('',*,*,#15814,.T.);
#22806=ORIENTED_EDGE('',*,*,#15811,.T.);
#22807=ORIENTED_EDGE('',*,*,#15808,.T.);
#22808=ORIENTED_EDGE('',*,*,#15805,.T.);
#22809=ORIENTED_EDGE('',*,*,#15802,.T.);
#22810=ORIENTED_EDGE('',*,*,#15799,.T.);
#22811=ORIENTED_EDGE('',*,*,#15796,.T.);
#22812=ORIENTED_EDGE('',*,*,#15793,.T.);
#22813=ORIENTED_EDGE('',*,*,#15790,.T.);
#22814=ORIENTED_EDGE('',*,*,#15787,.T.);
#22815=ORIENTED_EDGE('',*,*,#15731,.F.);
#22816=ORIENTED_EDGE('',*,*,#15838,.T.);
#22817=ORIENTED_EDGE('',*,*,#15831,.T.);
#22818=ORIENTED_EDGE('',*,*,#15839,.T.);
#22819=ORIENTED_EDGE('',*,*,#15836,.T.);
#22820=ORIENTED_EDGE('',*,*,#15734,.F.);
#22821=ORIENTED_EDGE('',*,*,#15830,.T.);
#22822=ORIENTED_EDGE('',*,*,#15837,.F.);
#22823=ORIENTED_EDGE('',*,*,#15839,.F.);
#22824=ORIENTED_EDGE('',*,*,#15840,.F.);
#22825=ORIENTED_EDGE('',*,*,#15782,.F.);
#22826=ORIENTED_EDGE('',*,*,#15785,.F.);
#22827=ORIENTED_EDGE('',*,*,#15789,.F.);
#22828=ORIENTED_EDGE('',*,*,#15792,.F.);
#22829=ORIENTED_EDGE('',*,*,#15795,.F.);
#22830=ORIENTED_EDGE('',*,*,#15798,.F.);
#22831=ORIENTED_EDGE('',*,*,#15801,.F.);
#22832=ORIENTED_EDGE('',*,*,#15804,.F.);
#22833=ORIENTED_EDGE('',*,*,#15807,.F.);
#22834=ORIENTED_EDGE('',*,*,#15810,.F.);
#22835=ORIENTED_EDGE('',*,*,#15813,.F.);
#22836=ORIENTED_EDGE('',*,*,#15816,.F.);
#22837=ORIENTED_EDGE('',*,*,#15819,.F.);
#22838=ORIENTED_EDGE('',*,*,#15822,.F.);
#22839=ORIENTED_EDGE('',*,*,#15825,.F.);
#22840=ORIENTED_EDGE('',*,*,#15828,.F.);
#22841=ORIENTED_EDGE('',*,*,#15832,.F.);
#22842=ORIENTED_EDGE('',*,*,#15838,.F.);
#22843=ORIENTED_EDGE('',*,*,#15730,.F.);
#22844=ORIENTED_EDGE('',*,*,#15737,.F.);
#22845=ORIENTED_EDGE('',*,*,#15740,.F.);
#22846=ORIENTED_EDGE('',*,*,#15743,.F.);
#22847=ORIENTED_EDGE('',*,*,#15746,.F.);
#22848=ORIENTED_EDGE('',*,*,#15749,.F.);
#22849=ORIENTED_EDGE('',*,*,#15752,.F.);
#22850=ORIENTED_EDGE('',*,*,#15755,.F.);
#22851=ORIENTED_EDGE('',*,*,#15758,.F.);
#22852=ORIENTED_EDGE('',*,*,#15761,.F.);
#22853=ORIENTED_EDGE('',*,*,#15764,.F.);
#22854=ORIENTED_EDGE('',*,*,#15767,.F.);
#22855=ORIENTED_EDGE('',*,*,#15770,.F.);
#22856=ORIENTED_EDGE('',*,*,#15773,.F.);
#22857=ORIENTED_EDGE('',*,*,#15776,.F.);
#22858=ORIENTED_EDGE('',*,*,#15779,.F.);
#22859=ORIENTED_EDGE('',*,*,#15841,.F.);
#22860=ORIENTED_EDGE('',*,*,#15778,.T.);
#22861=ORIENTED_EDGE('',*,*,#15835,.T.);
#22862=ORIENTED_EDGE('',*,*,#15842,.F.);
#22863=ORIENTED_EDGE('',*,*,#15841,.T.);
#22864=ORIENTED_EDGE('',*,*,#15843,.F.);
#22865=ORIENTED_EDGE('',*,*,#15844,.F.);
#22866=ORIENTED_EDGE('',*,*,#15845,.F.);
#22867=ORIENTED_EDGE('',*,*,#15846,.T.);
#22868=ORIENTED_EDGE('',*,*,#15847,.F.);
#22869=ORIENTED_EDGE('',*,*,#15848,.F.);
#22870=ORIENTED_EDGE('',*,*,#15849,.F.);
#22871=ORIENTED_EDGE('',*,*,#15850,.F.);
#22872=ORIENTED_EDGE('',*,*,#15851,.F.);
#22873=ORIENTED_EDGE('',*,*,#15852,.F.);
#22874=ORIENTED_EDGE('',*,*,#15853,.F.);
#22875=ORIENTED_EDGE('',*,*,#15854,.T.);
#22876=ORIENTED_EDGE('',*,*,#15855,.F.);
#22877=ORIENTED_EDGE('',*,*,#15846,.F.);
#22878=ORIENTED_EDGE('',*,*,#15856,.F.);
#22879=ORIENTED_EDGE('',*,*,#15857,.F.);
#22880=ORIENTED_EDGE('',*,*,#15858,.F.);
#22881=ORIENTED_EDGE('',*,*,#15854,.F.);
#22882=ORIENTED_EDGE('',*,*,#15859,.F.);
#22883=ORIENTED_EDGE('',*,*,#15848,.T.);
#22884=ORIENTED_EDGE('',*,*,#15860,.F.);
#22885=ORIENTED_EDGE('',*,*,#15861,.F.);
#22886=ORIENTED_EDGE('',*,*,#15862,.F.);
#22887=ORIENTED_EDGE('',*,*,#15844,.T.);
#22888=ORIENTED_EDGE('',*,*,#15863,.T.);
#22889=ORIENTED_EDGE('',*,*,#15860,.T.);
#22890=ORIENTED_EDGE('',*,*,#15843,.T.);
#22891=ORIENTED_EDGE('',*,*,#15855,.T.);
#22892=ORIENTED_EDGE('',*,*,#15864,.T.);
#22893=ORIENTED_EDGE('',*,*,#15865,.T.);
#22894=ORIENTED_EDGE('',*,*,#15866,.T.);
#22895=ORIENTED_EDGE('',*,*,#15851,.T.);
#22896=ORIENTED_EDGE('',*,*,#15858,.T.);
#22897=ORIENTED_EDGE('',*,*,#15847,.T.);
#22898=ORIENTED_EDGE('',*,*,#15867,.T.);
#22899=ORIENTED_EDGE('',*,*,#15868,.T.);
#22900=ORIENTED_EDGE('',*,*,#15869,.T.);
#22901=ORIENTED_EDGE('',*,*,#15857,.T.);
#22902=ORIENTED_EDGE('',*,*,#15870,.F.);
#22903=ORIENTED_EDGE('',*,*,#15871,.T.);
#22904=ORIENTED_EDGE('',*,*,#15864,.F.);
#22905=ORIENTED_EDGE('',*,*,#15852,.T.);
#22906=ORIENTED_EDGE('',*,*,#15866,.F.);
#22907=ORIENTED_EDGE('',*,*,#15872,.F.);
#22908=ORIENTED_EDGE('',*,*,#15873,.F.);
#22909=ORIENTED_EDGE('',*,*,#15850,.T.);
#22910=ORIENTED_EDGE('',*,*,#15874,.F.);
#22911=ORIENTED_EDGE('',*,*,#15875,.T.);
#22912=ORIENTED_EDGE('',*,*,#15867,.F.);
#22913=ORIENTED_EDGE('',*,*,#15861,.T.);
#22914=ORIENTED_EDGE('',*,*,#15869,.F.);
#22915=ORIENTED_EDGE('',*,*,#15876,.F.);
#22916=ORIENTED_EDGE('',*,*,#15877,.F.);
#22917=ORIENTED_EDGE('',*,*,#15865,.F.);
#22918=ORIENTED_EDGE('',*,*,#15871,.F.);
#22919=ORIENTED_EDGE('',*,*,#15878,.F.);
#22920=ORIENTED_EDGE('',*,*,#15872,.T.);
#22921=ORIENTED_EDGE('',*,*,#15868,.F.);
#22922=ORIENTED_EDGE('',*,*,#15875,.F.);
#22923=ORIENTED_EDGE('',*,*,#15879,.F.);
#22924=ORIENTED_EDGE('',*,*,#15876,.T.);
#22925=ORIENTED_EDGE('',*,*,#15877,.T.);
#22926=ORIENTED_EDGE('',*,*,#15879,.T.);
#22927=ORIENTED_EDGE('',*,*,#15874,.T.);
#22928=ORIENTED_EDGE('',*,*,#15849,.T.);
#22929=ORIENTED_EDGE('',*,*,#15859,.T.);
#22930=ORIENTED_EDGE('',*,*,#15853,.T.);
#22931=ORIENTED_EDGE('',*,*,#15873,.T.);
#22932=ORIENTED_EDGE('',*,*,#15878,.T.);
#22933=ORIENTED_EDGE('',*,*,#15870,.T.);
#22934=ORIENTED_EDGE('',*,*,#15856,.T.);
#22935=ORIENTED_EDGE('',*,*,#15845,.T.);
#22936=ORIENTED_EDGE('',*,*,#15862,.T.);
#22937=ORIENTED_EDGE('',*,*,#15880,.F.);
#22938=ORIENTED_EDGE('',*,*,#15733,.F.);
#22939=ORIENTED_EDGE('',*,*,#15881,.T.);
#22940=ORIENTED_EDGE('',*,*,#15880,.T.);
#22941=ORIENTED_EDGE('',*,*,#15881,.F.);
#22942=ORIENTED_EDGE('',*,*,#15882,.F.);
#22943=ORIENTED_EDGE('',*,*,#15842,.T.);
#22944=ORIENTED_EDGE('',*,*,#15834,.T.);
#22945=ORIENTED_EDGE('',*,*,#15786,.T.);
#22946=ORIENTED_EDGE('',*,*,#15783,.T.);
#22947=ORIENTED_EDGE('',*,*,#15840,.T.);
#22948=ORIENTED_EDGE('',*,*,#15883,.F.);
#22949=ORIENTED_EDGE('',*,*,#15884,.T.);
#22950=ORIENTED_EDGE('',*,*,#15882,.T.);
#22951=ORIENTED_EDGE('',*,*,#15884,.F.);
#22952=ORIENTED_EDGE('',*,*,#15863,.F.);
#22953=ORIENTED_EDGE('',*,*,#15885,.T.);
#22954=ORIENTED_EDGE('',*,*,#15883,.T.);
#22955=ORIENTED_EDGE('',*,*,#15885,.F.);
#22956=CONICAL_SURFACE('',#24772,4.7393933982822,0.392699081698728);
#22957=CONICAL_SURFACE('',#24776,4.71,0.785398163397448);
#22958=CONICAL_SURFACE('',#24780,4.6656066017178,1.17809724509617);
#22959=CONICAL_SURFACE('',#24783,4.71,0.785398163397448);
#22960=CONICAL_SURFACE('',#24793,4.6656066017178,1.17809724509617);
#22961=CONICAL_SURFACE('',#24803,0.754393398282202,1.17809724509617);
#22962=CONICAL_SURFACE('',#24805,0.725,0.785398163397448);
#22963=CONICAL_SURFACE('',#24807,0.710606601717798,0.392699081698724);
#22964=CONICAL_SURFACE('',#24813,0.710606601717798,0.392699081698723);
#22965=CONICAL_SURFACE('',#24815,0.725,0.785398163397448);
#22966=CONICAL_SURFACE('',#24817,0.754393398282202,1.17809724509618);
#22967=CONICAL_SURFACE('',#24824,0.225,0.785398163397452);
#22968=CONICAL_SURFACE('',#24829,0.225,0.785398163397445);
#22969=CONICAL_SURFACE('',#24834,0.225,0.785398163397449);
#22970=CONICAL_SURFACE('',#24839,0.225,0.785398163397452);
#22971=CONICAL_SURFACE('',#24844,0.225,0.785398163397449);
#22972=CONICAL_SURFACE('',#24849,0.225,0.785398163397445);
#22973=CONICAL_SURFACE('',#24854,4.7393933982822,0.392699081698727);
#22974=CONICAL_SURFACE('',#24859,4.735,0.785398163397452);
#22975=CONICAL_SURFACE('',#24863,4.735,0.785398163397452);
#22976=CONICAL_SURFACE('',#24868,0.0649999999999999,1.02974425867665);
#22977=CONICAL_SURFACE('',#24872,0.18,0.78539816339745);
#22978=CONICAL_SURFACE('',#24873,0.0649999999999999,1.02974425867665);
#22979=CONICAL_SURFACE('',#24877,0.18,0.78539816339745);
#22980=CONICAL_SURFACE('',#24878,0.065,1.02974425867665);
#22981=CONICAL_SURFACE('',#24882,0.18,0.785398163397449);
#22982=CONICAL_SURFACE('',#24883,0.1325,0.321750554396641);
#22983=CONICAL_SURFACE('',#24887,0.1325,0.785398163397446);
#22984=CONICAL_SURFACE('',#24890,0.1325,0.321750554396641);
#22985=CONICAL_SURFACE('',#24894,0.1325,0.785398163397446);
#22986=CONICAL_SURFACE('',#24897,0.1325,0.321750554396647);
#22987=CONICAL_SURFACE('',#24901,0.1325,0.785398163397455);
#22988=CONICAL_SURFACE('',#24904,0.132499999999999,0.321750554396641);
#22989=CONICAL_SURFACE('',#24908,0.132499999999999,0.785398163397446);
#22990=CONICAL_SURFACE('',#24911,0.1325,0.321750554396641);
#22991=CONICAL_SURFACE('',#24915,0.1325,0.785398163397446);
#22992=CONICAL_SURFACE('',#24918,0.1325,0.321750554396647);
#22993=CONICAL_SURFACE('',#24922,0.1325,0.785398163397455);
#22994=CONICAL_SURFACE('',#24925,4.075,0.785398163397448);
#22995=CONICAL_SURFACE('',#24930,0.0524999999999998,1.02974425867665);
#22996=CONICAL_SURFACE('',#24934,0.155,0.78539816339745);
#22997=CONICAL_SURFACE('',#24936,0.0525000000000002,1.02974425867665);
#22998=CONICAL_SURFACE('',#24940,0.155,0.78539816339745);
#22999=CONICAL_SURFACE('',#24942,0.0525000000000002,1.02974425867665);
#23000=CONICAL_SURFACE('',#24946,0.154999999999999,0.785398163397452);
#23001=CONICAL_SURFACE('',#24948,0.0525000000000002,1.02974425867665);
#23002=CONICAL_SURFACE('',#24952,0.155,0.78539816339745);
#23003=CONICAL_SURFACE('',#24954,0.0524999999999998,1.02974425867665);
#23004=CONICAL_SURFACE('',#24958,0.155,0.78539816339745);
#23005=CONICAL_SURFACE('',#24960,0.0525000000000002,1.02974425867665);
#23006=CONICAL_SURFACE('',#24964,0.154999999999999,0.785398163397452);
#23007=CONICAL_SURFACE('',#24966,0.0525000000000002,1.02974425867665);
#23008=CONICAL_SURFACE('',#24970,0.154999999999999,0.785398163397448);
#23009=CONICAL_SURFACE('',#24972,0.0524999999999998,1.02974425867665);
#23010=CONICAL_SURFACE('',#24976,0.155,0.785398163397451);
#23011=CONICAL_SURFACE('',#24978,0.0525,1.02974425867665);
#23012=CONICAL_SURFACE('',#24982,0.155,0.785398163397451);
#23013=CONICAL_SURFACE('',#24984,0.0525,1.02974425867665);
#23014=CONICAL_SURFACE('',#24988,0.155,0.78539816339745);
#23015=CONICAL_SURFACE('',#24990,0.0525000000000002,1.02974425867665);
#23016=CONICAL_SURFACE('',#24994,0.155,0.785398163397451);
#23017=CONICAL_SURFACE('',#24996,0.0525000000000002,1.02974425867666);
#23018=CONICAL_SURFACE('',#25000,0.155,0.785398163397448);
#23019=CONICAL_SURFACE('',#25002,0.0524999999999993,1.02974425867665);
#23020=CONICAL_SURFACE('',#25006,0.155,0.785398163397453);
#23021=CONICAL_SURFACE('',#25008,0.0525000000000002,1.02974425867665);
#23022=CONICAL_SURFACE('',#25012,0.155,0.785398163397451);
#23023=CONICAL_SURFACE('',#25014,0.0525,1.02974425867665);
#23024=CONICAL_SURFACE('',#25018,0.155,0.78539816339745);
#23025=CONICAL_SURFACE('',#25020,0.0525,1.02974425867665);
#23026=CONICAL_SURFACE('',#25024,0.155,0.785398163397451);
#23027=CONICAL_SURFACE('',#25026,0.0524999999999998,1.02974425867665);
#23028=CONICAL_SURFACE('',#25030,0.155,0.785398163397448);
#23029=CONICAL_SURFACE('',#25032,0.0525000000000002,1.02974425867665);
#23030=CONICAL_SURFACE('',#25036,0.154999999999999,0.785398163397448);
#23031=CONICAL_SURFACE('',#25038,4.115,0.785398163397441);
#23032=CONICAL_SURFACE('',#25047,4.115,0.785398163397463);
#23033=CONICAL_SURFACE('',#25051,4.58,0.785398163397459);
#23034=CONICAL_SURFACE('',#25057,4.58,0.785398163397443);
#23035=CONICAL_SURFACE('',#25059,0.0525,1.02974425867667);
#23036=CONICAL_SURFACE('',#25063,0.155,0.78539816339745);
#23037=CONICAL_SURFACE('',#25065,0.0525,1.02974425867667);
#23038=CONICAL_SURFACE('',#25069,0.155,0.78539816339745);
#23039=CONICAL_SURFACE('',#25071,0.0650000000000004,1.02974425867666);
#23040=CONICAL_SURFACE('',#25075,0.180000000000001,0.785398163397451);
#23041=CONICAL_SURFACE('',#25077,0.0649999999999999,1.02974425867666);
#23042=CONICAL_SURFACE('',#25081,0.18,0.785398163397451);
#23043=CONICAL_SURFACE('',#25083,0.065,1.02974425867666);
#23044=CONICAL_SURFACE('',#25087,0.18,0.78539816339745);
#23045=CONICAL_SURFACE('',#25089,0.1325,0.321750554396632);
#23046=CONICAL_SURFACE('',#25094,0.1325,0.785398163397466);
#23047=CONICAL_SURFACE('',#25100,0.1325,0.321750554396642);
#23048=CONICAL_SURFACE('',#25105,0.1325,0.785398163397484);
#23049=CONICAL_SURFACE('',#25111,0.1325,0.32175055439664);
#23050=CONICAL_SURFACE('',#25116,0.1325,0.785398163397479);
#23051=CONICAL_SURFACE('',#25122,0.1325,0.321750554396637);
#23052=CONICAL_SURFACE('',#25127,0.1325,0.785398163397475);
#23053=CONICAL_SURFACE('',#25133,0.1325,0.321750554396637);
#23054=CONICAL_SURFACE('',#25138,0.1325,0.785398163397475);
#23055=CONICAL_SURFACE('',#25144,0.1325,0.321750554396632);
#23056=CONICAL_SURFACE('',#25149,0.1325,0.785398163397466);
#23057=CONICAL_SURFACE('',#25155,0.1325,0.321750554396642);
#23058=CONICAL_SURFACE('',#25160,0.1325,0.785398163397484);
#23059=CONICAL_SURFACE('',#25166,0.132499999999999,0.321750554396637);
#23060=CONICAL_SURFACE('',#25171,0.132499999999999,0.785398163397475);
#23061=CONICAL_SURFACE('',#25177,0.1325,0.321750554396637);
#23062=CONICAL_SURFACE('',#25182,0.1325,0.785398163397475);
#23063=CONICAL_SURFACE('',#25188,0.1325,0.32175055439664);
#23064=CONICAL_SURFACE('',#25193,0.1325,0.785398163397479);
#23065=CONICAL_SURFACE('',#25199,0.1325,0.321750554396637);
#23066=CONICAL_SURFACE('',#25204,0.1325,0.785398163397475);
#23067=CONICAL_SURFACE('',#25210,0.1325,0.321750554396632);
#23068=CONICAL_SURFACE('',#25215,0.1325,0.785398163397466);
#23069=CONICAL_SURFACE('',#25221,0.72,0.785398163397459);
#23070=CONICAL_SURFACE('',#25230,0.72,0.785398163397459);
#23071=CONICAL_SURFACE('',#25234,4.585,0.785398163397463);
#23072=CONICAL_SURFACE('',#25243,4.585,0.785398163397463);
#23073=CONICAL_SURFACE('',#25632,1.035,0.785398163397459);
#23074=CONICAL_SURFACE('',#25641,1.035,0.785398163397459);
#23075=CONICAL_SURFACE('',#25645,0.6543933982822,1.17809724509617);
#23076=CONICAL_SURFACE('',#25648,0.625,0.785398163397442);
#23077=CONICAL_SURFACE('',#25652,0.610606601717797,0.39269908169869);
#23078=CONICAL_SURFACE('',#25658,0.610606601717798,0.392699081698726);
#23079=CONICAL_SURFACE('',#25660,0.625,0.785398163397442);
#23080=CONICAL_SURFACE('',#25662,0.654393398282201,1.17809724509617);
#23081=CONICAL_SURFACE('',#25666,0.88,0.785398163397459);
#23082=CONICAL_SURFACE('',#25678,1.05,0.643501108793286);
#23083=CONICAL_SURFACE('',#25682,1.08,0.785398163397459);
#23084=CONICAL_SURFACE('',#25692,1.4956066017178,1.17809724509617);
#23085=CONICAL_SURFACE('',#25694,1.525,0.785398163397442);
#23086=CONICAL_SURFACE('',#25696,1.5393933982822,0.392699081698728);
#23087=CONICAL_SURFACE('',#25702,1.5393933982822,0.392699081698728);
#23088=CONICAL_SURFACE('',#25704,1.525,0.785398163397442);
#23089=CONICAL_SURFACE('',#25706,0.925,0.785398163397459);
#23090=CONICAL_SURFACE('',#25714,1.4956066017178,1.17809724509617);
#23091=CONICAL_SURFACE('',#25718,0.225,0.785398163397459);
#23092=CONICAL_SURFACE('',#25725,0.225,0.785398163397459);
#23093=CONICAL_SURFACE('',#25732,0.1325,0.321750554396645);
#23094=CONICAL_SURFACE('',#25736,0.1325,0.785398163397441);
#23095=CONICAL_SURFACE('',#25739,0.1325,0.321750554396645);
#23096=CONICAL_SURFACE('',#25743,0.1325,0.785398163397441);
#23097=CONICAL_SURFACE('',#25746,0.93,0.785398163397459);
#23098=CONICAL_SURFACE('',#25759,0.18,0.785398163397448);
#23099=CONICAL_SURFACE('',#25779,0.815,0.785398163397459);
#23100=CONICAL_SURFACE('',#25788,0.815,0.785398163397459);
#23101=CONICAL_SURFACE('',#25792,3.985,0.785398163397456);
#23102=CONICAL_SURFACE('',#25798,3.985,0.785398163397456);
#23103=CONICAL_SURFACE('',#25800,0.0425,1.02974425867665);
#23104=CONICAL_SURFACE('',#25804,0.0425,1.02974425867665);
#23105=CONICAL_SURFACE('',#25814,0.52,0.785398163397448);
#23106=CONICAL_SURFACE('',#25829,0.78,0.785398163397454);
#23107=CONICAL_SURFACE('',#25832,0.78,0.785398163397449);
#23108=CONICAL_SURFACE('',#25842,0.09,0.785398163397451);
#23109=CONICAL_SURFACE('',#25846,0.185,0.785398163397459);
#23110=CONICAL_SURFACE('',#25854,0.115,0.785398163397459);
#23111=CONICAL_SURFACE('',#25860,0.115,0.785398163397459);
#23112=CONICAL_SURFACE('',#25867,0.39,0.785398163397459);
#23113=CONICAL_SURFACE('',#25872,0.1,0.785398163397459);
#23114=CONICAL_SURFACE('',#25881,0.1,0.785398163397459);
#23115=CONICAL_SURFACE('',#25887,0.1,0.785398163397459);
#23116=CONICAL_SURFACE('',#25891,0.1,0.785398163397459);
#23117=CONICAL_SURFACE('',#25892,0.1,0.785398163397459);
#23118=CONICAL_SURFACE('',#25896,0.1,0.785398163397459);
#23119=CONICAL_SURFACE('',#25899,0.69,0.785398163397459);
#23120=CONICAL_SURFACE('',#25905,0.69,0.785398163397459);
#23121=CONICAL_SURFACE('',#25907,0.2175,0.785398163397459);
#23122=CONICAL_SURFACE('',#25924,0.2175,0.785398163397459);
#23123=CONICAL_SURFACE('',#25931,0.685,0.785398163397459);
#23124=CONICAL_SURFACE('',#25937,0.105,0.785398163397459);
#23125=CONICAL_SURFACE('',#25941,0.105,0.785398163397459);
#23126=CONICAL_SURFACE('',#25942,0.105,0.785398163397459);
#23127=CONICAL_SURFACE('',#25946,0.105,0.785398163397459);
#23128=CONICAL_SURFACE('',#25947,0.105,0.785398163397459);
#23129=CONICAL_SURFACE('',#25951,0.105,0.785398163397459);
#23130=CONICAL_SURFACE('',#25952,0.69,0.785398163397459);
#23131=CONICAL_SURFACE('',#26170,0.0207846096908265,0.995084829080935);
#23132=CONICAL_SURFACE('',#26181,0.085,0.876058050598194);
#23133=CONICAL_SURFACE('',#26182,0.09,0.785398163397448);
#23134=CONICAL_SURFACE('',#26211,0.065,1.02974425867665);
#23135=CONICAL_SURFACE('',#26215,0.18,0.785398163397448);
#23136=CONICAL_SURFACE('',#26217,0.2825,0.785398163397448);
#23137=CONICAL_SURFACE('',#26219,0.2825,0.785398163397448);
#23138=CONICAL_SURFACE('',#26221,0.2825,0.785398163397448);
#23139=CONICAL_SURFACE('',#26223,0.2825,0.785398163397448);
#23140=CONICAL_SURFACE('',#26225,0.2825,0.785398163397448);
#23141=CONICAL_SURFACE('',#26227,0.2825,0.785398163397448);
#23142=CONICAL_SURFACE('',#26234,0.2825,0.785398163397448);
#23143=CONICAL_SURFACE('',#26236,0.2825,0.785398163397448);
#23144=CONICAL_SURFACE('',#26238,0.2825,0.785398163397448);
#23145=CONICAL_SURFACE('',#26240,0.2825,0.785398163397448);
#23146=CONICAL_SURFACE('',#26242,0.2825,0.785398163397448);
#23147=CONICAL_SURFACE('',#26244,0.2825,0.785398163397448);
#23148=CONICAL_SURFACE('',#26249,0.115,0.785398163397448);
#23149=CONICAL_SURFACE('',#26504,0.1825,0.785398163397448);
#23150=CONICAL_SURFACE('',#26506,0.0346410161513776,1.00188494390461);
#23151=CONICAL_SURFACE('',#26517,0.088,0.785398163397448);
#23152=CONICAL_SURFACE('',#26520,0.105,0.785398163397449);
#23153=CONICAL_SURFACE('',#26766,0.1825,0.785398163397448);
#23154=CONICAL_SURFACE('',#26768,0.0346410161513776,1.00188494390461);
#23155=CONICAL_SURFACE('',#26779,0.088,0.785398163397448);
#23156=CONICAL_SURFACE('',#26782,0.105,0.785398163397449);
#23157=CONICAL_SURFACE('',#27007,0.2175,0.785398163397448);
#23158=CONICAL_SURFACE('',#27009,0.0461880215351701,1.00445035903315);
#23159=CONICAL_SURFACE('',#27020,0.11,0.78539816339745);
#23160=CONICAL_SURFACE('',#27021,0.13,0.785398163397449);
#23161=CONICAL_SURFACE('',#27066,0.0704,0.785398163397448);
#23162=CONICAL_SURFACE('',#27073,0.14375,0.558599315343562);
#23163=CONICAL_SURFACE('',#27136,0.0704,0.785398163397448);
#23164=CONICAL_SURFACE('',#27141,0.14375,0.558599315343562);
#23165=ADVANCED_FACE('',(#2412),#22956,.T.);
#23166=ADVANCED_FACE('',(#2413),#22957,.T.);
#23167=ADVANCED_FACE('',(#2414),#1952,.T.);
#23168=ADVANCED_FACE('',(#2415),#22958,.T.);
#23169=ADVANCED_FACE('',(#2416),#22959,.T.);
#23170=ADVANCED_FACE('',(#2417,#1036,#1037,#1038,#1039,#1040,#1041,#1042),
#1276,.T.);
#23171=ADVANCED_FACE('',(#2418),#22960,.T.);
#23172=ADVANCED_FACE('',(#2419,#1043,#1044,#1045,#1046,#1047,#1048,#1049),
#1277,.T.);
#23173=ADVANCED_FACE('',(#2420),#22961,.F.);
#23174=ADVANCED_FACE('',(#2421),#22962,.F.);
#23175=ADVANCED_FACE('',(#2422),#22963,.F.);
#23176=ADVANCED_FACE('',(#2423),#1953,.F.);
#23177=ADVANCED_FACE('',(#2424),#22964,.F.);
#23178=ADVANCED_FACE('',(#2425),#22965,.F.);
#23179=ADVANCED_FACE('',(#2426),#22966,.F.);
#23180=ADVANCED_FACE('',(#2427,#1050,#1051,#1052,#1053),#1278,.T.);
#23181=ADVANCED_FACE('',(#2428),#22967,.F.);
#23182=ADVANCED_FACE('',(#2429),#1954,.F.);
#23183=ADVANCED_FACE('',(#2430),#22968,.F.);
#23184=ADVANCED_FACE('',(#2431),#1955,.F.);
#23185=ADVANCED_FACE('',(#2432),#22969,.F.);
#23186=ADVANCED_FACE('',(#2433),#1956,.F.);
#23187=ADVANCED_FACE('',(#2434),#22970,.F.);
#23188=ADVANCED_FACE('',(#2435),#1957,.F.);
#23189=ADVANCED_FACE('',(#2436),#22971,.F.);
#23190=ADVANCED_FACE('',(#2437),#1958,.F.);
#23191=ADVANCED_FACE('',(#2438),#22972,.F.);
#23192=ADVANCED_FACE('',(#2439),#1959,.F.);
#23193=ADVANCED_FACE('',(#2440),#22973,.T.);
#23194=ADVANCED_FACE('',(#2441),#1960,.T.);
#23195=ADVANCED_FACE('',(#2442),#22974,.T.);
#23196=ADVANCED_FACE('',(#2443,#1054),#1279,.F.);
#23197=ADVANCED_FACE('',(#2444),#22975,.T.);
#23198=ADVANCED_FACE('',(#2445,#1055),#1280,.F.);
#23199=ADVANCED_FACE('',(#2446),#1961,.T.);
#23200=ADVANCED_FACE('',(#2447),#22976,.F.);
#23201=ADVANCED_FACE('',(#2448),#1962,.F.);
#23202=ADVANCED_FACE('',(#2449),#22977,.F.);
#23203=ADVANCED_FACE('',(#2450),#22978,.F.);
#23204=ADVANCED_FACE('',(#2451),#1963,.F.);
#23205=ADVANCED_FACE('',(#2452),#22979,.F.);
#23206=ADVANCED_FACE('',(#2453),#22980,.F.);
#23207=ADVANCED_FACE('',(#2454),#1964,.F.);
#23208=ADVANCED_FACE('',(#2455),#22981,.F.);
#23209=ADVANCED_FACE('',(#2456),#22982,.F.);
#23210=ADVANCED_FACE('',(#2457),#1965,.F.);
#23211=ADVANCED_FACE('',(#2458),#22983,.F.);
#23212=ADVANCED_FACE('',(#2459,#1056),#1281,.F.);
#23213=ADVANCED_FACE('',(#2460),#22984,.F.);
#23214=ADVANCED_FACE('',(#2461),#1966,.F.);
#23215=ADVANCED_FACE('',(#2462),#22985,.F.);
#23216=ADVANCED_FACE('',(#2463,#1057),#1282,.F.);
#23217=ADVANCED_FACE('',(#2464),#22986,.F.);
#23218=ADVANCED_FACE('',(#2465),#1967,.F.);
#23219=ADVANCED_FACE('',(#2466),#22987,.F.);
#23220=ADVANCED_FACE('',(#2467,#1058),#1283,.F.);
#23221=ADVANCED_FACE('',(#2468),#22988,.F.);
#23222=ADVANCED_FACE('',(#2469),#1968,.F.);
#23223=ADVANCED_FACE('',(#2470),#22989,.F.);
#23224=ADVANCED_FACE('',(#2471,#1059),#1284,.F.);
#23225=ADVANCED_FACE('',(#2472),#22990,.F.);
#23226=ADVANCED_FACE('',(#2473),#1969,.F.);
#23227=ADVANCED_FACE('',(#2474),#22991,.F.);
#23228=ADVANCED_FACE('',(#2475,#1060),#1285,.F.);
#23229=ADVANCED_FACE('',(#2476),#22992,.F.);
#23230=ADVANCED_FACE('',(#2477),#1970,.F.);
#23231=ADVANCED_FACE('',(#2478),#22993,.F.);
#23232=ADVANCED_FACE('',(#2479,#1061),#1286,.F.);
#23233=ADVANCED_FACE('',(#2480),#22994,.T.);
#23234=ADVANCED_FACE('',(#2481),#1971,.T.);
#23235=ADVANCED_FACE('',(#2482),#22995,.F.);
#23236=ADVANCED_FACE('',(#2483),#1972,.F.);
#23237=ADVANCED_FACE('',(#2484),#22996,.F.);
#23238=ADVANCED_FACE('',(#2485),#22997,.F.);
#23239=ADVANCED_FACE('',(#2486),#1973,.F.);
#23240=ADVANCED_FACE('',(#2487),#22998,.F.);
#23241=ADVANCED_FACE('',(#2488),#22999,.F.);
#23242=ADVANCED_FACE('',(#2489),#1974,.F.);
#23243=ADVANCED_FACE('',(#2490),#23000,.F.);
#23244=ADVANCED_FACE('',(#2491),#23001,.F.);
#23245=ADVANCED_FACE('',(#2492),#1975,.F.);
#23246=ADVANCED_FACE('',(#2493),#23002,.F.);
#23247=ADVANCED_FACE('',(#2494),#23003,.F.);
#23248=ADVANCED_FACE('',(#2495),#1976,.F.);
#23249=ADVANCED_FACE('',(#2496),#23004,.F.);
#23250=ADVANCED_FACE('',(#2497),#23005,.F.);
#23251=ADVANCED_FACE('',(#2498),#1977,.F.);
#23252=ADVANCED_FACE('',(#2499),#23006,.F.);
#23253=ADVANCED_FACE('',(#2500),#23007,.F.);
#23254=ADVANCED_FACE('',(#2501),#1978,.F.);
#23255=ADVANCED_FACE('',(#2502),#23008,.F.);
#23256=ADVANCED_FACE('',(#2503),#23009,.F.);
#23257=ADVANCED_FACE('',(#2504),#1979,.F.);
#23258=ADVANCED_FACE('',(#2505),#23010,.F.);
#23259=ADVANCED_FACE('',(#2506),#23011,.F.);
#23260=ADVANCED_FACE('',(#2507),#1980,.F.);
#23261=ADVANCED_FACE('',(#2508),#23012,.F.);
#23262=ADVANCED_FACE('',(#2509),#23013,.F.);
#23263=ADVANCED_FACE('',(#2510),#1981,.F.);
#23264=ADVANCED_FACE('',(#2511),#23014,.F.);
#23265=ADVANCED_FACE('',(#2512),#23015,.F.);
#23266=ADVANCED_FACE('',(#2513),#1982,.F.);
#23267=ADVANCED_FACE('',(#2514),#23016,.F.);
#23268=ADVANCED_FACE('',(#2515),#23017,.F.);
#23269=ADVANCED_FACE('',(#2516),#1983,.F.);
#23270=ADVANCED_FACE('',(#2517),#23018,.F.);
#23271=ADVANCED_FACE('',(#2518),#23019,.F.);
#23272=ADVANCED_FACE('',(#2519),#1984,.F.);
#23273=ADVANCED_FACE('',(#2520),#23020,.F.);
#23274=ADVANCED_FACE('',(#2521),#23021,.F.);
#23275=ADVANCED_FACE('',(#2522),#1985,.F.);
#23276=ADVANCED_FACE('',(#2523),#23022,.F.);
#23277=ADVANCED_FACE('',(#2524),#23023,.F.);
#23278=ADVANCED_FACE('',(#2525),#1986,.F.);
#23279=ADVANCED_FACE('',(#2526),#23024,.F.);
#23280=ADVANCED_FACE('',(#2527),#23025,.F.);
#23281=ADVANCED_FACE('',(#2528),#1987,.F.);
#23282=ADVANCED_FACE('',(#2529),#23026,.F.);
#23283=ADVANCED_FACE('',(#2530),#23027,.F.);
#23284=ADVANCED_FACE('',(#2531),#1988,.F.);
#23285=ADVANCED_FACE('',(#2532),#23028,.F.);
#23286=ADVANCED_FACE('',(#2533),#23029,.F.);
#23287=ADVANCED_FACE('',(#2534),#1989,.F.);
#23288=ADVANCED_FACE('',(#2535),#23030,.F.);
#23289=ADVANCED_FACE('',(#2536),#23031,.F.);
#23290=ADVANCED_FACE('',(#2537),#1990,.F.);
#23291=ADVANCED_FACE('',(#2538,#1062,#1063,#1064,#1065,#1066,#1067,#1068),
#1287,.T.);
#23292=ADVANCED_FACE('',(#2539),#23032,.F.);
#23293=ADVANCED_FACE('',(#2540,#1069,#1070,#1071,#1072,#1073,#1074,#1075,
#1076,#1077,#1078,#1079,#1080,#1081),#1288,.T.);
#23294=ADVANCED_FACE('',(#2541),#23033,.T.);
#23295=ADVANCED_FACE('',(#2542),#1991,.T.);
#23296=ADVANCED_FACE('',(#2543),#23034,.T.);
#23297=ADVANCED_FACE('',(#2544),#23035,.F.);
#23298=ADVANCED_FACE('',(#2545),#1992,.F.);
#23299=ADVANCED_FACE('',(#2546),#23036,.F.);
#23300=ADVANCED_FACE('',(#2547),#23037,.F.);
#23301=ADVANCED_FACE('',(#2548),#1993,.F.);
#23302=ADVANCED_FACE('',(#2549),#23038,.F.);
#23303=ADVANCED_FACE('',(#2550),#23039,.F.);
#23304=ADVANCED_FACE('',(#2551),#1994,.F.);
#23305=ADVANCED_FACE('',(#2552),#23040,.F.);
#23306=ADVANCED_FACE('',(#2553),#23041,.F.);
#23307=ADVANCED_FACE('',(#2554),#1995,.F.);
#23308=ADVANCED_FACE('',(#2555),#23042,.F.);
#23309=ADVANCED_FACE('',(#2556),#23043,.F.);
#23310=ADVANCED_FACE('',(#2557),#1996,.F.);
#23311=ADVANCED_FACE('',(#2558),#23044,.F.);
#23312=ADVANCED_FACE('',(#2559),#23045,.F.);
#23313=ADVANCED_FACE('',(#2560),#1997,.F.);
#23314=ADVANCED_FACE('',(#2561),#23046,.F.);
#23315=ADVANCED_FACE('',(#2562,#1082),#1289,.F.);
#23316=ADVANCED_FACE('',(#2563),#1998,.F.);
#23317=ADVANCED_FACE('',(#2564),#23047,.F.);
#23318=ADVANCED_FACE('',(#2565),#1999,.F.);
#23319=ADVANCED_FACE('',(#2566),#23048,.F.);
#23320=ADVANCED_FACE('',(#2567,#1083),#1290,.F.);
#23321=ADVANCED_FACE('',(#2568),#2000,.F.);
#23322=ADVANCED_FACE('',(#2569),#23049,.F.);
#23323=ADVANCED_FACE('',(#2570),#2001,.F.);
#23324=ADVANCED_FACE('',(#2571),#23050,.F.);
#23325=ADVANCED_FACE('',(#2572,#1084),#1291,.F.);
#23326=ADVANCED_FACE('',(#2573),#2002,.F.);
#23327=ADVANCED_FACE('',(#2574),#23051,.F.);
#23328=ADVANCED_FACE('',(#2575),#2003,.F.);
#23329=ADVANCED_FACE('',(#2576),#23052,.F.);
#23330=ADVANCED_FACE('',(#2577,#1085),#1292,.F.);
#23331=ADVANCED_FACE('',(#2578),#2004,.F.);
#23332=ADVANCED_FACE('',(#2579),#23053,.F.);
#23333=ADVANCED_FACE('',(#2580),#2005,.F.);
#23334=ADVANCED_FACE('',(#2581),#23054,.F.);
#23335=ADVANCED_FACE('',(#2582,#1086),#1293,.F.);
#23336=ADVANCED_FACE('',(#2583),#2006,.F.);
#23337=ADVANCED_FACE('',(#2584),#23055,.F.);
#23338=ADVANCED_FACE('',(#2585),#2007,.F.);
#23339=ADVANCED_FACE('',(#2586),#23056,.F.);
#23340=ADVANCED_FACE('',(#2587,#1087),#1294,.F.);
#23341=ADVANCED_FACE('',(#2588),#2008,.F.);
#23342=ADVANCED_FACE('',(#2589),#23057,.F.);
#23343=ADVANCED_FACE('',(#2590),#2009,.F.);
#23344=ADVANCED_FACE('',(#2591),#23058,.F.);
#23345=ADVANCED_FACE('',(#2592,#1088),#1295,.F.);
#23346=ADVANCED_FACE('',(#2593),#2010,.F.);
#23347=ADVANCED_FACE('',(#2594),#23059,.F.);
#23348=ADVANCED_FACE('',(#2595),#2011,.F.);
#23349=ADVANCED_FACE('',(#2596),#23060,.F.);
#23350=ADVANCED_FACE('',(#2597,#1089),#1296,.F.);
#23351=ADVANCED_FACE('',(#2598),#2012,.F.);
#23352=ADVANCED_FACE('',(#2599),#23061,.F.);
#23353=ADVANCED_FACE('',(#2600),#2013,.F.);
#23354=ADVANCED_FACE('',(#2601),#23062,.F.);
#23355=ADVANCED_FACE('',(#2602,#1090),#1297,.F.);
#23356=ADVANCED_FACE('',(#2603),#2014,.F.);
#23357=ADVANCED_FACE('',(#2604),#23063,.F.);
#23358=ADVANCED_FACE('',(#2605),#2015,.F.);
#23359=ADVANCED_FACE('',(#2606),#23064,.F.);
#23360=ADVANCED_FACE('',(#2607,#1091),#1298,.F.);
#23361=ADVANCED_FACE('',(#2608),#2016,.F.);
#23362=ADVANCED_FACE('',(#2609),#23065,.F.);
#23363=ADVANCED_FACE('',(#2610),#2017,.F.);
#23364=ADVANCED_FACE('',(#2611),#23066,.F.);
#23365=ADVANCED_FACE('',(#2612,#1092),#1299,.F.);
#23366=ADVANCED_FACE('',(#2613),#2018,.F.);
#23367=ADVANCED_FACE('',(#2614),#23067,.F.);
#23368=ADVANCED_FACE('',(#2615),#2019,.F.);
#23369=ADVANCED_FACE('',(#2616),#23068,.F.);
#23370=ADVANCED_FACE('',(#2617,#1093),#1300,.F.);
#23371=ADVANCED_FACE('',(#2618),#2020,.F.);
#23372=ADVANCED_FACE('',(#2619),#23069,.F.);
#23373=ADVANCED_FACE('',(#2620),#2021,.F.);
#23374=ADVANCED_FACE('',(#2621,#1094,#1095,#1096,#1097),#1301,.T.);
#23375=ADVANCED_FACE('',(#2622),#23070,.F.);
#23376=ADVANCED_FACE('',(#2623,#1098),#1302,.T.);
#23377=ADVANCED_FACE('',(#2624),#23071,.T.);
#23378=ADVANCED_FACE('',(#2625),#2022,.T.);
#23379=ADVANCED_FACE('',(#2626,#1099,#1100,#1101,#1102,#1103,#1104,#1105,
#1106,#1107,#1108,#1109,#1110,#1111),#1303,.T.);
#23380=ADVANCED_FACE('',(#2627),#23072,.T.);
#23381=ADVANCED_FACE('',(#2628,#1112,#1113,#1114,#1115,#1116,#1117,#1118,
#1119,#1120,#1121,#1122,#1123,#1124,#1125,#1126,#1127,#1128,#1129,#1130,
#1131,#1132,#1133,#1134,#1135,#1136,#1137,#1138,#1139,#1140,#1141,#1142,
#1143,#1144,#1145,#1146,#1147,#1148,#1149,#1150,#1151,#1152,#1153,#1154,
#1155,#1156),#1304,.T.);
#23382=ADVANCED_FACE('',(#2629),#2023,.F.);
#23383=ADVANCED_FACE('',(#2630),#2024,.F.);
#23384=ADVANCED_FACE('',(#2631),#1305,.F.);
#23385=ADVANCED_FACE('',(#2632),#2025,.F.);
#23386=ADVANCED_FACE('',(#2633),#1306,.F.);
#23387=ADVANCED_FACE('',(#2634),#2026,.F.);
#23388=ADVANCED_FACE('',(#2635),#1307,.F.);
#23389=ADVANCED_FACE('',(#2636),#2027,.F.);
#23390=ADVANCED_FACE('',(#2637),#1308,.F.);
#23391=ADVANCED_FACE('',(#2638),#1309,.F.);
#23392=ADVANCED_FACE('',(#2639),#2028,.F.);
#23393=ADVANCED_FACE('',(#2640),#2029,.F.);
#23394=ADVANCED_FACE('',(#2641),#1310,.F.);
#23395=ADVANCED_FACE('',(#2642),#2030,.F.);
#23396=ADVANCED_FACE('',(#2643),#1311,.F.);
#23397=ADVANCED_FACE('',(#2644),#1312,.F.);
#23398=ADVANCED_FACE('',(#2645),#2031,.F.);
#23399=ADVANCED_FACE('',(#2646),#2032,.F.);
#23400=ADVANCED_FACE('',(#2647),#2033,.F.);
#23401=ADVANCED_FACE('',(#2648),#1313,.F.);
#23402=ADVANCED_FACE('',(#2649),#2034,.F.);
#23403=ADVANCED_FACE('',(#2650),#1314,.F.);
#23404=ADVANCED_FACE('',(#2651),#1315,.F.);
#23405=ADVANCED_FACE('',(#2652),#2035,.F.);
#23406=ADVANCED_FACE('',(#2653),#2036,.F.);
#23407=ADVANCED_FACE('',(#2654),#1316,.F.);
#23408=ADVANCED_FACE('',(#2655),#2037,.F.);
#23409=ADVANCED_FACE('',(#2656),#1317,.F.);
#23410=ADVANCED_FACE('',(#2657),#1318,.F.);
#23411=ADVANCED_FACE('',(#2658),#2038,.F.);
#23412=ADVANCED_FACE('',(#2659),#2039,.F.);
#23413=ADVANCED_FACE('',(#2660),#1319,.F.);
#23414=ADVANCED_FACE('',(#2661),#2040,.F.);
#23415=ADVANCED_FACE('',(#2662),#1320,.F.);
#23416=ADVANCED_FACE('',(#2663),#1321,.F.);
#23417=ADVANCED_FACE('',(#2664),#2041,.F.);
#23418=ADVANCED_FACE('',(#2665),#2042,.F.);
#23419=ADVANCED_FACE('',(#2666),#1322,.F.);
#23420=ADVANCED_FACE('',(#2667),#2043,.F.);
#23421=ADVANCED_FACE('',(#2668),#1323,.F.);
#23422=ADVANCED_FACE('',(#2669),#1324,.F.);
#23423=ADVANCED_FACE('',(#2670),#2044,.F.);
#23424=ADVANCED_FACE('',(#2671),#2045,.F.);
#23425=ADVANCED_FACE('',(#2672),#1325,.F.);
#23426=ADVANCED_FACE('',(#2673),#2046,.F.);
#23427=ADVANCED_FACE('',(#2674),#1326,.F.);
#23428=ADVANCED_FACE('',(#2675),#1327,.F.);
#23429=ADVANCED_FACE('',(#2676),#2047,.F.);
#23430=ADVANCED_FACE('',(#2677),#2048,.F.);
#23431=ADVANCED_FACE('',(#2678),#1328,.F.);
#23432=ADVANCED_FACE('',(#2679),#1329,.F.);
#23433=ADVANCED_FACE('',(#2680),#2049,.F.);
#23434=ADVANCED_FACE('',(#2681),#1330,.F.);
#23435=ADVANCED_FACE('',(#2682),#2050,.F.);
#23436=ADVANCED_FACE('',(#2683),#1331,.F.);
#23437=ADVANCED_FACE('',(#2684),#2051,.F.);
#23438=ADVANCED_FACE('',(#2685),#1332,.F.);
#23439=ADVANCED_FACE('',(#2686),#1333,.F.);
#23440=ADVANCED_FACE('',(#2687),#2052,.F.);
#23441=ADVANCED_FACE('',(#2688),#2053,.F.);
#23442=ADVANCED_FACE('',(#2689),#1334,.F.);
#23443=ADVANCED_FACE('',(#2690),#2054,.F.);
#23444=ADVANCED_FACE('',(#2691),#1335,.F.);
#23445=ADVANCED_FACE('',(#2692),#1336,.F.);
#23446=ADVANCED_FACE('',(#2693),#2055,.F.);
#23447=ADVANCED_FACE('',(#2694),#2056,.F.);
#23448=ADVANCED_FACE('',(#2695),#1337,.F.);
#23449=ADVANCED_FACE('',(#2696),#2057,.F.);
#23450=ADVANCED_FACE('',(#2697),#1338,.F.);
#23451=ADVANCED_FACE('',(#2698),#1339,.F.);
#23452=ADVANCED_FACE('',(#2699),#2058,.F.);
#23453=ADVANCED_FACE('',(#2700),#2059,.F.);
#23454=ADVANCED_FACE('',(#2701),#1340,.F.);
#23455=ADVANCED_FACE('',(#2702),#2060,.F.);
#23456=ADVANCED_FACE('',(#2703),#1341,.F.);
#23457=ADVANCED_FACE('',(#2704),#1342,.F.);
#23458=ADVANCED_FACE('',(#2705),#2061,.F.);
#23459=ADVANCED_FACE('',(#2706),#2062,.F.);
#23460=ADVANCED_FACE('',(#2707),#1343,.F.);
#23461=ADVANCED_FACE('',(#2708),#2063,.F.);
#23462=ADVANCED_FACE('',(#2709),#1344,.F.);
#23463=ADVANCED_FACE('',(#2710),#1345,.F.);
#23464=ADVANCED_FACE('',(#2711),#2064,.F.);
#23465=ADVANCED_FACE('',(#2712),#2065,.F.);
#23466=ADVANCED_FACE('',(#2713),#1346,.F.);
#23467=ADVANCED_FACE('',(#2714),#2066,.F.);
#23468=ADVANCED_FACE('',(#2715),#1347,.F.);
#23469=ADVANCED_FACE('',(#2716),#1348,.F.);
#23470=ADVANCED_FACE('',(#2717),#2067,.F.);
#23471=ADVANCED_FACE('',(#2718),#2068,.F.);
#23472=ADVANCED_FACE('',(#2719),#2069,.F.);
#23473=ADVANCED_FACE('',(#2720),#1349,.F.);
#23474=ADVANCED_FACE('',(#2721),#2070,.F.);
#23475=ADVANCED_FACE('',(#2722),#1350,.F.);
#23476=ADVANCED_FACE('',(#2723),#1351,.F.);
#23477=ADVANCED_FACE('',(#2724),#2071,.F.);
#23478=ADVANCED_FACE('',(#2725),#2072,.F.);
#23479=ADVANCED_FACE('',(#2726),#1352,.F.);
#23480=ADVANCED_FACE('',(#2727),#2073,.F.);
#23481=ADVANCED_FACE('',(#2728),#1353,.F.);
#23482=ADVANCED_FACE('',(#2729),#1354,.F.);
#23483=ADVANCED_FACE('',(#2730),#2074,.F.);
#23484=ADVANCED_FACE('',(#2731),#2075,.F.);
#23485=ADVANCED_FACE('',(#2732),#1355,.F.);
#23486=ADVANCED_FACE('',(#2733),#1356,.F.);
#23487=ADVANCED_FACE('',(#2734),#2076,.F.);
#23488=ADVANCED_FACE('',(#2735),#1357,.F.);
#23489=ADVANCED_FACE('',(#2736),#2077,.F.);
#23490=ADVANCED_FACE('',(#2737),#1358,.F.);
#23491=ADVANCED_FACE('',(#2738),#2078,.F.);
#23492=ADVANCED_FACE('',(#2739),#1359,.F.);
#23493=ADVANCED_FACE('',(#2740),#1360,.F.);
#23494=ADVANCED_FACE('',(#2741),#2079,.F.);
#23495=ADVANCED_FACE('',(#2742),#2080,.F.);
#23496=ADVANCED_FACE('',(#2743),#1361,.F.);
#23497=ADVANCED_FACE('',(#2744),#2081,.F.);
#23498=ADVANCED_FACE('',(#2745),#1362,.F.);
#23499=ADVANCED_FACE('',(#2746),#1363,.F.);
#23500=ADVANCED_FACE('',(#2747),#2082,.F.);
#23501=ADVANCED_FACE('',(#2748),#2083,.F.);
#23502=ADVANCED_FACE('',(#2749),#2084,.F.);
#23503=ADVANCED_FACE('',(#2750),#1364,.F.);
#23504=ADVANCED_FACE('',(#2751),#1365,.F.);
#23505=ADVANCED_FACE('',(#2752),#2085,.F.);
#23506=ADVANCED_FACE('',(#2753),#1366,.F.);
#23507=ADVANCED_FACE('',(#2754),#2086,.F.);
#23508=ADVANCED_FACE('',(#2755),#1367,.F.);
#23509=ADVANCED_FACE('',(#2756),#1368,.F.);
#23510=ADVANCED_FACE('',(#2757),#2087,.F.);
#23511=ADVANCED_FACE('',(#2758),#2088,.F.);
#23512=ADVANCED_FACE('',(#2759),#1369,.F.);
#23513=ADVANCED_FACE('',(#2760),#2089,.F.);
#23514=ADVANCED_FACE('',(#2761),#1370,.F.);
#23515=ADVANCED_FACE('',(#2762),#1371,.F.);
#23516=ADVANCED_FACE('',(#2763),#2090,.F.);
#23517=ADVANCED_FACE('',(#2764),#2091,.F.);
#23518=ADVANCED_FACE('',(#2765),#1372,.F.);
#23519=ADVANCED_FACE('',(#2766),#2092,.F.);
#23520=ADVANCED_FACE('',(#2767),#1373,.F.);
#23521=ADVANCED_FACE('',(#2768),#1374,.F.);
#23522=ADVANCED_FACE('',(#2769),#2093,.F.);
#23523=ADVANCED_FACE('',(#2770),#2094,.F.);
#23524=ADVANCED_FACE('',(#2771),#1375,.F.);
#23525=ADVANCED_FACE('',(#2772),#1376,.F.);
#23526=ADVANCED_FACE('',(#2773),#2095,.F.);
#23527=ADVANCED_FACE('',(#2774),#1377,.F.);
#23528=ADVANCED_FACE('',(#2775),#2096,.F.);
#23529=ADVANCED_FACE('',(#2776),#1378,.F.);
#23530=ADVANCED_FACE('',(#2777),#2097,.F.);
#23531=ADVANCED_FACE('',(#2778),#1379,.F.);
#23532=ADVANCED_FACE('',(#2779),#1380,.F.);
#23533=ADVANCED_FACE('',(#2780),#2098,.F.);
#23534=ADVANCED_FACE('',(#2781),#1381,.F.);
#23535=ADVANCED_FACE('',(#2782),#2099,.F.);
#23536=ADVANCED_FACE('',(#2783),#1382,.F.);
#23537=ADVANCED_FACE('',(#2784),#1383,.F.);
#23538=ADVANCED_FACE('',(#2785),#2100,.F.);
#23539=ADVANCED_FACE('',(#2786),#1384,.F.);
#23540=ADVANCED_FACE('',(#2787),#2101,.F.);
#23541=ADVANCED_FACE('',(#2788),#2102,.F.);
#23542=ADVANCED_FACE('',(#2789),#2103,.F.);
#23543=ADVANCED_FACE('',(#2790),#2104,.F.);
#23544=ADVANCED_FACE('',(#2791),#2105,.F.);
#23545=ADVANCED_FACE('',(#2792),#2106,.F.);
#23546=ADVANCED_FACE('',(#2793),#2107,.F.);
#23547=ADVANCED_FACE('',(#2794),#2108,.F.);
#23548=ADVANCED_FACE('',(#2795),#2109,.F.);
#23549=ADVANCED_FACE('',(#2796),#2110,.F.);
#23550=ADVANCED_FACE('',(#2797),#2111,.F.);
#23551=ADVANCED_FACE('',(#2798),#2112,.F.);
#23552=ADVANCED_FACE('',(#2799),#1385,.F.);
#23553=ADVANCED_FACE('',(#2800),#1386,.F.);
#23554=ADVANCED_FACE('',(#2801),#1387,.F.);
#23555=ADVANCED_FACE('',(#2802),#1388,.F.);
#23556=ADVANCED_FACE('',(#2803),#1389,.F.);
#23557=ADVANCED_FACE('',(#2804),#1390,.F.);
#23558=ADVANCED_FACE('',(#2805),#1391,.F.);
#23559=ADVANCED_FACE('',(#2806),#1392,.F.);
#23560=ADVANCED_FACE('',(#2807),#1393,.F.);
#23561=ADVANCED_FACE('',(#2808),#1394,.F.);
#23562=ADVANCED_FACE('',(#2809),#1395,.F.);
#23563=ADVANCED_FACE('',(#2810),#1396,.F.);
#23564=ADVANCED_FACE('',(#2811),#1397,.F.);
#23565=ADVANCED_FACE('',(#2812),#1398,.F.);
#23566=ADVANCED_FACE('',(#2813),#1399,.F.);
#23567=ADVANCED_FACE('',(#2814),#1400,.F.);
#23568=ADVANCED_FACE('',(#2815),#1401,.F.);
#23569=ADVANCED_FACE('',(#2816),#1402,.F.);
#23570=ADVANCED_FACE('',(#2817),#1403,.F.);
#23571=ADVANCED_FACE('',(#2818),#1404,.F.);
#23572=ADVANCED_FACE('',(#2819),#1405,.F.);
#23573=ADVANCED_FACE('',(#2820),#1406,.F.);
#23574=ADVANCED_FACE('',(#2821),#1407,.F.);
#23575=ADVANCED_FACE('',(#2822),#1408,.F.);
#23576=ADVANCED_FACE('',(#2823),#1409,.F.);
#23577=ADVANCED_FACE('',(#2824),#1410,.F.);
#23578=ADVANCED_FACE('',(#2825),#1411,.F.);
#23579=ADVANCED_FACE('',(#2826),#1412,.F.);
#23580=ADVANCED_FACE('',(#2827),#2113,.F.);
#23581=ADVANCED_FACE('',(#2828,#1157),#1413,.T.);
#23582=ADVANCED_FACE('',(#2829),#2114,.T.);
#23583=ADVANCED_FACE('',(#2830),#2115,.F.);
#23584=ADVANCED_FACE('',(#2831),#23073,.T.);
#23585=ADVANCED_FACE('',(#2832),#2116,.T.);
#23586=ADVANCED_FACE('',(#2833,#1158),#1414,.T.);
#23587=ADVANCED_FACE('',(#2834),#23074,.T.);
#23588=ADVANCED_FACE('',(#2835,#1159),#1415,.T.);
#23589=ADVANCED_FACE('',(#2836),#23075,.F.);
#23590=ADVANCED_FACE('',(#2837),#23076,.F.);
#23591=ADVANCED_FACE('',(#2838,#1160),#1416,.T.);
#23592=ADVANCED_FACE('',(#2839),#23077,.F.);
#23593=ADVANCED_FACE('',(#2840),#2117,.F.);
#23594=ADVANCED_FACE('',(#2841),#23078,.F.);
#23595=ADVANCED_FACE('',(#2842),#23079,.F.);
#23596=ADVANCED_FACE('',(#2843),#23080,.F.);
#23597=ADVANCED_FACE('',(#2844,#1161),#1417,.T.);
#23598=ADVANCED_FACE('',(#2845),#23081,.T.);
#23599=ADVANCED_FACE('',(#2846),#2118,.T.);
#23600=ADVANCED_FACE('',(#2847),#954,.T.);
#23601=ADVANCED_FACE('',(#2848),#2119,.T.);
#23602=ADVANCED_FACE('',(#2849),#955,.T.);
#23603=ADVANCED_FACE('',(#2850),#23082,.T.);
#23604=ADVANCED_FACE('',(#2851),#2120,.T.);
#23605=ADVANCED_FACE('',(#2852),#23083,.F.);
#23606=ADVANCED_FACE('',(#2853,#1162,#1163,#1164),#1418,.T.);
#23607=ADVANCED_FACE('',(#2854),#2121,.F.);
#23608=ADVANCED_FACE('',(#2855),#23084,.T.);
#23609=ADVANCED_FACE('',(#2856),#23085,.T.);
#23610=ADVANCED_FACE('',(#2857),#23086,.T.);
#23611=ADVANCED_FACE('',(#2858),#2122,.T.);
#23612=ADVANCED_FACE('',(#2859),#23087,.T.);
#23613=ADVANCED_FACE('',(#2860),#23088,.T.);
#23614=ADVANCED_FACE('',(#2861),#23089,.F.);
#23615=ADVANCED_FACE('',(#2862),#2123,.F.);
#23616=ADVANCED_FACE('',(#2863,#1165),#1419,.T.);
#23617=ADVANCED_FACE('',(#2864),#23090,.T.);
#23618=ADVANCED_FACE('',(#2865),#23091,.F.);
#23619=ADVANCED_FACE('',(#2866),#2124,.F.);
#23620=ADVANCED_FACE('',(#2867),#23092,.F.);
#23621=ADVANCED_FACE('',(#2868),#2125,.F.);
#23622=ADVANCED_FACE('',(#2869),#23093,.F.);
#23623=ADVANCED_FACE('',(#2870),#2126,.F.);
#23624=ADVANCED_FACE('',(#2871),#23094,.F.);
#23625=ADVANCED_FACE('',(#2872,#1166),#1420,.F.);
#23626=ADVANCED_FACE('',(#2873),#23095,.F.);
#23627=ADVANCED_FACE('',(#2874),#2127,.F.);
#23628=ADVANCED_FACE('',(#2875),#23096,.F.);
#23629=ADVANCED_FACE('',(#2876,#1167),#1421,.F.);
#23630=ADVANCED_FACE('',(#2877),#23097,.F.);
#23631=ADVANCED_FACE('',(#2878,#1168),#1422,.T.);
#23632=ADVANCED_FACE('',(#2879),#2128,.F.);
#23633=ADVANCED_FACE('',(#2880),#2129,.F.);
#23634=ADVANCED_FACE('',(#2881),#2130,.F.);
#23635=ADVANCED_FACE('',(#2882),#23098,.F.);
#23636=ADVANCED_FACE('',(#2883),#2131,.F.);
#23637=ADVANCED_FACE('',(#2884),#2132,.F.);
#23638=ADVANCED_FACE('',(#2885),#2133,.F.);
#23639=ADVANCED_FACE('',(#2886),#2134,.F.);
#23640=ADVANCED_FACE('',(#2887),#2135,.F.);
#23641=ADVANCED_FACE('',(#2888),#2136,.F.);
#23642=ADVANCED_FACE('',(#2889),#23099,.F.);
#23643=ADVANCED_FACE('',(#2890),#2137,.F.);
#23644=ADVANCED_FACE('',(#2891,#1169,#1170,#1171,#1172,#1173,#1174,#1175,
#1176,#1177,#1178),#1423,.T.);
#23645=ADVANCED_FACE('',(#2892),#23100,.F.);
#23646=ADVANCED_FACE('',(#2893,#1179,#1180,#1181,#1182,#1183,#1184,#1185,
#1186,#1187,#1188),#1424,.T.);
#23647=ADVANCED_FACE('',(#2894),#23101,.T.);
#23648=ADVANCED_FACE('',(#2895),#2138,.T.);
#23649=ADVANCED_FACE('',(#2896),#23102,.T.);
#23650=ADVANCED_FACE('',(#2897),#23103,.F.);
#23651=ADVANCED_FACE('',(#2898),#2139,.F.);
#23652=ADVANCED_FACE('',(#2899),#23104,.F.);
#23653=ADVANCED_FACE('',(#2900),#2140,.F.);
#23654=ADVANCED_FACE('',(#2901),#2141,.T.);
#23655=ADVANCED_FACE('',(#2902),#1425,.F.);
#23656=ADVANCED_FACE('',(#2903,#1189),#1426,.T.);
#23657=ADVANCED_FACE('',(#2904),#23105,.T.);
#23658=ADVANCED_FACE('',(#2905),#2142,.T.);
#23659=ADVANCED_FACE('',(#2906),#2143,.T.);
#23660=ADVANCED_FACE('',(#2907,#1190),#1427,.F.);
#23661=ADVANCED_FACE('',(#2908,#1191),#1428,.F.);
#23662=ADVANCED_FACE('',(#2909),#2144,.T.);
#23663=ADVANCED_FACE('',(#2910,#1192),#1429,.T.);
#23664=ADVANCED_FACE('',(#2911),#23106,.T.);
#23665=ADVANCED_FACE('',(#2912),#2145,.T.);
#23666=ADVANCED_FACE('',(#2913),#23107,.T.);
#23667=ADVANCED_FACE('',(#2914,#1193,#1194,#1195),#1430,.T.);
#23668=ADVANCED_FACE('',(#2915),#2146,.T.);
#23669=ADVANCED_FACE('',(#2916,#1196),#1431,.T.);
#23670=ADVANCED_FACE('',(#2917),#2147,.T.);
#23671=ADVANCED_FACE('',(#2918),#23108,.T.);
#23672=ADVANCED_FACE('',(#2919),#1432,.T.);
#23673=ADVANCED_FACE('',(#2920),#23109,.T.);
#23674=ADVANCED_FACE('',(#2921,#1197),#1433,.T.);
#23675=ADVANCED_FACE('',(#2922),#2148,.T.);
#23676=ADVANCED_FACE('',(#2923),#23110,.F.);
#23677=ADVANCED_FACE('',(#2924),#2149,.F.);
#23678=ADVANCED_FACE('',(#2925),#23111,.F.);
#23679=ADVANCED_FACE('',(#2926),#467,.T.);
#23680=ADVANCED_FACE('',(#2927,#1198),#1434,.T.);
#23681=ADVANCED_FACE('',(#2928),#468,.T.);
#23682=ADVANCED_FACE('',(#2929),#2150,.T.);
#23683=ADVANCED_FACE('',(#2930),#23112,.T.);
#23684=ADVANCED_FACE('',(#2931),#2151,.F.);
#23685=ADVANCED_FACE('',(#2932),#469,.T.);
#23686=ADVANCED_FACE('',(#2933),#23113,.F.);
#23687=ADVANCED_FACE('',(#2934),#2152,.F.);
#23688=ADVANCED_FACE('',(#2935,#1199,#1200,#1201,#1202),#1435,.T.);
#23689=ADVANCED_FACE('',(#2936),#23114,.F.);
#23690=ADVANCED_FACE('',(#2937,#1203,#1204,#1205,#1206),#1436,.T.);
#23691=ADVANCED_FACE('',(#2938),#23115,.F.);
#23692=ADVANCED_FACE('',(#2939),#2153,.F.);
#23693=ADVANCED_FACE('',(#2940),#23116,.F.);
#23694=ADVANCED_FACE('',(#2941),#23117,.F.);
#23695=ADVANCED_FACE('',(#2942),#2154,.F.);
#23696=ADVANCED_FACE('',(#2943),#23118,.F.);
#23697=ADVANCED_FACE('',(#2944),#1437,.F.);
#23698=ADVANCED_FACE('',(#2945),#1438,.F.);
#23699=ADVANCED_FACE('',(#2946),#23119,.T.);
#23700=ADVANCED_FACE('',(#2947),#2155,.T.);
#23701=ADVANCED_FACE('',(#2948),#23120,.T.);
#23702=ADVANCED_FACE('',(#2949),#23121,.F.);
#23703=ADVANCED_FACE('',(#2950),#2156,.F.);
#23704=ADVANCED_FACE('',(#2951,#1207),#1439,.T.);
#23705=ADVANCED_FACE('',(#2952),#23122,.F.);
#23706=ADVANCED_FACE('',(#2953,#1208,#1209,#1210,#1211),#1440,.T.);
#23707=ADVANCED_FACE('',(#2954),#23123,.T.);
#23708=ADVANCED_FACE('',(#2955),#2157,.T.);
#23709=ADVANCED_FACE('',(#2956),#23124,.F.);
#23710=ADVANCED_FACE('',(#2957),#2158,.F.);
#23711=ADVANCED_FACE('',(#2958),#23125,.F.);
#23712=ADVANCED_FACE('',(#2959),#23126,.F.);
#23713=ADVANCED_FACE('',(#2960),#2159,.F.);
#23714=ADVANCED_FACE('',(#2961),#23127,.F.);
#23715=ADVANCED_FACE('',(#2962),#23128,.F.);
#23716=ADVANCED_FACE('',(#2963),#2160,.F.);
#23717=ADVANCED_FACE('',(#2964),#23129,.F.);
#23718=ADVANCED_FACE('',(#2965),#23130,.T.);
#23719=ADVANCED_FACE('',(#2966),#1441,.F.);
#23720=ADVANCED_FACE('',(#2967),#1442,.F.);
#23721=ADVANCED_FACE('',(#2968),#1443,.F.);
#23722=ADVANCED_FACE('',(#2969,#1212,#1213,#1214,#1215,#1216,#1217,#1218,
#1219,#1220,#1221),#1444,.T.);
#23723=ADVANCED_FACE('',(#2970),#2161,.T.);
#23724=ADVANCED_FACE('',(#2971),#2162,.F.);
#23725=ADVANCED_FACE('',(#2972),#2163,.F.);
#23726=ADVANCED_FACE('',(#2973),#2164,.F.);
#23727=ADVANCED_FACE('',(#2974),#1445,.F.);
#23728=ADVANCED_FACE('',(#2975),#2165,.T.);
#23729=ADVANCED_FACE('',(#2976),#1446,.F.);
#23730=ADVANCED_FACE('',(#2977),#2166,.F.);
#23731=ADVANCED_FACE('',(#2978),#1447,.F.);
#23732=ADVANCED_FACE('',(#2979),#2167,.T.);
#23733=ADVANCED_FACE('',(#2980),#1448,.F.);
#23734=ADVANCED_FACE('',(#2981),#2168,.F.);
#23735=ADVANCED_FACE('',(#2982),#1449,.F.);
#23736=ADVANCED_FACE('',(#2983),#2169,.T.);
#23737=ADVANCED_FACE('',(#2984),#1450,.F.);
#23738=ADVANCED_FACE('',(#2985),#2170,.F.);
#23739=ADVANCED_FACE('',(#2986),#1451,.F.);
#23740=ADVANCED_FACE('',(#2987),#2171,.T.);
#23741=ADVANCED_FACE('',(#2988),#1452,.F.);
#23742=ADVANCED_FACE('',(#2989),#2172,.F.);
#23743=ADVANCED_FACE('',(#2990),#1453,.F.);
#23744=ADVANCED_FACE('',(#2991),#2173,.T.);
#23745=ADVANCED_FACE('',(#2992),#1454,.F.);
#23746=ADVANCED_FACE('',(#2993),#2174,.F.);
#23747=ADVANCED_FACE('',(#2994),#1455,.F.);
#23748=ADVANCED_FACE('',(#2995),#2175,.T.);
#23749=ADVANCED_FACE('',(#2996),#1456,.F.);
#23750=ADVANCED_FACE('',(#2997),#2176,.F.);
#23751=ADVANCED_FACE('',(#2998),#2177,.F.);
#23752=ADVANCED_FACE('',(#2999,#1222,#1223,#1224,#1225,#1226,#1227,#1228,
#1229,#1230,#1231),#1457,.T.);
#23753=ADVANCED_FACE('',(#3000),#1458,.T.);
#23754=ADVANCED_FACE('',(#3001),#1459,.T.);
#23755=ADVANCED_FACE('',(#3002),#1460,.T.);
#23756=ADVANCED_FACE('',(#3003),#1461,.T.);
#23757=ADVANCED_FACE('',(#3004),#1462,.T.);
#23758=ADVANCED_FACE('',(#3005),#1463,.T.);
#23759=ADVANCED_FACE('',(#3006),#1464,.T.);
#23760=ADVANCED_FACE('',(#3007,#1232),#1465,.T.);
#23761=ADVANCED_FACE('',(#3008),#1466,.T.);
#23762=ADVANCED_FACE('',(#3009),#1467,.F.);
#23763=ADVANCED_FACE('',(#3010),#1468,.T.);
#23764=ADVANCED_FACE('',(#3011,#1233),#1469,.F.);
#23765=ADVANCED_FACE('',(#3012),#1470,.T.);
#23766=ADVANCED_FACE('',(#3013),#1471,.T.);
#23767=ADVANCED_FACE('',(#3014,#1234,#1235,#1236),#1472,.T.);
#23768=ADVANCED_FACE('',(#3015),#1473,.T.);
#23769=ADVANCED_FACE('',(#3016),#1474,.F.);
#23770=ADVANCED_FACE('',(#3017),#2178,.F.);
#23771=ADVANCED_FACE('',(#3018),#2179,.F.);
#23772=ADVANCED_FACE('',(#3019),#1475,.T.);
#23773=ADVANCED_FACE('',(#3020,#1237,#1238),#1476,.T.);
#23774=ADVANCED_FACE('',(#3021),#1477,.T.);
#23775=ADVANCED_FACE('',(#3022),#1478,.T.);
#23776=ADVANCED_FACE('',(#3023),#1479,.F.);
#23777=ADVANCED_FACE('',(#3024),#1480,.F.);
#23778=ADVANCED_FACE('',(#3025),#1481,.F.);
#23779=ADVANCED_FACE('',(#3026),#1482,.F.);
#23780=ADVANCED_FACE('',(#3027),#1483,.F.);
#23781=ADVANCED_FACE('',(#3028),#1484,.T.);
#23782=ADVANCED_FACE('',(#3029),#1485,.F.);
#23783=ADVANCED_FACE('',(#3030),#1486,.F.);
#23784=ADVANCED_FACE('',(#3031),#1487,.F.);
#23785=ADVANCED_FACE('',(#3032),#1488,.F.);
#23786=ADVANCED_FACE('',(#3033),#1489,.F.);
#23787=ADVANCED_FACE('',(#3034),#1490,.T.);
#23788=ADVANCED_FACE('',(#3035),#2180,.T.);
#23789=ADVANCED_FACE('',(#3036),#1491,.T.);
#23790=ADVANCED_FACE('',(#3037),#1492,.T.);
#23791=ADVANCED_FACE('',(#3038),#2181,.T.);
#23792=ADVANCED_FACE('',(#3039),#2182,.F.);
#23793=ADVANCED_FACE('',(#3040),#2183,.F.);
#23794=ADVANCED_FACE('',(#3041),#1493,.F.);
#23795=ADVANCED_FACE('',(#3042),#2184,.F.);
#23796=ADVANCED_FACE('',(#3043),#1494,.F.);
#23797=ADVANCED_FACE('',(#3044),#2185,.F.);
#23798=ADVANCED_FACE('',(#3045),#1495,.F.);
#23799=ADVANCED_FACE('',(#3046),#2186,.F.);
#23800=ADVANCED_FACE('',(#3047),#1496,.T.);
#23801=ADVANCED_FACE('',(#3048),#1497,.T.);
#23802=ADVANCED_FACE('',(#3049),#1498,.T.);
#23803=ADVANCED_FACE('',(#3050,#1239,#1240),#1499,.T.);
#23804=ADVANCED_FACE('',(#3051),#1500,.T.);
#23805=ADVANCED_FACE('',(#3052,#1241,#1242),#1501,.T.);
#23806=ADVANCED_FACE('',(#3053),#1502,.T.);
#23807=ADVANCED_FACE('',(#3054,#1243),#1503,.F.);
#23808=ADVANCED_FACE('',(#3055),#1504,.T.);
#23809=ADVANCED_FACE('',(#3056),#1505,.T.);
#23810=ADVANCED_FACE('',(#3057),#1506,.T.);
#23811=ADVANCED_FACE('',(#3058),#1507,.T.);
#23812=ADVANCED_FACE('',(#3059),#1508,.T.);
#23813=ADVANCED_FACE('',(#3060),#1509,.T.);
#23814=ADVANCED_FACE('',(#3061),#1510,.T.);
#23815=ADVANCED_FACE('',(#3062),#1511,.T.);
#23816=ADVANCED_FACE('',(#3063),#1512,.T.);
#23817=ADVANCED_FACE('',(#3064),#1513,.T.);
#23818=ADVANCED_FACE('',(#3065),#2187,.T.);
#23819=ADVANCED_FACE('',(#3066),#1514,.T.);
#23820=ADVANCED_FACE('',(#3067),#1515,.T.);
#23821=ADVANCED_FACE('',(#3068),#1516,.T.);
#23822=ADVANCED_FACE('',(#3069),#1517,.T.);
#23823=ADVANCED_FACE('',(#3070),#1518,.T.);
#23824=ADVANCED_FACE('',(#3071),#1519,.T.);
#23825=ADVANCED_FACE('',(#3072),#1520,.T.);
#23826=ADVANCED_FACE('',(#3073),#1521,.T.);
#23827=ADVANCED_FACE('',(#3074),#1522,.T.);
#23828=ADVANCED_FACE('',(#3075),#1523,.T.);
#23829=ADVANCED_FACE('',(#3076),#1524,.T.);
#23830=ADVANCED_FACE('',(#3077),#1525,.T.);
#23831=ADVANCED_FACE('',(#3078),#1526,.T.);
#23832=ADVANCED_FACE('',(#3079),#1527,.T.);
#23833=ADVANCED_FACE('',(#3080),#1528,.T.);
#23834=ADVANCED_FACE('',(#3081),#1529,.T.);
#23835=ADVANCED_FACE('',(#3082),#1530,.T.);
#23836=ADVANCED_FACE('',(#3083),#1531,.T.);
#23837=ADVANCED_FACE('',(#3084),#1532,.T.);
#23838=ADVANCED_FACE('',(#3085),#1533,.T.);
#23839=ADVANCED_FACE('',(#3086),#1534,.T.);
#23840=ADVANCED_FACE('',(#3087),#2188,.F.);
#23841=ADVANCED_FACE('',(#3088),#2189,.F.);
#23842=ADVANCED_FACE('',(#3089),#2190,.F.);
#23843=ADVANCED_FACE('',(#3090),#2191,.F.);
#23844=ADVANCED_FACE('',(#3091,#1244,#1245,#1246,#1247),#1535,.T.);
#23845=ADVANCED_FACE('',(#3092),#2192,.T.);
#23846=ADVANCED_FACE('',(#3093,#1248,#1249,#1250,#1251,#1252,#1253,#1254,
#1255,#1256,#1257,#1258),#1536,.T.);
#23847=ADVANCED_FACE('',(#3094),#2193,.T.);
#23848=ADVANCED_FACE('',(#3095),#2194,.T.);
#23849=ADVANCED_FACE('',(#3096),#2195,.T.);
#23850=ADVANCED_FACE('',(#3097),#2196,.T.);
#23851=ADVANCED_FACE('',(#3098),#2197,.T.);
#23852=ADVANCED_FACE('',(#3099),#2198,.T.);
#23853=ADVANCED_FACE('',(#3100),#2199,.T.);
#23854=ADVANCED_FACE('',(#3101),#1537,.F.);
#23855=ADVANCED_FACE('',(#3102),#470,.F.);
#23856=ADVANCED_FACE('',(#3103),#1538,.T.);
#23857=ADVANCED_FACE('',(#3104),#2200,.T.);
#23858=ADVANCED_FACE('',(#3105),#471,.F.);
#23859=ADVANCED_FACE('',(#3106),#2201,.T.);
#23860=ADVANCED_FACE('',(#3107),#23131,.F.);
#23861=ADVANCED_FACE('',(#3108),#1539,.F.);
#23862=ADVANCED_FACE('',(#3109),#1540,.F.);
#23863=ADVANCED_FACE('',(#3110),#1541,.F.);
#23864=ADVANCED_FACE('',(#3111),#1542,.F.);
#23865=ADVANCED_FACE('',(#3112),#1543,.F.);
#23866=ADVANCED_FACE('',(#3113),#1544,.F.);
#23867=ADVANCED_FACE('',(#3114,#1259),#1545,.F.);
#23868=ADVANCED_FACE('',(#3115),#1546,.T.);
#23869=ADVANCED_FACE('',(#3116),#23132,.T.);
#23870=ADVANCED_FACE('',(#3117),#23133,.T.);
#23871=ADVANCED_FACE('',(#3118,#1260),#1547,.T.);
#23872=ADVANCED_FACE('',(#3119),#2202,.T.);
#23873=ADVANCED_FACE('',(#3120),#2203,.T.);
#23874=ADVANCED_FACE('',(#3121),#2204,.T.);
#23875=ADVANCED_FACE('',(#3122),#2205,.T.);
#23876=ADVANCED_FACE('',(#3123),#2206,.T.);
#23877=ADVANCED_FACE('',(#3124),#2207,.T.);
#23878=ADVANCED_FACE('',(#3125),#2208,.T.);
#23879=ADVANCED_FACE('',(#3126),#2209,.T.);
#23880=ADVANCED_FACE('',(#3127),#2210,.T.);
#23881=ADVANCED_FACE('',(#3128),#2211,.T.);
#23882=ADVANCED_FACE('',(#3129),#2212,.T.);
#23883=ADVANCED_FACE('',(#3130),#2213,.T.);
#23884=ADVANCED_FACE('',(#3131),#2214,.T.);
#23885=ADVANCED_FACE('',(#3132),#2215,.T.);
#23886=ADVANCED_FACE('',(#3133),#2216,.T.);
#23887=ADVANCED_FACE('',(#3134),#2217,.T.);
#23888=ADVANCED_FACE('',(#3135),#472,.F.);
#23889=ADVANCED_FACE('',(#3136),#1548,.T.);
#23890=ADVANCED_FACE('',(#3137),#2218,.T.);
#23891=ADVANCED_FACE('',(#3138),#473,.F.);
#23892=ADVANCED_FACE('',(#3139),#2219,.T.);
#23893=ADVANCED_FACE('',(#3140),#23134,.F.);
#23894=ADVANCED_FACE('',(#3141),#2220,.F.);
#23895=ADVANCED_FACE('',(#3142),#23135,.F.);
#23896=ADVANCED_FACE('',(#3143),#23136,.T.);
#23897=ADVANCED_FACE('',(#3144),#23137,.T.);
#23898=ADVANCED_FACE('',(#3145),#23138,.T.);
#23899=ADVANCED_FACE('',(#3146),#23139,.T.);
#23900=ADVANCED_FACE('',(#3147),#23140,.T.);
#23901=ADVANCED_FACE('',(#3148),#23141,.T.);
#23902=ADVANCED_FACE('',(#3149),#1549,.T.);
#23903=ADVANCED_FACE('',(#3150),#1550,.T.);
#23904=ADVANCED_FACE('',(#3151),#1551,.T.);
#23905=ADVANCED_FACE('',(#3152,#1261),#1552,.F.);
#23906=ADVANCED_FACE('',(#3153),#1553,.T.);
#23907=ADVANCED_FACE('',(#3154),#23142,.T.);
#23908=ADVANCED_FACE('',(#3155),#23143,.T.);
#23909=ADVANCED_FACE('',(#3156),#23144,.T.);
#23910=ADVANCED_FACE('',(#3157),#23145,.T.);
#23911=ADVANCED_FACE('',(#3158),#23146,.T.);
#23912=ADVANCED_FACE('',(#3159),#23147,.T.);
#23913=ADVANCED_FACE('',(#3160),#1554,.T.);
#23914=ADVANCED_FACE('',(#3161),#1555,.T.);
#23915=ADVANCED_FACE('',(#3162),#23148,.T.);
#23916=ADVANCED_FACE('',(#3163),#1556,.T.);
#23917=ADVANCED_FACE('',(#3164,#1262),#1557,.T.);
#23918=ADVANCED_FACE('',(#3165),#2221,.T.);
#23919=ADVANCED_FACE('',(#3166),#2222,.T.);
#23920=ADVANCED_FACE('',(#3167),#2223,.T.);
#23921=ADVANCED_FACE('',(#3168),#2224,.T.);
#23922=ADVANCED_FACE('',(#3169),#2225,.T.);
#23923=ADVANCED_FACE('',(#3170),#2226,.T.);
#23924=ADVANCED_FACE('',(#3171),#2227,.T.);
#23925=ADVANCED_FACE('',(#3172),#2228,.T.);
#23926=ADVANCED_FACE('',(#3173),#2229,.T.);
#23927=ADVANCED_FACE('',(#3174),#2230,.T.);
#23928=ADVANCED_FACE('',(#3175),#2231,.T.);
#23929=ADVANCED_FACE('',(#3176),#2232,.T.);
#23930=ADVANCED_FACE('',(#3177),#2233,.T.);
#23931=ADVANCED_FACE('',(#3178),#2234,.T.);
#23932=ADVANCED_FACE('',(#3179),#2235,.T.);
#23933=ADVANCED_FACE('',(#3180),#2236,.T.);
#23934=ADVANCED_FACE('',(#3181),#2237,.T.);
#23935=ADVANCED_FACE('',(#3182),#2238,.T.);
#23936=ADVANCED_FACE('',(#3183),#2239,.T.);
#23937=ADVANCED_FACE('',(#3184),#2240,.T.);
#23938=ADVANCED_FACE('',(#3185),#2241,.T.);
#23939=ADVANCED_FACE('',(#3186),#2242,.T.);
#23940=ADVANCED_FACE('',(#3187),#2243,.T.);
#23941=ADVANCED_FACE('',(#3188),#2244,.T.);
#23942=ADVANCED_FACE('',(#3189),#2245,.T.);
#23943=ADVANCED_FACE('',(#3190),#2246,.T.);
#23944=ADVANCED_FACE('',(#3191),#2247,.T.);
#23945=ADVANCED_FACE('',(#3192),#2248,.T.);
#23946=ADVANCED_FACE('',(#3193),#2249,.T.);
#23947=ADVANCED_FACE('',(#3194),#2250,.T.);
#23948=ADVANCED_FACE('',(#3195),#2251,.T.);
#23949=ADVANCED_FACE('',(#3196),#2252,.T.);
#23950=ADVANCED_FACE('',(#3197),#2253,.T.);
#23951=ADVANCED_FACE('',(#3198),#2254,.T.);
#23952=ADVANCED_FACE('',(#3199),#2255,.T.);
#23953=ADVANCED_FACE('',(#3200),#2256,.T.);
#23954=ADVANCED_FACE('',(#3201),#2257,.T.);
#23955=ADVANCED_FACE('',(#3202),#2258,.T.);
#23956=ADVANCED_FACE('',(#3203),#2259,.T.);
#23957=ADVANCED_FACE('',(#3204),#2260,.T.);
#23958=ADVANCED_FACE('',(#3205),#2261,.T.);
#23959=ADVANCED_FACE('',(#3206),#2262,.T.);
#23960=ADVANCED_FACE('',(#3207),#2263,.T.);
#23961=ADVANCED_FACE('',(#3208),#2264,.T.);
#23962=ADVANCED_FACE('',(#3209),#2265,.T.);
#23963=ADVANCED_FACE('',(#3210),#2266,.T.);
#23964=ADVANCED_FACE('',(#3211),#2267,.T.);
#23965=ADVANCED_FACE('',(#3212),#2268,.T.);
#23966=ADVANCED_FACE('',(#3213),#2269,.T.);
#23967=ADVANCED_FACE('',(#3214),#2270,.T.);
#23968=ADVANCED_FACE('',(#3215),#2271,.T.);
#23969=ADVANCED_FACE('',(#3216),#2272,.T.);
#23970=ADVANCED_FACE('',(#3217),#2273,.T.);
#23971=ADVANCED_FACE('',(#3218),#2274,.T.);
#23972=ADVANCED_FACE('',(#3219),#2275,.T.);
#23973=ADVANCED_FACE('',(#3220),#2276,.T.);
#23974=ADVANCED_FACE('',(#3221),#2277,.T.);
#23975=ADVANCED_FACE('',(#3222),#1558,.F.);
#23976=ADVANCED_FACE('',(#3223),#474,.F.);
#23977=ADVANCED_FACE('',(#3224),#1559,.T.);
#23978=ADVANCED_FACE('',(#3225),#2278,.T.);
#23979=ADVANCED_FACE('',(#3226),#475,.F.);
#23980=ADVANCED_FACE('',(#3227),#1560,.T.);
#23981=ADVANCED_FACE('',(#3228),#1561,.F.);
#23982=ADVANCED_FACE('',(#3229),#1562,.F.);
#23983=ADVANCED_FACE('',(#3230),#1563,.T.);
#23984=ADVANCED_FACE('',(#3231),#1564,.F.);
#23985=ADVANCED_FACE('',(#3232),#1565,.F.);
#23986=ADVANCED_FACE('',(#3233),#1566,.T.);
#23987=ADVANCED_FACE('',(#3234),#1567,.F.);
#23988=ADVANCED_FACE('',(#3235),#1568,.F.);
#23989=ADVANCED_FACE('',(#3236),#1569,.T.);
#23990=ADVANCED_FACE('',(#3237),#1570,.F.);
#23991=ADVANCED_FACE('',(#3238),#1571,.F.);
#23992=ADVANCED_FACE('',(#3239),#1572,.T.);
#23993=ADVANCED_FACE('',(#3240),#1573,.F.);
#23994=ADVANCED_FACE('',(#3241),#1574,.F.);
#23995=ADVANCED_FACE('',(#3242),#1575,.T.);
#23996=ADVANCED_FACE('',(#3243),#1576,.F.);
#23997=ADVANCED_FACE('',(#3244),#1577,.F.);
#23998=ADVANCED_FACE('',(#3245),#1578,.T.);
#23999=ADVANCED_FACE('',(#3246),#1579,.F.);
#24000=ADVANCED_FACE('',(#3247),#1580,.F.);
#24001=ADVANCED_FACE('',(#3248),#1581,.T.);
#24002=ADVANCED_FACE('',(#3249),#1582,.F.);
#24003=ADVANCED_FACE('',(#3250),#1583,.F.);
#24004=ADVANCED_FACE('',(#3251),#1584,.T.);
#24005=ADVANCED_FACE('',(#3252),#1585,.F.);
#24006=ADVANCED_FACE('',(#3253),#1586,.F.);
#24007=ADVANCED_FACE('',(#3254),#1587,.T.);
#24008=ADVANCED_FACE('',(#3255),#1588,.F.);
#24009=ADVANCED_FACE('',(#3256),#1589,.F.);
#24010=ADVANCED_FACE('',(#3257),#1590,.T.);
#24011=ADVANCED_FACE('',(#3258),#1591,.F.);
#24012=ADVANCED_FACE('',(#3259),#1592,.F.);
#24013=ADVANCED_FACE('',(#3260),#1593,.T.);
#24014=ADVANCED_FACE('',(#3261),#1594,.F.);
#24015=ADVANCED_FACE('',(#3262),#1595,.F.);
#24016=ADVANCED_FACE('',(#3263),#1596,.T.);
#24017=ADVANCED_FACE('',(#3264),#1597,.F.);
#24018=ADVANCED_FACE('',(#3265),#1598,.F.);
#24019=ADVANCED_FACE('',(#3266),#1599,.T.);
#24020=ADVANCED_FACE('',(#3267),#1600,.F.);
#24021=ADVANCED_FACE('',(#3268),#1601,.F.);
#24022=ADVANCED_FACE('',(#3269),#1602,.T.);
#24023=ADVANCED_FACE('',(#3270),#1603,.F.);
#24024=ADVANCED_FACE('',(#3271),#1604,.F.);
#24025=ADVANCED_FACE('',(#3272),#1605,.T.);
#24026=ADVANCED_FACE('',(#3273),#1606,.F.);
#24027=ADVANCED_FACE('',(#3274),#1607,.F.);
#24028=ADVANCED_FACE('',(#3275),#1608,.T.);
#24029=ADVANCED_FACE('',(#3276),#1609,.F.);
#24030=ADVANCED_FACE('',(#3277),#1610,.F.);
#24031=ADVANCED_FACE('',(#3278),#1611,.T.);
#24032=ADVANCED_FACE('',(#3279),#1612,.F.);
#24033=ADVANCED_FACE('',(#3280),#1613,.F.);
#24034=ADVANCED_FACE('',(#3281),#1614,.T.);
#24035=ADVANCED_FACE('',(#3282),#1615,.F.);
#24036=ADVANCED_FACE('',(#3283),#1616,.F.);
#24037=ADVANCED_FACE('',(#3284),#1617,.T.);
#24038=ADVANCED_FACE('',(#3285),#1618,.F.);
#24039=ADVANCED_FACE('',(#3286),#1619,.F.);
#24040=ADVANCED_FACE('',(#3287),#1620,.T.);
#24041=ADVANCED_FACE('',(#3288),#1621,.F.);
#24042=ADVANCED_FACE('',(#3289),#1622,.F.);
#24043=ADVANCED_FACE('',(#3290),#1623,.T.);
#24044=ADVANCED_FACE('',(#3291),#1624,.F.);
#24045=ADVANCED_FACE('',(#3292),#1625,.F.);
#24046=ADVANCED_FACE('',(#3293),#1626,.T.);
#24047=ADVANCED_FACE('',(#3294),#1627,.F.);
#24048=ADVANCED_FACE('',(#3295),#1628,.F.);
#24049=ADVANCED_FACE('',(#3296),#1629,.T.);
#24050=ADVANCED_FACE('',(#3297),#1630,.F.);
#24051=ADVANCED_FACE('',(#3298),#1631,.F.);
#24052=ADVANCED_FACE('',(#3299),#1632,.T.);
#24053=ADVANCED_FACE('',(#3300),#1633,.F.);
#24054=ADVANCED_FACE('',(#3301),#1634,.F.);
#24055=ADVANCED_FACE('',(#3302),#1635,.T.);
#24056=ADVANCED_FACE('',(#3303),#1636,.F.);
#24057=ADVANCED_FACE('',(#3304),#1637,.F.);
#24058=ADVANCED_FACE('',(#3305),#1638,.T.);
#24059=ADVANCED_FACE('',(#3306),#1639,.F.);
#24060=ADVANCED_FACE('',(#3307),#1640,.F.);
#24061=ADVANCED_FACE('',(#3308),#1641,.T.);
#24062=ADVANCED_FACE('',(#3309),#1642,.F.);
#24063=ADVANCED_FACE('',(#3310),#1643,.F.);
#24064=ADVANCED_FACE('',(#3311),#1644,.T.);
#24065=ADVANCED_FACE('',(#3312),#1645,.F.);
#24066=ADVANCED_FACE('',(#3313),#1646,.F.);
#24067=ADVANCED_FACE('',(#3314),#1647,.T.);
#24068=ADVANCED_FACE('',(#3315),#1648,.F.);
#24069=ADVANCED_FACE('',(#3316),#1649,.F.);
#24070=ADVANCED_FACE('',(#3317),#1650,.T.);
#24071=ADVANCED_FACE('',(#3318),#1651,.F.);
#24072=ADVANCED_FACE('',(#3319),#1652,.F.);
#24073=ADVANCED_FACE('',(#3320),#1653,.T.);
#24074=ADVANCED_FACE('',(#3321),#1654,.F.);
#24075=ADVANCED_FACE('',(#3322),#1655,.F.);
#24076=ADVANCED_FACE('',(#3323),#1656,.T.);
#24077=ADVANCED_FACE('',(#3324),#1657,.F.);
#24078=ADVANCED_FACE('',(#3325),#1658,.F.);
#24079=ADVANCED_FACE('',(#3326),#1659,.T.);
#24080=ADVANCED_FACE('',(#3327),#1660,.F.);
#24081=ADVANCED_FACE('',(#3328),#1661,.F.);
#24082=ADVANCED_FACE('',(#3329),#1662,.T.);
#24083=ADVANCED_FACE('',(#3330),#1663,.F.);
#24084=ADVANCED_FACE('',(#3331),#1664,.F.);
#24085=ADVANCED_FACE('',(#3332),#2279,.T.);
#24086=ADVANCED_FACE('',(#3333),#1665,.F.);
#24087=ADVANCED_FACE('',(#3334),#1666,.F.);
#24088=ADVANCED_FACE('',(#3335),#1667,.T.);
#24089=ADVANCED_FACE('',(#3336),#23149,.T.);
#24090=ADVANCED_FACE('',(#3337),#23150,.F.);
#24091=ADVANCED_FACE('',(#3338),#1668,.F.);
#24092=ADVANCED_FACE('',(#3339),#1669,.F.);
#24093=ADVANCED_FACE('',(#3340),#1670,.F.);
#24094=ADVANCED_FACE('',(#3341),#1671,.F.);
#24095=ADVANCED_FACE('',(#3342),#1672,.F.);
#24096=ADVANCED_FACE('',(#3343),#1673,.F.);
#24097=ADVANCED_FACE('',(#3344,#1263),#1674,.F.);
#24098=ADVANCED_FACE('',(#3345),#1675,.T.);
#24099=ADVANCED_FACE('',(#3346),#23151,.T.);
#24100=ADVANCED_FACE('',(#3347),#2280,.T.);
#24101=ADVANCED_FACE('',(#3348),#23152,.T.);
#24102=ADVANCED_FACE('',(#3349,#1264),#1676,.T.);
#24103=ADVANCED_FACE('',(#3350,#1265),#1677,.T.);
#24104=ADVANCED_FACE('',(#3351),#2281,.T.);
#24105=ADVANCED_FACE('',(#3352),#2282,.T.);
#24106=ADVANCED_FACE('',(#3353),#2283,.T.);
#24107=ADVANCED_FACE('',(#3354),#2284,.T.);
#24108=ADVANCED_FACE('',(#3355),#2285,.T.);
#24109=ADVANCED_FACE('',(#3356),#2286,.T.);
#24110=ADVANCED_FACE('',(#3357),#2287,.T.);
#24111=ADVANCED_FACE('',(#3358),#2288,.T.);
#24112=ADVANCED_FACE('',(#3359),#2289,.T.);
#24113=ADVANCED_FACE('',(#3360),#2290,.T.);
#24114=ADVANCED_FACE('',(#3361),#2291,.T.);
#24115=ADVANCED_FACE('',(#3362),#2292,.T.);
#24116=ADVANCED_FACE('',(#3363),#2293,.T.);
#24117=ADVANCED_FACE('',(#3364),#2294,.T.);
#24118=ADVANCED_FACE('',(#3365),#2295,.T.);
#24119=ADVANCED_FACE('',(#3366),#2296,.T.);
#24120=ADVANCED_FACE('',(#3367),#2297,.T.);
#24121=ADVANCED_FACE('',(#3368),#2298,.T.);
#24122=ADVANCED_FACE('',(#3369),#2299,.T.);
#24123=ADVANCED_FACE('',(#3370),#2300,.T.);
#24124=ADVANCED_FACE('',(#3371),#2301,.T.);
#24125=ADVANCED_FACE('',(#3372),#2302,.T.);
#24126=ADVANCED_FACE('',(#3373),#2303,.T.);
#24127=ADVANCED_FACE('',(#3374),#2304,.T.);
#24128=ADVANCED_FACE('',(#3375),#2305,.T.);
#24129=ADVANCED_FACE('',(#3376),#2306,.T.);
#24130=ADVANCED_FACE('',(#3377),#2307,.T.);
#24131=ADVANCED_FACE('',(#3378),#2308,.T.);
#24132=ADVANCED_FACE('',(#3379),#2309,.T.);
#24133=ADVANCED_FACE('',(#3380),#2310,.T.);
#24134=ADVANCED_FACE('',(#3381),#2311,.T.);
#24135=ADVANCED_FACE('',(#3382),#2312,.T.);
#24136=ADVANCED_FACE('',(#3383),#2313,.T.);
#24137=ADVANCED_FACE('',(#3384),#2314,.T.);
#24138=ADVANCED_FACE('',(#3385),#2315,.T.);
#24139=ADVANCED_FACE('',(#3386),#2316,.T.);
#24140=ADVANCED_FACE('',(#3387),#2317,.T.);
#24141=ADVANCED_FACE('',(#3388),#2318,.T.);
#24142=ADVANCED_FACE('',(#3389),#2319,.T.);
#24143=ADVANCED_FACE('',(#3390),#2320,.T.);
#24144=ADVANCED_FACE('',(#3391),#2321,.T.);
#24145=ADVANCED_FACE('',(#3392),#2322,.T.);
#24146=ADVANCED_FACE('',(#3393),#2323,.T.);
#24147=ADVANCED_FACE('',(#3394),#2324,.T.);
#24148=ADVANCED_FACE('',(#3395),#2325,.T.);
#24149=ADVANCED_FACE('',(#3396),#2326,.T.);
#24150=ADVANCED_FACE('',(#3397),#2327,.T.);
#24151=ADVANCED_FACE('',(#3398),#1678,.F.);
#24152=ADVANCED_FACE('',(#3399),#476,.F.);
#24153=ADVANCED_FACE('',(#3400),#1679,.T.);
#24154=ADVANCED_FACE('',(#3401),#2328,.T.);
#24155=ADVANCED_FACE('',(#3402),#477,.F.);
#24156=ADVANCED_FACE('',(#3403),#1680,.T.);
#24157=ADVANCED_FACE('',(#3404),#1681,.F.);
#24158=ADVANCED_FACE('',(#3405),#1682,.F.);
#24159=ADVANCED_FACE('',(#3406),#1683,.T.);
#24160=ADVANCED_FACE('',(#3407),#1684,.F.);
#24161=ADVANCED_FACE('',(#3408),#1685,.F.);
#24162=ADVANCED_FACE('',(#3409),#1686,.T.);
#24163=ADVANCED_FACE('',(#3410),#1687,.F.);
#24164=ADVANCED_FACE('',(#3411),#1688,.F.);
#24165=ADVANCED_FACE('',(#3412),#1689,.T.);
#24166=ADVANCED_FACE('',(#3413),#1690,.F.);
#24167=ADVANCED_FACE('',(#3414),#1691,.F.);
#24168=ADVANCED_FACE('',(#3415),#1692,.T.);
#24169=ADVANCED_FACE('',(#3416),#1693,.F.);
#24170=ADVANCED_FACE('',(#3417),#1694,.F.);
#24171=ADVANCED_FACE('',(#3418),#1695,.T.);
#24172=ADVANCED_FACE('',(#3419),#1696,.F.);
#24173=ADVANCED_FACE('',(#3420),#1697,.F.);
#24174=ADVANCED_FACE('',(#3421),#1698,.T.);
#24175=ADVANCED_FACE('',(#3422),#1699,.F.);
#24176=ADVANCED_FACE('',(#3423),#1700,.F.);
#24177=ADVANCED_FACE('',(#3424),#1701,.T.);
#24178=ADVANCED_FACE('',(#3425),#1702,.F.);
#24179=ADVANCED_FACE('',(#3426),#1703,.F.);
#24180=ADVANCED_FACE('',(#3427),#1704,.T.);
#24181=ADVANCED_FACE('',(#3428),#1705,.F.);
#24182=ADVANCED_FACE('',(#3429),#1706,.F.);
#24183=ADVANCED_FACE('',(#3430),#1707,.T.);
#24184=ADVANCED_FACE('',(#3431),#1708,.F.);
#24185=ADVANCED_FACE('',(#3432),#1709,.F.);
#24186=ADVANCED_FACE('',(#3433),#1710,.T.);
#24187=ADVANCED_FACE('',(#3434),#1711,.F.);
#24188=ADVANCED_FACE('',(#3435),#1712,.F.);
#24189=ADVANCED_FACE('',(#3436),#1713,.T.);
#24190=ADVANCED_FACE('',(#3437),#1714,.F.);
#24191=ADVANCED_FACE('',(#3438),#1715,.F.);
#24192=ADVANCED_FACE('',(#3439),#1716,.T.);
#24193=ADVANCED_FACE('',(#3440),#1717,.F.);
#24194=ADVANCED_FACE('',(#3441),#1718,.F.);
#24195=ADVANCED_FACE('',(#3442),#1719,.T.);
#24196=ADVANCED_FACE('',(#3443),#1720,.F.);
#24197=ADVANCED_FACE('',(#3444),#1721,.F.);
#24198=ADVANCED_FACE('',(#3445),#1722,.T.);
#24199=ADVANCED_FACE('',(#3446),#1723,.F.);
#24200=ADVANCED_FACE('',(#3447),#1724,.F.);
#24201=ADVANCED_FACE('',(#3448),#1725,.T.);
#24202=ADVANCED_FACE('',(#3449),#1726,.F.);
#24203=ADVANCED_FACE('',(#3450),#1727,.F.);
#24204=ADVANCED_FACE('',(#3451),#1728,.T.);
#24205=ADVANCED_FACE('',(#3452),#1729,.F.);
#24206=ADVANCED_FACE('',(#3453),#1730,.F.);
#24207=ADVANCED_FACE('',(#3454),#1731,.T.);
#24208=ADVANCED_FACE('',(#3455),#1732,.F.);
#24209=ADVANCED_FACE('',(#3456),#1733,.F.);
#24210=ADVANCED_FACE('',(#3457),#1734,.T.);
#24211=ADVANCED_FACE('',(#3458),#1735,.F.);
#24212=ADVANCED_FACE('',(#3459),#1736,.F.);
#24213=ADVANCED_FACE('',(#3460),#1737,.T.);
#24214=ADVANCED_FACE('',(#3461),#1738,.F.);
#24215=ADVANCED_FACE('',(#3462),#1739,.F.);
#24216=ADVANCED_FACE('',(#3463),#1740,.T.);
#24217=ADVANCED_FACE('',(#3464),#1741,.F.);
#24218=ADVANCED_FACE('',(#3465),#1742,.F.);
#24219=ADVANCED_FACE('',(#3466),#1743,.T.);
#24220=ADVANCED_FACE('',(#3467),#1744,.F.);
#24221=ADVANCED_FACE('',(#3468),#1745,.F.);
#24222=ADVANCED_FACE('',(#3469),#1746,.T.);
#24223=ADVANCED_FACE('',(#3470),#1747,.F.);
#24224=ADVANCED_FACE('',(#3471),#1748,.F.);
#24225=ADVANCED_FACE('',(#3472),#1749,.T.);
#24226=ADVANCED_FACE('',(#3473),#1750,.F.);
#24227=ADVANCED_FACE('',(#3474),#1751,.F.);
#24228=ADVANCED_FACE('',(#3475),#1752,.T.);
#24229=ADVANCED_FACE('',(#3476),#1753,.F.);
#24230=ADVANCED_FACE('',(#3477),#1754,.F.);
#24231=ADVANCED_FACE('',(#3478),#1755,.T.);
#24232=ADVANCED_FACE('',(#3479),#1756,.F.);
#24233=ADVANCED_FACE('',(#3480),#1757,.F.);
#24234=ADVANCED_FACE('',(#3481),#1758,.T.);
#24235=ADVANCED_FACE('',(#3482),#1759,.F.);
#24236=ADVANCED_FACE('',(#3483),#1760,.F.);
#24237=ADVANCED_FACE('',(#3484),#1761,.T.);
#24238=ADVANCED_FACE('',(#3485),#1762,.F.);
#24239=ADVANCED_FACE('',(#3486),#1763,.F.);
#24240=ADVANCED_FACE('',(#3487),#1764,.T.);
#24241=ADVANCED_FACE('',(#3488),#1765,.F.);
#24242=ADVANCED_FACE('',(#3489),#1766,.F.);
#24243=ADVANCED_FACE('',(#3490),#1767,.T.);
#24244=ADVANCED_FACE('',(#3491),#1768,.F.);
#24245=ADVANCED_FACE('',(#3492),#1769,.F.);
#24246=ADVANCED_FACE('',(#3493),#1770,.T.);
#24247=ADVANCED_FACE('',(#3494),#1771,.F.);
#24248=ADVANCED_FACE('',(#3495),#1772,.F.);
#24249=ADVANCED_FACE('',(#3496),#1773,.T.);
#24250=ADVANCED_FACE('',(#3497),#1774,.F.);
#24251=ADVANCED_FACE('',(#3498),#1775,.F.);
#24252=ADVANCED_FACE('',(#3499),#1776,.T.);
#24253=ADVANCED_FACE('',(#3500),#1777,.F.);
#24254=ADVANCED_FACE('',(#3501),#1778,.F.);
#24255=ADVANCED_FACE('',(#3502),#1779,.T.);
#24256=ADVANCED_FACE('',(#3503),#1780,.F.);
#24257=ADVANCED_FACE('',(#3504),#1781,.F.);
#24258=ADVANCED_FACE('',(#3505),#1782,.T.);
#24259=ADVANCED_FACE('',(#3506),#1783,.F.);
#24260=ADVANCED_FACE('',(#3507),#1784,.F.);
#24261=ADVANCED_FACE('',(#3508),#2329,.T.);
#24262=ADVANCED_FACE('',(#3509),#1785,.F.);
#24263=ADVANCED_FACE('',(#3510),#1786,.F.);
#24264=ADVANCED_FACE('',(#3511),#1787,.T.);
#24265=ADVANCED_FACE('',(#3512),#23153,.T.);
#24266=ADVANCED_FACE('',(#3513),#23154,.F.);
#24267=ADVANCED_FACE('',(#3514),#1788,.F.);
#24268=ADVANCED_FACE('',(#3515),#1789,.F.);
#24269=ADVANCED_FACE('',(#3516),#1790,.F.);
#24270=ADVANCED_FACE('',(#3517),#1791,.F.);
#24271=ADVANCED_FACE('',(#3518),#1792,.F.);
#24272=ADVANCED_FACE('',(#3519),#1793,.F.);
#24273=ADVANCED_FACE('',(#3520,#1266),#1794,.F.);
#24274=ADVANCED_FACE('',(#3521),#1795,.T.);
#24275=ADVANCED_FACE('',(#3522),#23155,.T.);
#24276=ADVANCED_FACE('',(#3523),#2330,.T.);
#24277=ADVANCED_FACE('',(#3524),#23156,.T.);
#24278=ADVANCED_FACE('',(#3525,#1267),#1796,.T.);
#24279=ADVANCED_FACE('',(#3526,#1268),#1797,.T.);
#24280=ADVANCED_FACE('',(#3527),#2331,.T.);
#24281=ADVANCED_FACE('',(#3528),#2332,.T.);
#24282=ADVANCED_FACE('',(#3529),#2333,.T.);
#24283=ADVANCED_FACE('',(#3530),#2334,.T.);
#24284=ADVANCED_FACE('',(#3531),#2335,.T.);
#24285=ADVANCED_FACE('',(#3532),#2336,.T.);
#24286=ADVANCED_FACE('',(#3533),#2337,.T.);
#24287=ADVANCED_FACE('',(#3534),#2338,.T.);
#24288=ADVANCED_FACE('',(#3535),#2339,.T.);
#24289=ADVANCED_FACE('',(#3536),#2340,.T.);
#24290=ADVANCED_FACE('',(#3537),#2341,.T.);
#24291=ADVANCED_FACE('',(#3538),#2342,.T.);
#24292=ADVANCED_FACE('',(#3539),#2343,.T.);
#24293=ADVANCED_FACE('',(#3540),#2344,.T.);
#24294=ADVANCED_FACE('',(#3541),#2345,.T.);
#24295=ADVANCED_FACE('',(#3542),#2346,.T.);
#24296=ADVANCED_FACE('',(#3543),#2347,.T.);
#24297=ADVANCED_FACE('',(#3544),#2348,.T.);
#24298=ADVANCED_FACE('',(#3545),#2349,.T.);
#24299=ADVANCED_FACE('',(#3546),#2350,.T.);
#24300=ADVANCED_FACE('',(#3547),#2351,.T.);
#24301=ADVANCED_FACE('',(#3548),#2352,.T.);
#24302=ADVANCED_FACE('',(#3549),#2353,.T.);
#24303=ADVANCED_FACE('',(#3550),#2354,.T.);
#24304=ADVANCED_FACE('',(#3551),#1798,.F.);
#24305=ADVANCED_FACE('',(#3552),#478,.F.);
#24306=ADVANCED_FACE('',(#3553),#1799,.T.);
#24307=ADVANCED_FACE('',(#3554),#2355,.T.);
#24308=ADVANCED_FACE('',(#3555),#479,.F.);
#24309=ADVANCED_FACE('',(#3556),#2356,.T.);
#24310=ADVANCED_FACE('',(#3557),#1800,.T.);
#24311=ADVANCED_FACE('',(#3558),#1801,.F.);
#24312=ADVANCED_FACE('',(#3559),#1802,.F.);
#24313=ADVANCED_FACE('',(#3560),#1803,.T.);
#24314=ADVANCED_FACE('',(#3561),#1804,.F.);
#24315=ADVANCED_FACE('',(#3562),#1805,.F.);
#24316=ADVANCED_FACE('',(#3563),#1806,.T.);
#24317=ADVANCED_FACE('',(#3564),#1807,.F.);
#24318=ADVANCED_FACE('',(#3565),#1808,.F.);
#24319=ADVANCED_FACE('',(#3566),#1809,.T.);
#24320=ADVANCED_FACE('',(#3567),#1810,.F.);
#24321=ADVANCED_FACE('',(#3568),#1811,.F.);
#24322=ADVANCED_FACE('',(#3569),#1812,.T.);
#24323=ADVANCED_FACE('',(#3570),#1813,.F.);
#24324=ADVANCED_FACE('',(#3571),#1814,.F.);
#24325=ADVANCED_FACE('',(#3572),#1815,.T.);
#24326=ADVANCED_FACE('',(#3573),#1816,.F.);
#24327=ADVANCED_FACE('',(#3574),#1817,.F.);
#24328=ADVANCED_FACE('',(#3575),#1818,.T.);
#24329=ADVANCED_FACE('',(#3576),#1819,.F.);
#24330=ADVANCED_FACE('',(#3577),#1820,.F.);
#24331=ADVANCED_FACE('',(#3578),#1821,.T.);
#24332=ADVANCED_FACE('',(#3579),#1822,.F.);
#24333=ADVANCED_FACE('',(#3580),#1823,.F.);
#24334=ADVANCED_FACE('',(#3581),#1824,.T.);
#24335=ADVANCED_FACE('',(#3582),#1825,.F.);
#24336=ADVANCED_FACE('',(#3583),#1826,.F.);
#24337=ADVANCED_FACE('',(#3584),#1827,.T.);
#24338=ADVANCED_FACE('',(#3585),#1828,.F.);
#24339=ADVANCED_FACE('',(#3586),#1829,.F.);
#24340=ADVANCED_FACE('',(#3587),#1830,.T.);
#24341=ADVANCED_FACE('',(#3588),#1831,.F.);
#24342=ADVANCED_FACE('',(#3589),#1832,.F.);
#24343=ADVANCED_FACE('',(#3590),#1833,.T.);
#24344=ADVANCED_FACE('',(#3591),#1834,.F.);
#24345=ADVANCED_FACE('',(#3592),#1835,.F.);
#24346=ADVANCED_FACE('',(#3593),#1836,.T.);
#24347=ADVANCED_FACE('',(#3594),#1837,.F.);
#24348=ADVANCED_FACE('',(#3595),#1838,.F.);
#24349=ADVANCED_FACE('',(#3596),#1839,.T.);
#24350=ADVANCED_FACE('',(#3597),#1840,.F.);
#24351=ADVANCED_FACE('',(#3598),#1841,.F.);
#24352=ADVANCED_FACE('',(#3599),#1842,.T.);
#24353=ADVANCED_FACE('',(#3600),#1843,.F.);
#24354=ADVANCED_FACE('',(#3601),#1844,.F.);
#24355=ADVANCED_FACE('',(#3602),#1845,.T.);
#24356=ADVANCED_FACE('',(#3603),#1846,.F.);
#24357=ADVANCED_FACE('',(#3604),#1847,.F.);
#24358=ADVANCED_FACE('',(#3605),#1848,.T.);
#24359=ADVANCED_FACE('',(#3606),#1849,.F.);
#24360=ADVANCED_FACE('',(#3607),#1850,.F.);
#24361=ADVANCED_FACE('',(#3608),#1851,.T.);
#24362=ADVANCED_FACE('',(#3609),#1852,.F.);
#24363=ADVANCED_FACE('',(#3610),#1853,.F.);
#24364=ADVANCED_FACE('',(#3611),#1854,.T.);
#24365=ADVANCED_FACE('',(#3612),#1855,.F.);
#24366=ADVANCED_FACE('',(#3613),#1856,.F.);
#24367=ADVANCED_FACE('',(#3614),#1857,.T.);
#24368=ADVANCED_FACE('',(#3615),#1858,.F.);
#24369=ADVANCED_FACE('',(#3616),#1859,.F.);
#24370=ADVANCED_FACE('',(#3617),#1860,.T.);
#24371=ADVANCED_FACE('',(#3618),#1861,.F.);
#24372=ADVANCED_FACE('',(#3619),#1862,.F.);
#24373=ADVANCED_FACE('',(#3620),#1863,.T.);
#24374=ADVANCED_FACE('',(#3621),#1864,.F.);
#24375=ADVANCED_FACE('',(#3622),#1865,.F.);
#24376=ADVANCED_FACE('',(#3623),#1866,.T.);
#24377=ADVANCED_FACE('',(#3624),#1867,.F.);
#24378=ADVANCED_FACE('',(#3625),#1868,.F.);
#24379=ADVANCED_FACE('',(#3626),#1869,.T.);
#24380=ADVANCED_FACE('',(#3627),#1870,.F.);
#24381=ADVANCED_FACE('',(#3628),#1871,.F.);
#24382=ADVANCED_FACE('',(#3629),#1872,.T.);
#24383=ADVANCED_FACE('',(#3630),#1873,.F.);
#24384=ADVANCED_FACE('',(#3631),#1874,.F.);
#24385=ADVANCED_FACE('',(#3632),#1875,.T.);
#24386=ADVANCED_FACE('',(#3633),#1876,.F.);
#24387=ADVANCED_FACE('',(#3634),#1877,.F.);
#24388=ADVANCED_FACE('',(#3635),#1878,.T.);
#24389=ADVANCED_FACE('',(#3636),#1879,.F.);
#24390=ADVANCED_FACE('',(#3637),#1880,.F.);
#24391=ADVANCED_FACE('',(#3638),#1881,.T.);
#24392=ADVANCED_FACE('',(#3639),#1882,.F.);
#24393=ADVANCED_FACE('',(#3640),#1883,.F.);
#24394=ADVANCED_FACE('',(#3641),#1884,.T.);
#24395=ADVANCED_FACE('',(#3642),#1885,.F.);
#24396=ADVANCED_FACE('',(#3643),#1886,.F.);
#24397=ADVANCED_FACE('',(#3644),#1887,.T.);
#24398=ADVANCED_FACE('',(#3645),#1888,.F.);
#24399=ADVANCED_FACE('',(#3646),#1889,.F.);
#24400=ADVANCED_FACE('',(#3647),#1890,.T.);
#24401=ADVANCED_FACE('',(#3648),#1891,.F.);
#24402=ADVANCED_FACE('',(#3649),#1892,.F.);
#24403=ADVANCED_FACE('',(#3650),#1893,.T.);
#24404=ADVANCED_FACE('',(#3651),#1894,.F.);
#24405=ADVANCED_FACE('',(#3652),#1895,.F.);
#24406=ADVANCED_FACE('',(#3653),#1896,.T.);
#24407=ADVANCED_FACE('',(#3654),#1897,.F.);
#24408=ADVANCED_FACE('',(#3655),#1898,.F.);
#24409=ADVANCED_FACE('',(#3656),#1899,.T.);
#24410=ADVANCED_FACE('',(#3657),#1900,.F.);
#24411=ADVANCED_FACE('',(#3658),#1901,.F.);
#24412=ADVANCED_FACE('',(#3659),#1902,.T.);
#24413=ADVANCED_FACE('',(#3660),#1903,.F.);
#24414=ADVANCED_FACE('',(#3661),#1904,.F.);
#24415=ADVANCED_FACE('',(#3662),#2357,.T.);
#24416=ADVANCED_FACE('',(#3663),#1905,.F.);
#24417=ADVANCED_FACE('',(#3664),#1906,.F.);
#24418=ADVANCED_FACE('',(#3665),#1907,.T.);
#24419=ADVANCED_FACE('',(#3666),#23157,.T.);
#24420=ADVANCED_FACE('',(#3667),#23158,.F.);
#24421=ADVANCED_FACE('',(#3668),#1908,.F.);
#24422=ADVANCED_FACE('',(#3669),#1909,.F.);
#24423=ADVANCED_FACE('',(#3670),#1910,.F.);
#24424=ADVANCED_FACE('',(#3671),#1911,.F.);
#24425=ADVANCED_FACE('',(#3672),#1912,.F.);
#24426=ADVANCED_FACE('',(#3673),#1913,.F.);
#24427=ADVANCED_FACE('',(#3674,#1269),#1914,.F.);
#24428=ADVANCED_FACE('',(#3675),#1915,.T.);
#24429=ADVANCED_FACE('',(#3676),#23159,.T.);
#24430=ADVANCED_FACE('',(#3677),#23160,.T.);
#24431=ADVANCED_FACE('',(#3678,#1270),#1916,.T.);
#24432=ADVANCED_FACE('',(#3679,#1271),#1917,.T.);
#24433=ADVANCED_FACE('',(#3680),#2358,.T.);
#24434=ADVANCED_FACE('',(#3681),#2359,.T.);
#24435=ADVANCED_FACE('',(#3682),#2360,.T.);
#24436=ADVANCED_FACE('',(#3683),#2361,.T.);
#24437=ADVANCED_FACE('',(#3684),#2362,.T.);
#24438=ADVANCED_FACE('',(#3685),#2363,.T.);
#24439=ADVANCED_FACE('',(#3686),#2364,.T.);
#24440=ADVANCED_FACE('',(#3687),#2365,.T.);
#24441=ADVANCED_FACE('',(#3688),#2366,.T.);
#24442=ADVANCED_FACE('',(#3689),#2367,.T.);
#24443=ADVANCED_FACE('',(#3690),#2368,.T.);
#24444=ADVANCED_FACE('',(#3691),#2369,.T.);
#24445=ADVANCED_FACE('',(#3692),#2370,.T.);
#24446=ADVANCED_FACE('',(#3693),#2371,.T.);
#24447=ADVANCED_FACE('',(#3694),#2372,.T.);
#24448=ADVANCED_FACE('',(#3695),#480,.F.);
#24449=ADVANCED_FACE('',(#3696),#1918,.T.);
#24450=ADVANCED_FACE('',(#3697),#2373,.T.);
#24451=ADVANCED_FACE('',(#3698),#481,.F.);
#24452=ADVANCED_FACE('',(#3699),#1919,.F.);
#24453=ADVANCED_FACE('',(#3700),#1920,.F.);
#24454=ADVANCED_FACE('',(#3701),#1921,.F.);
#24455=ADVANCED_FACE('',(#3702),#1922,.F.);
#24456=ADVANCED_FACE('',(#3703),#1923,.F.);
#24457=ADVANCED_FACE('',(#3704),#1924,.F.);
#24458=ADVANCED_FACE('',(#3705,#1272),#1925,.T.);
#24459=ADVANCED_FACE('',(#3706),#1926,.F.);
#24460=ADVANCED_FACE('',(#3707),#1927,.F.);
#24461=ADVANCED_FACE('',(#3708),#1928,.F.);
#24462=ADVANCED_FACE('',(#3709),#1929,.F.);
#24463=ADVANCED_FACE('',(#3710),#1930,.F.);
#24464=ADVANCED_FACE('',(#3711),#1931,.F.);
#24465=ADVANCED_FACE('',(#3712),#1932,.T.);
#24466=ADVANCED_FACE('',(#3713),#1933,.T.);
#24467=ADVANCED_FACE('',(#3714),#23161,.T.);
#24468=ADVANCED_FACE('',(#3715),#2374,.T.);
#24469=ADVANCED_FACE('',(#3716,#1273),#1934,.T.);
#24470=ADVANCED_FACE('',(#3717),#2375,.T.);
#24471=ADVANCED_FACE('',(#3718),#23162,.T.);
#24472=ADVANCED_FACE('',(#3719),#2376,.T.);
#24473=ADVANCED_FACE('',(#3720),#2377,.T.);
#24474=ADVANCED_FACE('',(#3721),#2378,.T.);
#24475=ADVANCED_FACE('',(#3722),#2379,.T.);
#24476=ADVANCED_FACE('',(#3723),#2380,.T.);
#24477=ADVANCED_FACE('',(#3724),#2381,.T.);
#24478=ADVANCED_FACE('',(#3725),#2382,.T.);
#24479=ADVANCED_FACE('',(#3726),#2383,.T.);
#24480=ADVANCED_FACE('',(#3727),#2384,.T.);
#24481=ADVANCED_FACE('',(#3728),#2385,.T.);
#24482=ADVANCED_FACE('',(#3729),#2386,.T.);
#24483=ADVANCED_FACE('',(#3730),#2387,.T.);
#24484=ADVANCED_FACE('',(#3731),#2388,.T.);
#24485=ADVANCED_FACE('',(#3732),#2389,.T.);
#24486=ADVANCED_FACE('',(#3733),#2390,.T.);
#24487=ADVANCED_FACE('',(#3734),#2391,.T.);
#24488=ADVANCED_FACE('',(#3735),#2392,.T.);
#24489=ADVANCED_FACE('',(#3736),#2393,.T.);
#24490=ADVANCED_FACE('',(#3737),#2394,.T.);
#24491=ADVANCED_FACE('',(#3738),#2395,.T.);
#24492=ADVANCED_FACE('',(#3739),#2396,.T.);
#24493=ADVANCED_FACE('',(#3740),#2397,.T.);
#24494=ADVANCED_FACE('',(#3741),#2398,.T.);
#24495=ADVANCED_FACE('',(#3742),#2399,.T.);
#24496=ADVANCED_FACE('',(#3743),#2400,.T.);
#24497=ADVANCED_FACE('',(#3744),#2401,.T.);
#24498=ADVANCED_FACE('',(#3745),#2402,.T.);
#24499=ADVANCED_FACE('',(#3746),#2403,.T.);
#24500=ADVANCED_FACE('',(#3747),#2404,.T.);
#24501=ADVANCED_FACE('',(#3748),#2405,.T.);
#24502=ADVANCED_FACE('',(#3749),#2406,.T.);
#24503=ADVANCED_FACE('',(#3750),#2407,.T.);
#24504=ADVANCED_FACE('',(#3751),#2408,.T.);
#24505=ADVANCED_FACE('',(#3752),#482,.F.);
#24506=ADVANCED_FACE('',(#3753),#1935,.T.);
#24507=ADVANCED_FACE('',(#3754),#2409,.T.);
#24508=ADVANCED_FACE('',(#3755),#483,.F.);
#24509=ADVANCED_FACE('',(#3756),#2410,.T.);
#24510=ADVANCED_FACE('',(#3757),#1936,.F.);
#24511=ADVANCED_FACE('',(#3758),#1937,.F.);
#24512=ADVANCED_FACE('',(#3759),#1938,.F.);
#24513=ADVANCED_FACE('',(#3760),#1939,.F.);
#24514=ADVANCED_FACE('',(#3761),#1940,.F.);
#24515=ADVANCED_FACE('',(#3762),#1941,.F.);
#24516=ADVANCED_FACE('',(#3763,#1274),#1942,.T.);
#24517=ADVANCED_FACE('',(#3764),#1943,.F.);
#24518=ADVANCED_FACE('',(#3765),#1944,.F.);
#24519=ADVANCED_FACE('',(#3766),#1945,.F.);
#24520=ADVANCED_FACE('',(#3767),#1946,.F.);
#24521=ADVANCED_FACE('',(#3768),#1947,.F.);
#24522=ADVANCED_FACE('',(#3769),#1948,.F.);
#24523=ADVANCED_FACE('',(#3770),#1949,.T.);
#24524=ADVANCED_FACE('',(#3771),#1950,.T.);
#24525=ADVANCED_FACE('',(#3772),#23163,.T.);
#24526=ADVANCED_FACE('',(#3773,#1275),#1951,.T.);
#24527=ADVANCED_FACE('',(#3774),#2411,.T.);
#24528=ADVANCED_FACE('',(#3775),#23164,.T.);
#24529=CLOSED_SHELL('',(#23165,#23166,#23167,#23168,#23169,#23170,#23171,
#23172,#23173,#23174,#23175,#23176,#23177,#23178,#23179,#23180,#23181,#23182,
#23183,#23184,#23185,#23186,#23187,#23188,#23189,#23190,#23191,#23192,#23193,
#23194,#23195,#23196,#23197,#23198,#23199,#23200,#23201,#23202,#23203,#23204,
#23205,#23206,#23207,#23208,#23209,#23210,#23211,#23212,#23213,#23214,#23215,
#23216,#23217,#23218,#23219,#23220,#23221,#23222,#23223,#23224,#23225,#23226,
#23227,#23228,#23229,#23230,#23231,#23232,#23233,#23234));
#24530=CLOSED_SHELL('',(#23235,#23236,#23237,#23238,#23239,#23240,#23241,
#23242,#23243,#23244,#23245,#23246,#23247,#23248,#23249,#23250,#23251,#23252,
#23253,#23254,#23255,#23256,#23257,#23258,#23259,#23260,#23261,#23262,#23263,
#23264,#23265,#23266,#23267,#23268,#23269,#23270,#23271,#23272,#23273,#23274,
#23275,#23276,#23277,#23278,#23279,#23280,#23281,#23282,#23283,#23284,#23285,
#23286,#23287,#23288,#23289,#23290,#23291,#23292,#23293,#23294,#23295,#23296));
#24531=CLOSED_SHELL('',(#23297,#23298,#23299,#23300,#23301,#23302,#23303,
#23304,#23305,#23306,#23307,#23308,#23309,#23310,#23311,#23312,#23313,#23314,
#23315,#23316,#23317,#23318,#23319,#23320,#23321,#23322,#23323,#23324,#23325,
#23326,#23327,#23328,#23329,#23330,#23331,#23332,#23333,#23334,#23335,#23336,
#23337,#23338,#23339,#23340,#23341,#23342,#23343,#23344,#23345,#23346,#23347,
#23348,#23349,#23350,#23351,#23352,#23353,#23354,#23355,#23356,#23357,#23358,
#23359,#23360,#23361,#23362,#23363,#23364,#23365,#23366,#23367,#23368,#23369,
#23370,#23371,#23372,#23373,#23374,#23375,#23376,#23377,#23378,#23379,#23380,
#23381,#23382,#23383,#23384,#23385,#23386,#23387,#23388,#23389,#23390,#23391,
#23392,#23393,#23394,#23395,#23396,#23397,#23398,#23399,#23400,#23401,#23402,
#23403,#23404,#23405,#23406,#23407,#23408,#23409,#23410,#23411,#23412,#23413,
#23414,#23415,#23416,#23417,#23418,#23419,#23420,#23421,#23422,#23423,#23424,
#23425,#23426,#23427,#23428,#23429,#23430,#23431,#23432,#23433,#23434,#23435,
#23436,#23437,#23438,#23439,#23440,#23441,#23442,#23443,#23444,#23445,#23446,
#23447,#23448,#23449,#23450,#23451,#23452,#23453,#23454,#23455,#23456,#23457,
#23458,#23459,#23460,#23461,#23462,#23463,#23464,#23465,#23466,#23467,#23468,
#23469,#23470,#23471,#23472,#23473,#23474,#23475,#23476,#23477,#23478,#23479,
#23480,#23481,#23482,#23483,#23484,#23485,#23486,#23487,#23488,#23489,#23490,
#23491,#23492,#23493,#23494,#23495,#23496,#23497,#23498,#23499,#23500,#23501,
#23502,#23503,#23504,#23505,#23506,#23507,#23508,#23509,#23510,#23511,#23512,
#23513,#23514,#23515,#23516,#23517,#23518,#23519,#23520,#23521,#23522,#23523,
#23524,#23525,#23526,#23527,#23528,#23529,#23530,#23531,#23532,#23533,#23534,
#23535,#23536,#23537,#23538,#23539,#23540,#23541,#23542,#23543,#23544,#23545,
#23546,#23547,#23548,#23549,#23550,#23551,#23552,#23553,#23554,#23555,#23556,
#23557,#23558,#23559,#23560,#23561,#23562,#23563,#23564,#23565,#23566,#23567,
#23568,#23569,#23570,#23571,#23572,#23573,#23574,#23575,#23576,#23577,#23578,
#23579,#23580,#23581,#23582,#23583));
#24532=CLOSED_SHELL('',(#23584,#23585,#23586,#23587,#23588,#23589,#23590,
#23591,#23592,#23593,#23594,#23595,#23596,#23597,#23598,#23599,#23600,#23601,
#23602,#23603,#23604));
#24533=CLOSED_SHELL('',(#23605,#23606,#23607,#23608,#23609,#23610,#23611,
#23612,#23613,#23614,#23615,#23616,#23617,#23618,#23619,#23620,#23621,#23622,
#23623,#23624,#23625,#23626,#23627,#23628,#23629,#23630,#23631));
#24534=CLOSED_SHELL('',(#23632,#23633,#23634,#23635,#23636,#23637,#23638,
#23639,#23640,#23641,#23642,#23643,#23644,#23645,#23646,#23647,#23648,#23649));
#24535=CLOSED_SHELL('',(#23650,#23651,#23652,#23653,#23654,#23655,#23656,
#23657,#23658,#23659,#23660,#23661,#23662,#23663,#23664,#23665,#23666,#23667,
#23668,#23669,#23670,#23671,#23672));
#24536=CLOSED_SHELL('',(#23673,#23674,#23675,#23676,#23677,#23678,#23679,
#23680,#23681,#23682,#23683,#23684,#23685,#23686,#23687,#23688,#23689,#23690,
#23691,#23692,#23693,#23694,#23695,#23696,#23697,#23698,#23699,#23700,#23701));
#24537=CLOSED_SHELL('',(#23702,#23703,#23704,#23705,#23706,#23707,#23708,
#23709,#23710,#23711,#23712,#23713,#23714,#23715,#23716,#23717,#23718));
#24538=CLOSED_SHELL('',(#23719,#23720,#23721,#23722,#23723,#23724,#23725,
#23726,#23727,#23728,#23729,#23730,#23731,#23732,#23733,#23734,#23735,#23736,
#23737,#23738,#23739,#23740,#23741,#23742,#23743,#23744,#23745,#23746,#23747,
#23748,#23749,#23750,#23751,#23752));
#24539=CLOSED_SHELL('',(#23753,#23754,#23755,#23756,#23757,#23758,#23759,
#23760,#23761,#23762,#23763,#23764,#23765,#23766,#23767,#23768,#23769,#23770,
#23771,#23772,#23773,#23774,#23775,#23776,#23777,#23778,#23779,#23780,#23781,
#23782,#23783,#23784,#23785,#23786,#23787));
#24540=CLOSED_SHELL('',(#23788,#23789,#23790,#23791,#23792,#23793,#23794,
#23795,#23796,#23797,#23798,#23799,#23800,#23801,#23802,#23803,#23804,#23805,
#23806,#23807));
#24541=CLOSED_SHELL('',(#23808,#23809,#23810,#23811,#23812,#23813,#23814,
#23815,#23816,#23817,#23818,#23819,#23820,#23821,#23822,#23823,#23824,#23825,
#23826,#23827,#23828,#23829,#23830,#23831,#23832,#23833,#23834,#23835,#23836,
#23837,#23838,#23839,#23840,#23841,#23842,#23843,#23844,#23845,#23846));
#24542=CLOSED_SHELL('',(#23847,#23848,#23849,#23850,#23851,#23852,#23853,
#23854,#23855,#23856,#23857,#23858,#23859,#23860,#23861,#23862,#23863,#23864,
#23865,#23866,#23867,#23868,#23869,#23870,#23871));
#24543=CLOSED_SHELL('',(#23872,#23873,#23874,#23875,#23876,#23877,#23878,
#23879,#23880,#23881,#23882,#23883,#23884,#23885,#23886,#23887,#23888,#23889,
#23890,#23891,#23892,#23893,#23894,#23895,#23896,#23897,#23898,#23899,#23900,
#23901,#23902,#23903,#23904,#23905,#23906,#23907,#23908,#23909,#23910,#23911,
#23912,#23913,#23914,#23915,#23916,#23917));
#24544=CLOSED_SHELL('',(#23918,#23919,#23920,#23921,#23922,#23923,#23924,
#23925,#23926,#23927,#23928,#23929,#23930,#23931,#23932,#23933,#23934,#23935,
#23936,#23937,#23938,#23939,#23940,#23941,#23942,#23943,#23944,#23945,#23946,
#23947,#23948,#23949,#23950,#23951,#23952,#23953,#23954,#23955,#23956,#23957,
#23958,#23959,#23960,#23961,#23962,#23963,#23964,#23965,#23966,#23967,#23968,
#23969,#23970,#23971,#23972,#23973,#23974,#23975,#23976,#23977,#23978,#23979,
#23980,#23981,#23982,#23983,#23984,#23985,#23986,#23987,#23988,#23989,#23990,
#23991,#23992,#23993,#23994,#23995,#23996,#23997,#23998,#23999,#24000,#24001,
#24002,#24003,#24004,#24005,#24006,#24007,#24008,#24009,#24010,#24011,#24012,
#24013,#24014,#24015,#24016,#24017,#24018,#24019,#24020,#24021,#24022,#24023,
#24024,#24025,#24026,#24027,#24028,#24029,#24030,#24031,#24032,#24033,#24034,
#24035,#24036,#24037,#24038,#24039,#24040,#24041,#24042,#24043,#24044,#24045,
#24046,#24047,#24048,#24049,#24050,#24051,#24052,#24053,#24054,#24055,#24056,
#24057,#24058,#24059,#24060,#24061,#24062,#24063,#24064,#24065,#24066,#24067,
#24068,#24069,#24070,#24071,#24072,#24073,#24074,#24075,#24076,#24077,#24078,
#24079,#24080,#24081,#24082,#24083,#24084,#24085,#24086,#24087,#24088,#24089,
#24090,#24091,#24092,#24093,#24094,#24095,#24096,#24097,#24098,#24099,#24100,
#24101,#24102,#24103));
#24545=CLOSED_SHELL('',(#24104,#24105,#24106,#24107,#24108,#24109,#24110,
#24111,#24112,#24113,#24114,#24115,#24116,#24117,#24118,#24119,#24120,#24121,
#24122,#24123,#24124,#24125,#24126,#24127,#24128,#24129,#24130,#24131,#24132,
#24133,#24134,#24135,#24136,#24137,#24138,#24139,#24140,#24141,#24142,#24143,
#24144,#24145,#24146,#24147,#24148,#24149,#24150,#24151,#24152,#24153,#24154,
#24155,#24156,#24157,#24158,#24159,#24160,#24161,#24162,#24163,#24164,#24165,
#24166,#24167,#24168,#24169,#24170,#24171,#24172,#24173,#24174,#24175,#24176,
#24177,#24178,#24179,#24180,#24181,#24182,#24183,#24184,#24185,#24186,#24187,
#24188,#24189,#24190,#24191,#24192,#24193,#24194,#24195,#24196,#24197,#24198,
#24199,#24200,#24201,#24202,#24203,#24204,#24205,#24206,#24207,#24208,#24209,
#24210,#24211,#24212,#24213,#24214,#24215,#24216,#24217,#24218,#24219,#24220,
#24221,#24222,#24223,#24224,#24225,#24226,#24227,#24228,#24229,#24230,#24231,
#24232,#24233,#24234,#24235,#24236,#24237,#24238,#24239,#24240,#24241,#24242,
#24243,#24244,#24245,#24246,#24247,#24248,#24249,#24250,#24251,#24252,#24253,
#24254,#24255,#24256,#24257,#24258,#24259,#24260,#24261,#24262,#24263,#24264,
#24265,#24266,#24267,#24268,#24269,#24270,#24271,#24272,#24273,#24274,#24275,
#24276,#24277,#24278,#24279));
#24546=CLOSED_SHELL('',(#24280,#24281,#24282,#24283,#24284,#24285,#24286,
#24287,#24288,#24289,#24290,#24291,#24292,#24293,#24294,#24295,#24296,#24297,
#24298,#24299,#24300,#24301,#24302,#24303,#24304,#24305,#24306,#24307,#24308,
#24309,#24310,#24311,#24312,#24313,#24314,#24315,#24316,#24317,#24318,#24319,
#24320,#24321,#24322,#24323,#24324,#24325,#24326,#24327,#24328,#24329,#24330,
#24331,#24332,#24333,#24334,#24335,#24336,#24337,#24338,#24339,#24340,#24341,
#24342,#24343,#24344,#24345,#24346,#24347,#24348,#24349,#24350,#24351,#24352,
#24353,#24354,#24355,#24356,#24357,#24358,#24359,#24360,#24361,#24362,#24363,
#24364,#24365,#24366,#24367,#24368,#24369,#24370,#24371,#24372,#24373,#24374,
#24375,#24376,#24377,#24378,#24379,#24380,#24381,#24382,#24383,#24384,#24385,
#24386,#24387,#24388,#24389,#24390,#24391,#24392,#24393,#24394,#24395,#24396,
#24397,#24398,#24399,#24400,#24401,#24402,#24403,#24404,#24405,#24406,#24407,
#24408,#24409,#24410,#24411,#24412,#24413,#24414,#24415,#24416,#24417,#24418,
#24419,#24420,#24421,#24422,#24423,#24424,#24425,#24426,#24427,#24428,#24429,
#24430,#24431,#24432));
#24547=CLOSED_SHELL('',(#24433,#24434,#24435,#24436,#24437,#24438,#24439,
#24440,#24441,#24442,#24443,#24444,#24445,#24446,#24447,#24448,#24449,#24450,
#24451,#24452,#24453,#24454,#24455,#24456,#24457,#24458,#24459,#24460,#24461,
#24462,#24463,#24464,#24465,#24466,#24467,#24468,#24469,#24470,#24471));
#24548=CLOSED_SHELL('',(#24472,#24473,#24474,#24475,#24476,#24477,#24478,
#24479,#24480,#24481,#24482,#24483,#24484,#24485,#24486,#24487,#24488,#24489,
#24490,#24491,#24492,#24493,#24494,#24495,#24496,#24497,#24498,#24499,#24500,
#24501,#24502,#24503,#24504,#24505,#24506,#24507,#24508,#24509,#24510,#24511,
#24512,#24513,#24514,#24515,#24516,#24517,#24518,#24519,#24520,#24521,#24522,
#24523,#24524,#24525,#24526,#24527,#24528));
#24549=DERIVED_UNIT_ELEMENT(#24589,1.);
#24550=DERIVED_UNIT_ELEMENT(#55004,-3.);
#24551=DERIVED_UNIT_ELEMENT(#24589,1.);
#24552=DERIVED_UNIT_ELEMENT(#55004,-3.);
#24553=DERIVED_UNIT_ELEMENT(#24589,1.);
#24554=DERIVED_UNIT_ELEMENT(#55004,-3.);
#24555=DERIVED_UNIT_ELEMENT(#24589,1.);
#24556=DERIVED_UNIT_ELEMENT(#55004,-3.);
#24557=DERIVED_UNIT_ELEMENT(#24589,1.);
#24558=DERIVED_UNIT_ELEMENT(#55004,-3.);
#24559=DERIVED_UNIT_ELEMENT(#24589,1.);
#24560=DERIVED_UNIT_ELEMENT(#55004,-3.);
#24561=DERIVED_UNIT_ELEMENT(#24589,1.);
#24562=DERIVED_UNIT_ELEMENT(#55004,-3.);
#24563=DERIVED_UNIT_ELEMENT(#24589,1.);
#24564=DERIVED_UNIT_ELEMENT(#55004,-3.);
#24565=DERIVED_UNIT_ELEMENT(#24589,1.);
#24566=DERIVED_UNIT_ELEMENT(#55004,-3.);
#24567=DERIVED_UNIT_ELEMENT(#24589,1.);
#24568=DERIVED_UNIT_ELEMENT(#55004,-3.);
#24569=DERIVED_UNIT_ELEMENT(#24589,1.);
#24570=DERIVED_UNIT_ELEMENT(#55004,-3.);
#24571=DERIVED_UNIT_ELEMENT(#24589,1.);
#24572=DERIVED_UNIT_ELEMENT(#55004,-3.);
#24573=DERIVED_UNIT_ELEMENT(#24589,1.);
#24574=DERIVED_UNIT_ELEMENT(#55004,-3.);
#24575=DERIVED_UNIT_ELEMENT(#24589,1.);
#24576=DERIVED_UNIT_ELEMENT(#55004,-3.);
#24577=DERIVED_UNIT_ELEMENT(#24589,1.);
#24578=DERIVED_UNIT_ELEMENT(#55004,-3.);
#24579=DERIVED_UNIT_ELEMENT(#24589,1.);
#24580=DERIVED_UNIT_ELEMENT(#55004,-3.);
#24581=DERIVED_UNIT_ELEMENT(#24589,1.);
#24582=DERIVED_UNIT_ELEMENT(#55004,-3.);
#24583=DERIVED_UNIT_ELEMENT(#24589,1.);
#24584=DERIVED_UNIT_ELEMENT(#55004,-3.);
#24585=DERIVED_UNIT_ELEMENT(#24589,1.);
#24586=DERIVED_UNIT_ELEMENT(#55004,-3.);
#24587=DERIVED_UNIT_ELEMENT(#24589,1.);
#24588=DERIVED_UNIT_ELEMENT(#55004,-3.);
#24589=(
MASS_UNIT()
NAMED_UNIT(*)
SI_UNIT(.KILO.,.GRAM.)
);
#24590=DERIVED_UNIT((#24549,#24550));
#24591=DERIVED_UNIT((#24551,#24552));
#24592=DERIVED_UNIT((#24553,#24554));
#24593=DERIVED_UNIT((#24555,#24556));
#24594=DERIVED_UNIT((#24557,#24558));
#24595=DERIVED_UNIT((#24559,#24560));
#24596=DERIVED_UNIT((#24561,#24562));
#24597=DERIVED_UNIT((#24563,#24564));
#24598=DERIVED_UNIT((#24565,#24566));
#24599=DERIVED_UNIT((#24567,#24568));
#24600=DERIVED_UNIT((#24569,#24570));
#24601=DERIVED_UNIT((#24571,#24572));
#24602=DERIVED_UNIT((#24573,#24574));
#24603=DERIVED_UNIT((#24575,#24576));
#24604=DERIVED_UNIT((#24577,#24578));
#24605=DERIVED_UNIT((#24579,#24580));
#24606=DERIVED_UNIT((#24581,#24582));
#24607=DERIVED_UNIT((#24583,#24584));
#24608=DERIVED_UNIT((#24585,#24586));
#24609=DERIVED_UNIT((#24587,#24588));
#24610=MEASURE_REPRESENTATION_ITEM('density measure',
POSITIVE_RATIO_MEASURE(2700.),#24590);
#24611=MEASURE_REPRESENTATION_ITEM('density measure',
POSITIVE_RATIO_MEASURE(2700.),#24591);
#24612=MEASURE_REPRESENTATION_ITEM('density measure',
POSITIVE_RATIO_MEASURE(2700.),#24592);
#24613=MEASURE_REPRESENTATION_ITEM('density measure',
POSITIVE_RATIO_MEASURE(2700.),#24593);
#24614=MEASURE_REPRESENTATION_ITEM('density measure',
POSITIVE_RATIO_MEASURE(2700.),#24594);
#24615=MEASURE_REPRESENTATION_ITEM('density measure',
POSITIVE_RATIO_MEASURE(2700.),#24595);
#24616=MEASURE_REPRESENTATION_ITEM('density measure',
POSITIVE_RATIO_MEASURE(7850.),#24596);
#24617=MEASURE_REPRESENTATION_ITEM('density measure',
POSITIVE_RATIO_MEASURE(2700.),#24597);
#24618=MEASURE_REPRESENTATION_ITEM('density measure',
POSITIVE_RATIO_MEASURE(2700.),#24598);
#24619=MEASURE_REPRESENTATION_ITEM('density measure',
POSITIVE_RATIO_MEASURE(8000.),#24599);
#24620=MEASURE_REPRESENTATION_ITEM('density measure',
POSITIVE_RATIO_MEASURE(1060.),#24600);
#24621=MEASURE_REPRESENTATION_ITEM('density measure',
POSITIVE_RATIO_MEASURE(8000.),#24601);
#24622=MEASURE_REPRESENTATION_ITEM('density measure',
POSITIVE_RATIO_MEASURE(1060.),#24602);
#24623=MEASURE_REPRESENTATION_ITEM('density measure',
POSITIVE_RATIO_MEASURE(7850.),#24603);
#24624=MEASURE_REPRESENTATION_ITEM('density measure',
POSITIVE_RATIO_MEASURE(8470.),#24604);
#24625=MEASURE_REPRESENTATION_ITEM('density measure',
POSITIVE_RATIO_MEASURE(8000.),#24605);
#24626=MEASURE_REPRESENTATION_ITEM('density measure',
POSITIVE_RATIO_MEASURE(8000.),#24606);
#24627=MEASURE_REPRESENTATION_ITEM('density measure',
POSITIVE_RATIO_MEASURE(8000.),#24607);
#24628=MEASURE_REPRESENTATION_ITEM('density measure',
POSITIVE_RATIO_MEASURE(8000.),#24608);
#24629=MEASURE_REPRESENTATION_ITEM('density measure',
POSITIVE_RATIO_MEASURE(8000.),#24609);
#24630=PROPERTY_DEFINITION_REPRESENTATION(#24730,#24670);
#24631=PROPERTY_DEFINITION_REPRESENTATION(#24731,#24671);
#24632=PROPERTY_DEFINITION_REPRESENTATION(#24732,#24672);
#24633=PROPERTY_DEFINITION_REPRESENTATION(#24733,#24673);
#24634=PROPERTY_DEFINITION_REPRESENTATION(#24734,#24674);
#24635=PROPERTY_DEFINITION_REPRESENTATION(#24735,#24675);
#24636=PROPERTY_DEFINITION_REPRESENTATION(#24736,#24676);
#24637=PROPERTY_DEFINITION_REPRESENTATION(#24737,#24677);
#24638=PROPERTY_DEFINITION_REPRESENTATION(#24738,#24678);
#24639=PROPERTY_DEFINITION_REPRESENTATION(#24739,#24679);
#24640=PROPERTY_DEFINITION_REPRESENTATION(#24740,#24680);
#24641=PROPERTY_DEFINITION_REPRESENTATION(#24741,#24681);
#24642=PROPERTY_DEFINITION_REPRESENTATION(#24742,#24682);
#24643=PROPERTY_DEFINITION_REPRESENTATION(#24743,#24683);
#24644=PROPERTY_DEFINITION_REPRESENTATION(#24744,#24684);
#24645=PROPERTY_DEFINITION_REPRESENTATION(#24745,#24685);
#24646=PROPERTY_DEFINITION_REPRESENTATION(#24746,#24686);
#24647=PROPERTY_DEFINITION_REPRESENTATION(#24747,#24687);
#24648=PROPERTY_DEFINITION_REPRESENTATION(#24748,#24688);
#24649=PROPERTY_DEFINITION_REPRESENTATION(#24749,#24689);
#24650=PROPERTY_DEFINITION_REPRESENTATION(#24750,#24690);
#24651=PROPERTY_DEFINITION_REPRESENTATION(#24751,#24691);
#24652=PROPERTY_DEFINITION_REPRESENTATION(#24752,#24692);
#24653=PROPERTY_DEFINITION_REPRESENTATION(#24753,#24693);
#24654=PROPERTY_DEFINITION_REPRESENTATION(#24754,#24694);
#24655=PROPERTY_DEFINITION_REPRESENTATION(#24755,#24695);
#24656=PROPERTY_DEFINITION_REPRESENTATION(#24756,#24696);
#24657=PROPERTY_DEFINITION_REPRESENTATION(#24757,#24697);
#24658=PROPERTY_DEFINITION_REPRESENTATION(#24758,#24698);
#24659=PROPERTY_DEFINITION_REPRESENTATION(#24759,#24699);
#24660=PROPERTY_DEFINITION_REPRESENTATION(#24760,#24700);
#24661=PROPERTY_DEFINITION_REPRESENTATION(#24761,#24701);
#24662=PROPERTY_DEFINITION_REPRESENTATION(#24762,#24702);
#24663=PROPERTY_DEFINITION_REPRESENTATION(#24763,#24703);
#24664=PROPERTY_DEFINITION_REPRESENTATION(#24764,#24704);
#24665=PROPERTY_DEFINITION_REPRESENTATION(#24765,#24705);
#24666=PROPERTY_DEFINITION_REPRESENTATION(#24766,#24706);
#24667=PROPERTY_DEFINITION_REPRESENTATION(#24767,#24707);
#24668=PROPERTY_DEFINITION_REPRESENTATION(#24768,#24708);
#24669=PROPERTY_DEFINITION_REPRESENTATION(#24769,#24709);
#24670=REPRESENTATION('material name',(#24710),#54982);
#24671=REPRESENTATION('density',(#24610),#54982);
#24672=REPRESENTATION('material name',(#24711),#54983);
#24673=REPRESENTATION('density',(#24611),#54983);
#24674=REPRESENTATION('material name',(#24712),#54984);
#24675=REPRESENTATION('density',(#24612),#54984);
#24676=REPRESENTATION('material name',(#24713),#54985);
#24677=REPRESENTATION('density',(#24613),#54985);
#24678=REPRESENTATION('material name',(#24714),#54986);
#24679=REPRESENTATION('density',(#24614),#54986);
#24680=REPRESENTATION('material name',(#24715),#54987);
#24681=REPRESENTATION('density',(#24615),#54987);
#24682=REPRESENTATION('material name',(#24716),#54988);
#24683=REPRESENTATION('density',(#24616),#54988);
#24684=REPRESENTATION('material name',(#24717),#54989);
#24685=REPRESENTATION('density',(#24617),#54989);
#24686=REPRESENTATION('material name',(#24718),#54990);
#24687=REPRESENTATION('density',(#24618),#54990);
#24688=REPRESENTATION('material name',(#24719),#54991);
#24689=REPRESENTATION('density',(#24619),#54991);
#24690=REPRESENTATION('material name',(#24720),#54992);
#24691=REPRESENTATION('density',(#24620),#54992);
#24692=REPRESENTATION('material name',(#24721),#54993);
#24693=REPRESENTATION('density',(#24621),#54993);
#24694=REPRESENTATION('material name',(#24722),#54994);
#24695=REPRESENTATION('density',(#24622),#54994);
#24696=REPRESENTATION('material name',(#24723),#54995);
#24697=REPRESENTATION('density',(#24623),#54995);
#24698=REPRESENTATION('material name',(#24724),#54996);
#24699=REPRESENTATION('density',(#24624),#54996);
#24700=REPRESENTATION('material name',(#24725),#54997);
#24701=REPRESENTATION('density',(#24625),#54997);
#24702=REPRESENTATION('material name',(#24726),#54998);
#24703=REPRESENTATION('density',(#24626),#54998);
#24704=REPRESENTATION('material name',(#24727),#54999);
#24705=REPRESENTATION('density',(#24627),#54999);
#24706=REPRESENTATION('material name',(#24728),#55000);
#24707=REPRESENTATION('density',(#24628),#55000);
#24708=REPRESENTATION('material name',(#24729),#55001);
#24709=REPRESENTATION('density',(#24629),#55001);
#24710=DESCRIPTIVE_REPRESENTATION_ITEM('Aluminum 6061','Aluminum 6061');
#24711=DESCRIPTIVE_REPRESENTATION_ITEM('Aluminum 6061','Aluminum 6061');
#24712=DESCRIPTIVE_REPRESENTATION_ITEM('Aluminum 6061','Aluminum 6061');
#24713=DESCRIPTIVE_REPRESENTATION_ITEM('Aluminum 6061','Aluminum 6061');
#24714=DESCRIPTIVE_REPRESENTATION_ITEM('Aluminum 6061','Aluminum 6061');
#24715=DESCRIPTIVE_REPRESENTATION_ITEM('Aluminum 6061','Aluminum 6061');
#24716=DESCRIPTIVE_REPRESENTATION_ITEM('Steel','Steel');
#24717=DESCRIPTIVE_REPRESENTATION_ITEM('Aluminum 6061','Aluminum 6061');
#24718=DESCRIPTIVE_REPRESENTATION_ITEM('Aluminum 6061','Aluminum 6061');
#24719=DESCRIPTIVE_REPRESENTATION_ITEM('Stainless Steel AISI 304',
'Stainless Steel AISI 304');
#24720=DESCRIPTIVE_REPRESENTATION_ITEM('ABS Plastic','ABS Plastic');
#24721=DESCRIPTIVE_REPRESENTATION_ITEM('Stainless Steel AISI 304',
'Stainless Steel AISI 304');
#24722=DESCRIPTIVE_REPRESENTATION_ITEM('ABS Plastic','ABS Plastic');
#24723=DESCRIPTIVE_REPRESENTATION_ITEM('Steel','Steel');
#24724=DESCRIPTIVE_REPRESENTATION_ITEM('Brass, Soft Yellow',
'Brass, Soft Yellow');
#24725=DESCRIPTIVE_REPRESENTATION_ITEM('Stainless Steel AISI 304',
'Stainless Steel AISI 304');
#24726=DESCRIPTIVE_REPRESENTATION_ITEM('Stainless Steel AISI 304',
'Stainless Steel AISI 304');
#24727=DESCRIPTIVE_REPRESENTATION_ITEM('Stainless Steel AISI 304',
'Stainless Steel AISI 304');
#24728=DESCRIPTIVE_REPRESENTATION_ITEM('Stainless Steel AISI 304',
'Stainless Steel AISI 304');
#24729=DESCRIPTIVE_REPRESENTATION_ITEM('Stainless Steel AISI 304',
'Stainless Steel AISI 304');
#24730=PROPERTY_DEFINITION('material property','material name',#55126);
#24731=PROPERTY_DEFINITION('material property','density of part',#55126);
#24732=PROPERTY_DEFINITION('material property','material name',#55127);
#24733=PROPERTY_DEFINITION('material property','density of part',#55127);
#24734=PROPERTY_DEFINITION('material property','material name',#55128);
#24735=PROPERTY_DEFINITION('material property','density of part',#55128);
#24736=PROPERTY_DEFINITION('material property','material name',#55129);
#24737=PROPERTY_DEFINITION('material property','density of part',#55129);
#24738=PROPERTY_DEFINITION('material property','material name',#55130);
#24739=PROPERTY_DEFINITION('material property','density of part',#55130);
#24740=PROPERTY_DEFINITION('material property','material name',#55131);
#24741=PROPERTY_DEFINITION('material property','density of part',#55131);
#24742=PROPERTY_DEFINITION('material property','material name',#55132);
#24743=PROPERTY_DEFINITION('material property','density of part',#55132);
#24744=PROPERTY_DEFINITION('material property','material name',#55133);
#24745=PROPERTY_DEFINITION('material property','density of part',#55133);
#24746=PROPERTY_DEFINITION('material property','material name',#55134);
#24747=PROPERTY_DEFINITION('material property','density of part',#55134);
#24748=PROPERTY_DEFINITION('material property','material name',#55135);
#24749=PROPERTY_DEFINITION('material property','density of part',#55135);
#24750=PROPERTY_DEFINITION('material property','material name',#55136);
#24751=PROPERTY_DEFINITION('material property','density of part',#55136);
#24752=PROPERTY_DEFINITION('material property','material name',#55137);
#24753=PROPERTY_DEFINITION('material property','density of part',#55137);
#24754=PROPERTY_DEFINITION('material property','material name',#55138);
#24755=PROPERTY_DEFINITION('material property','density of part',#55138);
#24756=PROPERTY_DEFINITION('material property','material name',#55139);
#24757=PROPERTY_DEFINITION('material property','density of part',#55139);
#24758=PROPERTY_DEFINITION('material property','material name',#55140);
#24759=PROPERTY_DEFINITION('material property','density of part',#55140);
#24760=PROPERTY_DEFINITION('material property','material name',#55141);
#24761=PROPERTY_DEFINITION('material property','density of part',#55141);
#24762=PROPERTY_DEFINITION('material property','material name',#55142);
#24763=PROPERTY_DEFINITION('material property','density of part',#55142);
#24764=PROPERTY_DEFINITION('material property','material name',#55143);
#24765=PROPERTY_DEFINITION('material property','density of part',#55143);
#24766=PROPERTY_DEFINITION('material property','material name',#55144);
#24767=PROPERTY_DEFINITION('material property','density of part',#55144);
#24768=PROPERTY_DEFINITION('material property','material name',#55145);
#24769=PROPERTY_DEFINITION('material property','density of part',#55145);
#24770=AXIS2_PLACEMENT_3D('',#33869,#27196,#27197);
#24771=AXIS2_PLACEMENT_3D('',#33870,#27198,#27199);
#24772=AXIS2_PLACEMENT_3D('',#33871,#27200,#27201);
#24773=AXIS2_PLACEMENT_3D('',#33873,#27202,#27203);
#24774=AXIS2_PLACEMENT_3D('',#33877,#27205,#27206);
#24775=AXIS2_PLACEMENT_3D('',#33878,#27207,#27208);
#24776=AXIS2_PLACEMENT_3D('',#33879,#27209,#27210);
#24777=AXIS2_PLACEMENT_3D('',#33882,#27212,#27213);
#24778=AXIS2_PLACEMENT_3D('',#33883,#27214,#27215);
#24779=AXIS2_PLACEMENT_3D('',#33885,#27216,#27217);
#24780=AXIS2_PLACEMENT_3D('',#33887,#27219,#27220);
#24781=AXIS2_PLACEMENT_3D('',#33889,#27221,#27222);
#24782=AXIS2_PLACEMENT_3D('',#33892,#27224,#27225);
#24783=AXIS2_PLACEMENT_3D('',#33893,#27226,#27227);
#24784=AXIS2_PLACEMENT_3D('',#33896,#27229,#27230);
#24785=AXIS2_PLACEMENT_3D('',#33897,#27231,#27232);
#24786=AXIS2_PLACEMENT_3D('',#33899,#27233,#27234);
#24787=AXIS2_PLACEMENT_3D('',#33901,#27235,#27236);
#24788=AXIS2_PLACEMENT_3D('',#33903,#27237,#27238);
#24789=AXIS2_PLACEMENT_3D('',#33905,#27239,#27240);
#24790=AXIS2_PLACEMENT_3D('',#33907,#27241,#27242);
#24791=AXIS2_PLACEMENT_3D('',#33909,#27243,#27244);
#24792=AXIS2_PLACEMENT_3D('',#33911,#27245,#27246);
#24793=AXIS2_PLACEMENT_3D('',#33912,#27247,#27248);
#24794=AXIS2_PLACEMENT_3D('',#33915,#27250,#27251);
#24795=AXIS2_PLACEMENT_3D('',#33916,#27252,#27253);
#24796=AXIS2_PLACEMENT_3D('',#33918,#27254,#27255);
#24797=AXIS2_PLACEMENT_3D('',#33920,#27256,#27257);
#24798=AXIS2_PLACEMENT_3D('',#33922,#27258,#27259);
#24799=AXIS2_PLACEMENT_3D('',#33924,#27260,#27261);
#24800=AXIS2_PLACEMENT_3D('',#33926,#27262,#27263);
#24801=AXIS2_PLACEMENT_3D('',#33928,#27264,#27265);
#24802=AXIS2_PLACEMENT_3D('',#33930,#27266,#27267);
#24803=AXIS2_PLACEMENT_3D('',#33931,#27268,#27269);
#24804=AXIS2_PLACEMENT_3D('',#33933,#27270,#27271);
#24805=AXIS2_PLACEMENT_3D('',#33935,#27273,#27274);
#24806=AXIS2_PLACEMENT_3D('',#33938,#27276,#27277);
#24807=AXIS2_PLACEMENT_3D('',#33939,#27278,#27279);
#24808=AXIS2_PLACEMENT_3D('',#33943,#27281,#27282);
#24809=AXIS2_PLACEMENT_3D('',#33944,#27283,#27284);
#24810=AXIS2_PLACEMENT_3D('',#33945,#27285,#27286);
#24811=AXIS2_PLACEMENT_3D('',#33948,#27287,#27288);
#24812=AXIS2_PLACEMENT_3D('',#33949,#27289,#27290);
#24813=AXIS2_PLACEMENT_3D('',#33951,#27292,#27293);
#24814=AXIS2_PLACEMENT_3D('',#33953,#27294,#27295);
#24815=AXIS2_PLACEMENT_3D('',#33955,#27297,#27298);
#24816=AXIS2_PLACEMENT_3D('',#33958,#27300,#27301);
#24817=AXIS2_PLACEMENT_3D('',#33959,#27302,#27303);
#24818=AXIS2_PLACEMENT_3D('',#33962,#27305,#27306);
#24819=AXIS2_PLACEMENT_3D('',#33963,#27307,#27308);
#24820=AXIS2_PLACEMENT_3D('',#33965,#27309,#27310);
#24821=AXIS2_PLACEMENT_3D('',#33967,#27311,#27312);
#24822=AXIS2_PLACEMENT_3D('',#33969,#27313,#27314);
#24823=AXIS2_PLACEMENT_3D('',#33971,#27315,#27316);
#24824=AXIS2_PLACEMENT_3D('',#33972,#27317,#27318);
#24825=AXIS2_PLACEMENT_3D('',#33976,#27320,#27321);
#24826=AXIS2_PLACEMENT_3D('',#33977,#27322,#27323);
#24827=AXIS2_PLACEMENT_3D('',#33978,#27324,#27325);
#24828=AXIS2_PLACEMENT_3D('',#33980,#27326,#27327);
#24829=AXIS2_PLACEMENT_3D('',#33982,#27329,#27330);
#24830=AXIS2_PLACEMENT_3D('',#33986,#27332,#27333);
#24831=AXIS2_PLACEMENT_3D('',#33987,#27334,#27335);
#24832=AXIS2_PLACEMENT_3D('',#33988,#27336,#27337);
#24833=AXIS2_PLACEMENT_3D('',#33990,#27338,#27339);
#24834=AXIS2_PLACEMENT_3D('',#33992,#27341,#27342);
#24835=AXIS2_PLACEMENT_3D('',#33996,#27344,#27345);
#24836=AXIS2_PLACEMENT_3D('',#33997,#27346,#27347);
#24837=AXIS2_PLACEMENT_3D('',#33998,#27348,#27349);
#24838=AXIS2_PLACEMENT_3D('',#34000,#27350,#27351);
#24839=AXIS2_PLACEMENT_3D('',#34002,#27353,#27354);
#24840=AXIS2_PLACEMENT_3D('',#34006,#27356,#27357);
#24841=AXIS2_PLACEMENT_3D('',#34007,#27358,#27359);
#24842=AXIS2_PLACEMENT_3D('',#34008,#27360,#27361);
#24843=AXIS2_PLACEMENT_3D('',#34010,#27362,#27363);
#24844=AXIS2_PLACEMENT_3D('',#34012,#27365,#27366);
#24845=AXIS2_PLACEMENT_3D('',#34016,#27368,#27369);
#24846=AXIS2_PLACEMENT_3D('',#34017,#27370,#27371);
#24847=AXIS2_PLACEMENT_3D('',#34018,#27372,#27373);
#24848=AXIS2_PLACEMENT_3D('',#34020,#27374,#27375);
#24849=AXIS2_PLACEMENT_3D('',#34022,#27377,#27378);
#24850=AXIS2_PLACEMENT_3D('',#34026,#27380,#27381);
#24851=AXIS2_PLACEMENT_3D('',#34027,#27382,#27383);
#24852=AXIS2_PLACEMENT_3D('',#34028,#27384,#27385);
#24853=AXIS2_PLACEMENT_3D('',#34030,#27386,#27387);
#24854=AXIS2_PLACEMENT_3D('',#34032,#27389,#27390);
#24855=AXIS2_PLACEMENT_3D('',#34036,#27392,#27393);
#24856=AXIS2_PLACEMENT_3D('',#34037,#27394,#27395);
#24857=AXIS2_PLACEMENT_3D('',#34038,#27396,#27397);
#24858=AXIS2_PLACEMENT_3D('',#34041,#27399,#27400);
#24859=AXIS2_PLACEMENT_3D('',#34042,#27401,#27402);
#24860=AXIS2_PLACEMENT_3D('',#34045,#27404,#27405);
#24861=AXIS2_PLACEMENT_3D('',#34046,#27406,#27407);
#24862=AXIS2_PLACEMENT_3D('',#34048,#27408,#27409);
#24863=AXIS2_PLACEMENT_3D('',#34049,#27410,#27411);
#24864=AXIS2_PLACEMENT_3D('',#34052,#27413,#27414);
#24865=AXIS2_PLACEMENT_3D('',#34053,#27415,#27416);
#24866=AXIS2_PLACEMENT_3D('',#34055,#27417,#27418);
#24867=AXIS2_PLACEMENT_3D('',#34056,#27419,#27420);
#24868=AXIS2_PLACEMENT_3D('',#34058,#27422,#27423);
#24869=AXIS2_PLACEMENT_3D('',#34062,#27425,#27426);
#24870=AXIS2_PLACEMENT_3D('',#34063,#27427,#27428);
#24871=AXIS2_PLACEMENT_3D('',#34066,#27430,#27431);
#24872=AXIS2_PLACEMENT_3D('',#34067,#27432,#27433);
#24873=AXIS2_PLACEMENT_3D('',#34069,#27435,#27436);
#24874=AXIS2_PLACEMENT_3D('',#34073,#27438,#27439);
#24875=AXIS2_PLACEMENT_3D('',#34074,#27440,#27441);
#24876=AXIS2_PLACEMENT_3D('',#34077,#27443,#27444);
#24877=AXIS2_PLACEMENT_3D('',#34078,#27445,#27446);
#24878=AXIS2_PLACEMENT_3D('',#34080,#27448,#27449);
#24879=AXIS2_PLACEMENT_3D('',#34084,#27451,#27452);
#24880=AXIS2_PLACEMENT_3D('',#34085,#27453,#27454);
#24881=AXIS2_PLACEMENT_3D('',#34088,#27456,#27457);
#24882=AXIS2_PLACEMENT_3D('',#34089,#27458,#27459);
#24883=AXIS2_PLACEMENT_3D('',#34091,#27461,#27462);
#24884=AXIS2_PLACEMENT_3D('',#34094,#27464,#27465);
#24885=AXIS2_PLACEMENT_3D('',#34095,#27466,#27467);
#24886=AXIS2_PLACEMENT_3D('',#34098,#27469,#27470);
#24887=AXIS2_PLACEMENT_3D('',#34099,#27471,#27472);
#24888=AXIS2_PLACEMENT_3D('',#34102,#27474,#27475);
#24889=AXIS2_PLACEMENT_3D('',#34103,#27476,#27477);
#24890=AXIS2_PLACEMENT_3D('',#34104,#27478,#27479);
#24891=AXIS2_PLACEMENT_3D('',#34107,#27481,#27482);
#24892=AXIS2_PLACEMENT_3D('',#34108,#27483,#27484);
#24893=AXIS2_PLACEMENT_3D('',#34111,#27486,#27487);
#24894=AXIS2_PLACEMENT_3D('',#34112,#27488,#27489);
#24895=AXIS2_PLACEMENT_3D('',#34115,#27491,#27492);
#24896=AXIS2_PLACEMENT_3D('',#34116,#27493,#27494);
#24897=AXIS2_PLACEMENT_3D('',#34117,#27495,#27496);
#24898=AXIS2_PLACEMENT_3D('',#34120,#27498,#27499);
#24899=AXIS2_PLACEMENT_3D('',#34121,#27500,#27501);
#24900=AXIS2_PLACEMENT_3D('',#34124,#27503,#27504);
#24901=AXIS2_PLACEMENT_3D('',#34125,#27505,#27506);
#24902=AXIS2_PLACEMENT_3D('',#34128,#27508,#27509);
#24903=AXIS2_PLACEMENT_3D('',#34129,#27510,#27511);
#24904=AXIS2_PLACEMENT_3D('',#34130,#27512,#27513);
#24905=AXIS2_PLACEMENT_3D('',#34133,#27515,#27516);
#24906=AXIS2_PLACEMENT_3D('',#34134,#27517,#27518);
#24907=AXIS2_PLACEMENT_3D('',#34137,#27520,#27521);
#24908=AXIS2_PLACEMENT_3D('',#34138,#27522,#27523);
#24909=AXIS2_PLACEMENT_3D('',#34141,#27525,#27526);
#24910=AXIS2_PLACEMENT_3D('',#34142,#27527,#27528);
#24911=AXIS2_PLACEMENT_3D('',#34143,#27529,#27530);
#24912=AXIS2_PLACEMENT_3D('',#34146,#27532,#27533);
#24913=AXIS2_PLACEMENT_3D('',#34147,#27534,#27535);
#24914=AXIS2_PLACEMENT_3D('',#34150,#27537,#27538);
#24915=AXIS2_PLACEMENT_3D('',#34151,#27539,#27540);
#24916=AXIS2_PLACEMENT_3D('',#34154,#27542,#27543);
#24917=AXIS2_PLACEMENT_3D('',#34155,#27544,#27545);
#24918=AXIS2_PLACEMENT_3D('',#34156,#27546,#27547);
#24919=AXIS2_PLACEMENT_3D('',#34159,#27549,#27550);
#24920=AXIS2_PLACEMENT_3D('',#34160,#27551,#27552);
#24921=AXIS2_PLACEMENT_3D('',#34163,#27554,#27555);
#24922=AXIS2_PLACEMENT_3D('',#34164,#27556,#27557);
#24923=AXIS2_PLACEMENT_3D('',#34167,#27559,#27560);
#24924=AXIS2_PLACEMENT_3D('',#34168,#27561,#27562);
#24925=AXIS2_PLACEMENT_3D('',#34169,#27563,#27564);
#24926=AXIS2_PLACEMENT_3D('',#34173,#27566,#27567);
#24927=AXIS2_PLACEMENT_3D('',#34174,#27568,#27569);
#24928=AXIS2_PLACEMENT_3D('',#34175,#27570,#27571);
#24929=AXIS2_PLACEMENT_3D('',#34177,#27573,#27574);
#24930=AXIS2_PLACEMENT_3D('',#34178,#27575,#27576);
#24931=AXIS2_PLACEMENT_3D('',#34182,#27578,#27579);
#24932=AXIS2_PLACEMENT_3D('',#34183,#27580,#27581);
#24933=AXIS2_PLACEMENT_3D('',#34186,#27583,#27584);
#24934=AXIS2_PLACEMENT_3D('',#34187,#27585,#27586);
#24935=AXIS2_PLACEMENT_3D('',#34190,#27588,#27589);
#24936=AXIS2_PLACEMENT_3D('',#34191,#27590,#27591);
#24937=AXIS2_PLACEMENT_3D('',#34195,#27593,#27594);
#24938=AXIS2_PLACEMENT_3D('',#34196,#27595,#27596);
#24939=AXIS2_PLACEMENT_3D('',#34199,#27598,#27599);
#24940=AXIS2_PLACEMENT_3D('',#34200,#27600,#27601);
#24941=AXIS2_PLACEMENT_3D('',#34203,#27603,#27604);
#24942=AXIS2_PLACEMENT_3D('',#34204,#27605,#27606);
#24943=AXIS2_PLACEMENT_3D('',#34208,#27608,#27609);
#24944=AXIS2_PLACEMENT_3D('',#34209,#27610,#27611);
#24945=AXIS2_PLACEMENT_3D('',#34212,#27613,#27614);
#24946=AXIS2_PLACEMENT_3D('',#34213,#27615,#27616);
#24947=AXIS2_PLACEMENT_3D('',#34216,#27618,#27619);
#24948=AXIS2_PLACEMENT_3D('',#34217,#27620,#27621);
#24949=AXIS2_PLACEMENT_3D('',#34221,#27623,#27624);
#24950=AXIS2_PLACEMENT_3D('',#34222,#27625,#27626);
#24951=AXIS2_PLACEMENT_3D('',#34225,#27628,#27629);
#24952=AXIS2_PLACEMENT_3D('',#34226,#27630,#27631);
#24953=AXIS2_PLACEMENT_3D('',#34229,#27633,#27634);
#24954=AXIS2_PLACEMENT_3D('',#34230,#27635,#27636);
#24955=AXIS2_PLACEMENT_3D('',#34234,#27638,#27639);
#24956=AXIS2_PLACEMENT_3D('',#34235,#27640,#27641);
#24957=AXIS2_PLACEMENT_3D('',#34238,#27643,#27644);
#24958=AXIS2_PLACEMENT_3D('',#34239,#27645,#27646);
#24959=AXIS2_PLACEMENT_3D('',#34242,#27648,#27649);
#24960=AXIS2_PLACEMENT_3D('',#34243,#27650,#27651);
#24961=AXIS2_PLACEMENT_3D('',#34247,#27653,#27654);
#24962=AXIS2_PLACEMENT_3D('',#34248,#27655,#27656);
#24963=AXIS2_PLACEMENT_3D('',#34251,#27658,#27659);
#24964=AXIS2_PLACEMENT_3D('',#34252,#27660,#27661);
#24965=AXIS2_PLACEMENT_3D('',#34255,#27663,#27664);
#24966=AXIS2_PLACEMENT_3D('',#34256,#27665,#27666);
#24967=AXIS2_PLACEMENT_3D('',#34260,#27668,#27669);
#24968=AXIS2_PLACEMENT_3D('',#34261,#27670,#27671);
#24969=AXIS2_PLACEMENT_3D('',#34264,#27673,#27674);
#24970=AXIS2_PLACEMENT_3D('',#34265,#27675,#27676);
#24971=AXIS2_PLACEMENT_3D('',#34268,#27678,#27679);
#24972=AXIS2_PLACEMENT_3D('',#34269,#27680,#27681);
#24973=AXIS2_PLACEMENT_3D('',#34273,#27683,#27684);
#24974=AXIS2_PLACEMENT_3D('',#34274,#27685,#27686);
#24975=AXIS2_PLACEMENT_3D('',#34277,#27688,#27689);
#24976=AXIS2_PLACEMENT_3D('',#34278,#27690,#27691);
#24977=AXIS2_PLACEMENT_3D('',#34281,#27693,#27694);
#24978=AXIS2_PLACEMENT_3D('',#34282,#27695,#27696);
#24979=AXIS2_PLACEMENT_3D('',#34286,#27698,#27699);
#24980=AXIS2_PLACEMENT_3D('',#34287,#27700,#27701);
#24981=AXIS2_PLACEMENT_3D('',#34290,#27703,#27704);
#24982=AXIS2_PLACEMENT_3D('',#34291,#27705,#27706);
#24983=AXIS2_PLACEMENT_3D('',#34294,#27708,#27709);
#24984=AXIS2_PLACEMENT_3D('',#34295,#27710,#27711);
#24985=AXIS2_PLACEMENT_3D('',#34299,#27713,#27714);
#24986=AXIS2_PLACEMENT_3D('',#34300,#27715,#27716);
#24987=AXIS2_PLACEMENT_3D('',#34303,#27718,#27719);
#24988=AXIS2_PLACEMENT_3D('',#34304,#27720,#27721);
#24989=AXIS2_PLACEMENT_3D('',#34307,#27723,#27724);
#24990=AXIS2_PLACEMENT_3D('',#34308,#27725,#27726);
#24991=AXIS2_PLACEMENT_3D('',#34312,#27728,#27729);
#24992=AXIS2_PLACEMENT_3D('',#34313,#27730,#27731);
#24993=AXIS2_PLACEMENT_3D('',#34316,#27733,#27734);
#24994=AXIS2_PLACEMENT_3D('',#34317,#27735,#27736);
#24995=AXIS2_PLACEMENT_3D('',#34320,#27738,#27739);
#24996=AXIS2_PLACEMENT_3D('',#34321,#27740,#27741);
#24997=AXIS2_PLACEMENT_3D('',#34325,#27743,#27744);
#24998=AXIS2_PLACEMENT_3D('',#34326,#27745,#27746);
#24999=AXIS2_PLACEMENT_3D('',#34329,#27748,#27749);
#25000=AXIS2_PLACEMENT_3D('',#34330,#27750,#27751);
#25001=AXIS2_PLACEMENT_3D('',#34333,#27753,#27754);
#25002=AXIS2_PLACEMENT_3D('',#34334,#27755,#27756);
#25003=AXIS2_PLACEMENT_3D('',#34338,#27758,#27759);
#25004=AXIS2_PLACEMENT_3D('',#34339,#27760,#27761);
#25005=AXIS2_PLACEMENT_3D('',#34342,#27763,#27764);
#25006=AXIS2_PLACEMENT_3D('',#34343,#27765,#27766);
#25007=AXIS2_PLACEMENT_3D('',#34346,#27768,#27769);
#25008=AXIS2_PLACEMENT_3D('',#34347,#27770,#27771);
#25009=AXIS2_PLACEMENT_3D('',#34351,#27773,#27774);
#25010=AXIS2_PLACEMENT_3D('',#34352,#27775,#27776);
#25011=AXIS2_PLACEMENT_3D('',#34355,#27778,#27779);
#25012=AXIS2_PLACEMENT_3D('',#34356,#27780,#27781);
#25013=AXIS2_PLACEMENT_3D('',#34359,#27783,#27784);
#25014=AXIS2_PLACEMENT_3D('',#34360,#27785,#27786);
#25015=AXIS2_PLACEMENT_3D('',#34364,#27788,#27789);
#25016=AXIS2_PLACEMENT_3D('',#34365,#27790,#27791);
#25017=AXIS2_PLACEMENT_3D('',#34368,#27793,#27794);
#25018=AXIS2_PLACEMENT_3D('',#34369,#27795,#27796);
#25019=AXIS2_PLACEMENT_3D('',#34372,#27798,#27799);
#25020=AXIS2_PLACEMENT_3D('',#34373,#27800,#27801);
#25021=AXIS2_PLACEMENT_3D('',#34377,#27803,#27804);
#25022=AXIS2_PLACEMENT_3D('',#34378,#27805,#27806);
#25023=AXIS2_PLACEMENT_3D('',#34381,#27808,#27809);
#25024=AXIS2_PLACEMENT_3D('',#34382,#27810,#27811);
#25025=AXIS2_PLACEMENT_3D('',#34385,#27813,#27814);
#25026=AXIS2_PLACEMENT_3D('',#34386,#27815,#27816);
#25027=AXIS2_PLACEMENT_3D('',#34390,#27818,#27819);
#25028=AXIS2_PLACEMENT_3D('',#34391,#27820,#27821);
#25029=AXIS2_PLACEMENT_3D('',#34394,#27823,#27824);
#25030=AXIS2_PLACEMENT_3D('',#34395,#27825,#27826);
#25031=AXIS2_PLACEMENT_3D('',#34398,#27828,#27829);
#25032=AXIS2_PLACEMENT_3D('',#34399,#27830,#27831);
#25033=AXIS2_PLACEMENT_3D('',#34403,#27833,#27834);
#25034=AXIS2_PLACEMENT_3D('',#34404,#27835,#27836);
#25035=AXIS2_PLACEMENT_3D('',#34407,#27838,#27839);
#25036=AXIS2_PLACEMENT_3D('',#34408,#27840,#27841);
#25037=AXIS2_PLACEMENT_3D('',#34411,#27843,#27844);
#25038=AXIS2_PLACEMENT_3D('',#34412,#27845,#27846);
#25039=AXIS2_PLACEMENT_3D('',#34414,#27847,#27848);
#25040=AXIS2_PLACEMENT_3D('',#34418,#27850,#27851);
#25041=AXIS2_PLACEMENT_3D('',#34419,#27852,#27853);
#25042=AXIS2_PLACEMENT_3D('',#34420,#27854,#27855);
#25043=AXIS2_PLACEMENT_3D('',#34423,#27856,#27857);
#25044=AXIS2_PLACEMENT_3D('',#34424,#27858,#27859);
#25045=AXIS2_PLACEMENT_3D('',#34426,#27861,#27862);
#25046=AXIS2_PLACEMENT_3D('',#34428,#27863,#27864);
#25047=AXIS2_PLACEMENT_3D('',#34429,#27865,#27866);
#25048=AXIS2_PLACEMENT_3D('',#34432,#27868,#27869);
#25049=AXIS2_PLACEMENT_3D('',#34433,#27870,#27871);
#25050=AXIS2_PLACEMENT_3D('',#34435,#27872,#27873);
#25051=AXIS2_PLACEMENT_3D('',#34436,#27874,#27875);
#25052=AXIS2_PLACEMENT_3D('',#34440,#27877,#27878);
#25053=AXIS2_PLACEMENT_3D('',#34441,#27879,#27880);
#25054=AXIS2_PLACEMENT_3D('',#34442,#27881,#27882);
#25055=AXIS2_PLACEMENT_3D('',#34446,#27884,#27885);
#25056=AXIS2_PLACEMENT_3D('',#34447,#27886,#27887);
#25057=AXIS2_PLACEMENT_3D('',#34448,#27888,#27889);
#25058=AXIS2_PLACEMENT_3D('',#34450,#27891,#27892);
#25059=AXIS2_PLACEMENT_3D('',#34451,#27893,#27894);
#25060=AXIS2_PLACEMENT_3D('',#34455,#27896,#27897);
#25061=AXIS2_PLACEMENT_3D('',#34456,#27898,#27899);
#25062=AXIS2_PLACEMENT_3D('',#34459,#27901,#27902);
#25063=AXIS2_PLACEMENT_3D('',#34460,#27903,#27904);
#25064=AXIS2_PLACEMENT_3D('',#34463,#27906,#27907);
#25065=AXIS2_PLACEMENT_3D('',#34464,#27908,#27909);
#25066=AXIS2_PLACEMENT_3D('',#34468,#27911,#27912);
#25067=AXIS2_PLACEMENT_3D('',#34469,#27913,#27914);
#25068=AXIS2_PLACEMENT_3D('',#34472,#27916,#27917);
#25069=AXIS2_PLACEMENT_3D('',#34473,#27918,#27919);
#25070=AXIS2_PLACEMENT_3D('',#34476,#27921,#27922);
#25071=AXIS2_PLACEMENT_3D('',#34477,#27923,#27924);
#25072=AXIS2_PLACEMENT_3D('',#34481,#27926,#27927);
#25073=AXIS2_PLACEMENT_3D('',#34482,#27928,#27929);
#25074=AXIS2_PLACEMENT_3D('',#34485,#27931,#27932);
#25075=AXIS2_PLACEMENT_3D('',#34486,#27933,#27934);
#25076=AXIS2_PLACEMENT_3D('',#34489,#27936,#27937);
#25077=AXIS2_PLACEMENT_3D('',#34490,#27938,#27939);
#25078=AXIS2_PLACEMENT_3D('',#34494,#27941,#27942);
#25079=AXIS2_PLACEMENT_3D('',#34495,#27943,#27944);
#25080=AXIS2_PLACEMENT_3D('',#34498,#27946,#27947);
#25081=AXIS2_PLACEMENT_3D('',#34499,#27948,#27949);
#25082=AXIS2_PLACEMENT_3D('',#34502,#27951,#27952);
#25083=AXIS2_PLACEMENT_3D('',#34503,#27953,#27954);
#25084=AXIS2_PLACEMENT_3D('',#34507,#27956,#27957);
#25085=AXIS2_PLACEMENT_3D('',#34508,#27958,#27959);
#25086=AXIS2_PLACEMENT_3D('',#34511,#27961,#27962);
#25087=AXIS2_PLACEMENT_3D('',#34512,#27963,#27964);
#25088=AXIS2_PLACEMENT_3D('',#34515,#27966,#27967);
#25089=AXIS2_PLACEMENT_3D('',#34516,#27968,#27969);
#25090=AXIS2_PLACEMENT_3D('',#34518,#27970,#27971);
#25091=AXIS2_PLACEMENT_3D('',#34521,#27973,#27974);
#25092=AXIS2_PLACEMENT_3D('',#34522,#27975,#27976);
#25093=AXIS2_PLACEMENT_3D('',#34525,#27978,#27979);
#25094=AXIS2_PLACEMENT_3D('',#34526,#27980,#27981);
#25095=AXIS2_PLACEMENT_3D('',#34529,#27983,#27984);
#25096=AXIS2_PLACEMENT_3D('',#34530,#27985,#27986);
#25097=AXIS2_PLACEMENT_3D('',#34532,#27987,#27988);
#25098=AXIS2_PLACEMENT_3D('',#34533,#27989,#27990);
#25099=AXIS2_PLACEMENT_3D('',#34536,#27992,#27993);
#25100=AXIS2_PLACEMENT_3D('',#34537,#27994,#27995);
#25101=AXIS2_PLACEMENT_3D('',#34539,#27996,#27997);
#25102=AXIS2_PLACEMENT_3D('',#34542,#27999,#28000);
#25103=AXIS2_PLACEMENT_3D('',#34543,#28001,#28002);
#25104=AXIS2_PLACEMENT_3D('',#34546,#28004,#28005);
#25105=AXIS2_PLACEMENT_3D('',#34547,#28006,#28007);
#25106=AXIS2_PLACEMENT_3D('',#34550,#28009,#28010);
#25107=AXIS2_PLACEMENT_3D('',#34551,#28011,#28012);
#25108=AXIS2_PLACEMENT_3D('',#34553,#28013,#28014);
#25109=AXIS2_PLACEMENT_3D('',#34554,#28015,#28016);
#25110=AXIS2_PLACEMENT_3D('',#34557,#28018,#28019);
#25111=AXIS2_PLACEMENT_3D('',#34558,#28020,#28021);
#25112=AXIS2_PLACEMENT_3D('',#34560,#28022,#28023);
#25113=AXIS2_PLACEMENT_3D('',#34563,#28025,#28026);
#25114=AXIS2_PLACEMENT_3D('',#34564,#28027,#28028);
#25115=AXIS2_PLACEMENT_3D('',#34567,#28030,#28031);
#25116=AXIS2_PLACEMENT_3D('',#34568,#28032,#28033);
#25117=AXIS2_PLACEMENT_3D('',#34571,#28035,#28036);
#25118=AXIS2_PLACEMENT_3D('',#34572,#28037,#28038);
#25119=AXIS2_PLACEMENT_3D('',#34574,#28039,#28040);
#25120=AXIS2_PLACEMENT_3D('',#34575,#28041,#28042);
#25121=AXIS2_PLACEMENT_3D('',#34578,#28044,#28045);
#25122=AXIS2_PLACEMENT_3D('',#34579,#28046,#28047);
#25123=AXIS2_PLACEMENT_3D('',#34581,#28048,#28049);
#25124=AXIS2_PLACEMENT_3D('',#34584,#28051,#28052);
#25125=AXIS2_PLACEMENT_3D('',#34585,#28053,#28054);
#25126=AXIS2_PLACEMENT_3D('',#34588,#28056,#28057);
#25127=AXIS2_PLACEMENT_3D('',#34589,#28058,#28059);
#25128=AXIS2_PLACEMENT_3D('',#34592,#28061,#28062);
#25129=AXIS2_PLACEMENT_3D('',#34593,#28063,#28064);
#25130=AXIS2_PLACEMENT_3D('',#34595,#28065,#28066);
#25131=AXIS2_PLACEMENT_3D('',#34596,#28067,#28068);
#25132=AXIS2_PLACEMENT_3D('',#34599,#28070,#28071);
#25133=AXIS2_PLACEMENT_3D('',#34600,#28072,#28073);
#25134=AXIS2_PLACEMENT_3D('',#34602,#28074,#28075);
#25135=AXIS2_PLACEMENT_3D('',#34605,#28077,#28078);
#25136=AXIS2_PLACEMENT_3D('',#34606,#28079,#28080);
#25137=AXIS2_PLACEMENT_3D('',#34609,#28082,#28083);
#25138=AXIS2_PLACEMENT_3D('',#34610,#28084,#28085);
#25139=AXIS2_PLACEMENT_3D('',#34613,#28087,#28088);
#25140=AXIS2_PLACEMENT_3D('',#34614,#28089,#28090);
#25141=AXIS2_PLACEMENT_3D('',#34616,#28091,#28092);
#25142=AXIS2_PLACEMENT_3D('',#34617,#28093,#28094);
#25143=AXIS2_PLACEMENT_3D('',#34620,#28096,#28097);
#25144=AXIS2_PLACEMENT_3D('',#34621,#28098,#28099);
#25145=AXIS2_PLACEMENT_3D('',#34623,#28100,#28101);
#25146=AXIS2_PLACEMENT_3D('',#34626,#28103,#28104);
#25147=AXIS2_PLACEMENT_3D('',#34627,#28105,#28106);
#25148=AXIS2_PLACEMENT_3D('',#34630,#28108,#28109);
#25149=AXIS2_PLACEMENT_3D('',#34631,#28110,#28111);
#25150=AXIS2_PLACEMENT_3D('',#34634,#28113,#28114);
#25151=AXIS2_PLACEMENT_3D('',#34635,#28115,#28116);
#25152=AXIS2_PLACEMENT_3D('',#34637,#28117,#28118);
#25153=AXIS2_PLACEMENT_3D('',#34638,#28119,#28120);
#25154=AXIS2_PLACEMENT_3D('',#34641,#28122,#28123);
#25155=AXIS2_PLACEMENT_3D('',#34642,#28124,#28125);
#25156=AXIS2_PLACEMENT_3D('',#34644,#28126,#28127);
#25157=AXIS2_PLACEMENT_3D('',#34647,#28129,#28130);
#25158=AXIS2_PLACEMENT_3D('',#34648,#28131,#28132);
#25159=AXIS2_PLACEMENT_3D('',#34651,#28134,#28135);
#25160=AXIS2_PLACEMENT_3D('',#34652,#28136,#28137);
#25161=AXIS2_PLACEMENT_3D('',#34655,#28139,#28140);
#25162=AXIS2_PLACEMENT_3D('',#34656,#28141,#28142);
#25163=AXIS2_PLACEMENT_3D('',#34658,#28143,#28144);
#25164=AXIS2_PLACEMENT_3D('',#34659,#28145,#28146);
#25165=AXIS2_PLACEMENT_3D('',#34662,#28148,#28149);
#25166=AXIS2_PLACEMENT_3D('',#34663,#28150,#28151);
#25167=AXIS2_PLACEMENT_3D('',#34665,#28152,#28153);
#25168=AXIS2_PLACEMENT_3D('',#34668,#28155,#28156);
#25169=AXIS2_PLACEMENT_3D('',#34669,#28157,#28158);
#25170=AXIS2_PLACEMENT_3D('',#34672,#28160,#28161);
#25171=AXIS2_PLACEMENT_3D('',#34673,#28162,#28163);
#25172=AXIS2_PLACEMENT_3D('',#34676,#28165,#28166);
#25173=AXIS2_PLACEMENT_3D('',#34677,#28167,#28168);
#25174=AXIS2_PLACEMENT_3D('',#34679,#28169,#28170);
#25175=AXIS2_PLACEMENT_3D('',#34680,#28171,#28172);
#25176=AXIS2_PLACEMENT_3D('',#34683,#28174,#28175);
#25177=AXIS2_PLACEMENT_3D('',#34684,#28176,#28177);
#25178=AXIS2_PLACEMENT_3D('',#34686,#28178,#28179);
#25179=AXIS2_PLACEMENT_3D('',#34689,#28181,#28182);
#25180=AXIS2_PLACEMENT_3D('',#34690,#28183,#28184);
#25181=AXIS2_PLACEMENT_3D('',#34693,#28186,#28187);
#25182=AXIS2_PLACEMENT_3D('',#34694,#28188,#28189);
#25183=AXIS2_PLACEMENT_3D('',#34697,#28191,#28192);
#25184=AXIS2_PLACEMENT_3D('',#34698,#28193,#28194);
#25185=AXIS2_PLACEMENT_3D('',#34700,#28195,#28196);
#25186=AXIS2_PLACEMENT_3D('',#34701,#28197,#28198);
#25187=AXIS2_PLACEMENT_3D('',#34704,#28200,#28201);
#25188=AXIS2_PLACEMENT_3D('',#34705,#28202,#28203);
#25189=AXIS2_PLACEMENT_3D('',#34707,#28204,#28205);
#25190=AXIS2_PLACEMENT_3D('',#34710,#28207,#28208);
#25191=AXIS2_PLACEMENT_3D('',#34711,#28209,#28210);
#25192=AXIS2_PLACEMENT_3D('',#34714,#28212,#28213);
#25193=AXIS2_PLACEMENT_3D('',#34715,#28214,#28215);
#25194=AXIS2_PLACEMENT_3D('',#34718,#28217,#28218);
#25195=AXIS2_PLACEMENT_3D('',#34719,#28219,#28220);
#25196=AXIS2_PLACEMENT_3D('',#34721,#28221,#28222);
#25197=AXIS2_PLACEMENT_3D('',#34722,#28223,#28224);
#25198=AXIS2_PLACEMENT_3D('',#34725,#28226,#28227);
#25199=AXIS2_PLACEMENT_3D('',#34726,#28228,#28229);
#25200=AXIS2_PLACEMENT_3D('',#34728,#28230,#28231);
#25201=AXIS2_PLACEMENT_3D('',#34731,#28233,#28234);
#25202=AXIS2_PLACEMENT_3D('',#34732,#28235,#28236);
#25203=AXIS2_PLACEMENT_3D('',#34735,#28238,#28239);
#25204=AXIS2_PLACEMENT_3D('',#34736,#28240,#28241);
#25205=AXIS2_PLACEMENT_3D('',#34739,#28243,#28244);
#25206=AXIS2_PLACEMENT_3D('',#34740,#28245,#28246);
#25207=AXIS2_PLACEMENT_3D('',#34742,#28247,#28248);
#25208=AXIS2_PLACEMENT_3D('',#34743,#28249,#28250);
#25209=AXIS2_PLACEMENT_3D('',#34746,#28252,#28253);
#25210=AXIS2_PLACEMENT_3D('',#34747,#28254,#28255);
#25211=AXIS2_PLACEMENT_3D('',#34749,#28256,#28257);
#25212=AXIS2_PLACEMENT_3D('',#34752,#28259,#28260);
#25213=AXIS2_PLACEMENT_3D('',#34753,#28261,#28262);
#25214=AXIS2_PLACEMENT_3D('',#34756,#28264,#28265);
#25215=AXIS2_PLACEMENT_3D('',#34757,#28266,#28267);
#25216=AXIS2_PLACEMENT_3D('',#34760,#28269,#28270);
#25217=AXIS2_PLACEMENT_3D('',#34761,#28271,#28272);
#25218=AXIS2_PLACEMENT_3D('',#34763,#28273,#28274);
#25219=AXIS2_PLACEMENT_3D('',#34764,#28275,#28276);
#25220=AXIS2_PLACEMENT_3D('',#34767,#28278,#28279);
#25221=AXIS2_PLACEMENT_3D('',#34768,#28280,#28281);
#25222=AXIS2_PLACEMENT_3D('',#34770,#28282,#28283);
#25223=AXIS2_PLACEMENT_3D('',#34774,#28285,#28286);
#25224=AXIS2_PLACEMENT_3D('',#34775,#28287,#28288);
#25225=AXIS2_PLACEMENT_3D('',#34776,#28289,#28290);
#25226=AXIS2_PLACEMENT_3D('',#34779,#28291,#28292);
#25227=AXIS2_PLACEMENT_3D('',#34780,#28293,#28294);
#25228=AXIS2_PLACEMENT_3D('',#34782,#28296,#28297);
#25229=AXIS2_PLACEMENT_3D('',#34784,#28298,#28299);
#25230=AXIS2_PLACEMENT_3D('',#34785,#28300,#28301);
#25231=AXIS2_PLACEMENT_3D('',#34788,#28303,#28304);
#25232=AXIS2_PLACEMENT_3D('',#34789,#28305,#28306);
#25233=AXIS2_PLACEMENT_3D('',#34791,#28307,#28308);
#25234=AXIS2_PLACEMENT_3D('',#34792,#28309,#28310);
#25235=AXIS2_PLACEMENT_3D('',#34795,#28311,#28312);
#25236=AXIS2_PLACEMENT_3D('',#34796,#28313,#28314);
#25237=AXIS2_PLACEMENT_3D('',#34799,#28316,#28317);
#25238=AXIS2_PLACEMENT_3D('',#34800,#28318,#28319);
#25239=AXIS2_PLACEMENT_3D('',#34803,#28320,#28321);
#25240=AXIS2_PLACEMENT_3D('',#34804,#28322,#28323);
#25241=AXIS2_PLACEMENT_3D('',#34806,#28325,#28326);
#25242=AXIS2_PLACEMENT_3D('',#34808,#28327,#28328);
#25243=AXIS2_PLACEMENT_3D('',#34809,#28329,#28330);
#25244=AXIS2_PLACEMENT_3D('',#34811,#28331,#28332);
#25245=AXIS2_PLACEMENT_3D('',#34813,#28334,#28335);
#25246=AXIS2_PLACEMENT_3D('',#34818,#28337,#28338);
#25247=AXIS2_PLACEMENT_3D('',#34822,#28340,#28341);
#25248=AXIS2_PLACEMENT_3D('',#34823,#28342,#28343);
#25249=AXIS2_PLACEMENT_3D('',#34826,#28344,#28345);
#25250=AXIS2_PLACEMENT_3D('',#34830,#28347,#28348);
#25251=AXIS2_PLACEMENT_3D('',#34833,#28350,#28351);
#25252=AXIS2_PLACEMENT_3D('',#34838,#28353,#28354);
#25253=AXIS2_PLACEMENT_3D('',#34842,#28356,#28357);
#25254=AXIS2_PLACEMENT_3D('',#34843,#28358,#28359);
#25255=AXIS2_PLACEMENT_3D('',#34846,#28360,#28361);
#25256=AXIS2_PLACEMENT_3D('',#34848,#28362,#28363);
#25257=AXIS2_PLACEMENT_3D('',#34852,#28365,#28366);
#25258=AXIS2_PLACEMENT_3D('',#34858,#28369,#28370);
#25259=AXIS2_PLACEMENT_3D('',#34862,#28372,#28373);
#25260=AXIS2_PLACEMENT_3D('',#34863,#28374,#28375);
#25261=AXIS2_PLACEMENT_3D('',#34866,#28376,#28377);
#25262=AXIS2_PLACEMENT_3D('',#34870,#28379,#28380);
#25263=AXIS2_PLACEMENT_3D('',#34873,#28382,#28383);
#25264=AXIS2_PLACEMENT_3D('',#34878,#28385,#28386);
#25265=AXIS2_PLACEMENT_3D('',#34882,#28388,#28389);
#25266=AXIS2_PLACEMENT_3D('',#34883,#28390,#28391);
#25267=AXIS2_PLACEMENT_3D('',#34886,#28392,#28393);
#25268=AXIS2_PLACEMENT_3D('',#34888,#28394,#28395);
#25269=AXIS2_PLACEMENT_3D('',#34892,#28397,#28398);
#25270=AXIS2_PLACEMENT_3D('',#34898,#28401,#28402);
#25271=AXIS2_PLACEMENT_3D('',#34902,#28404,#28405);
#25272=AXIS2_PLACEMENT_3D('',#34903,#28406,#28407);
#25273=AXIS2_PLACEMENT_3D('',#34906,#28408,#28409);
#25274=AXIS2_PLACEMENT_3D('',#34910,#28411,#28412);
#25275=AXIS2_PLACEMENT_3D('',#34913,#28414,#28415);
#25276=AXIS2_PLACEMENT_3D('',#34918,#28417,#28418);
#25277=AXIS2_PLACEMENT_3D('',#34922,#28420,#28421);
#25278=AXIS2_PLACEMENT_3D('',#34923,#28422,#28423);
#25279=AXIS2_PLACEMENT_3D('',#34926,#28424,#28425);
#25280=AXIS2_PLACEMENT_3D('',#34928,#28426,#28427);
#25281=AXIS2_PLACEMENT_3D('',#34932,#28429,#28430);
#25282=AXIS2_PLACEMENT_3D('',#34938,#28433,#28434);
#25283=AXIS2_PLACEMENT_3D('',#34942,#28436,#28437);
#25284=AXIS2_PLACEMENT_3D('',#34945,#28439,#28440);
#25285=AXIS2_PLACEMENT_3D('',#34950,#28442,#28443);
#25286=AXIS2_PLACEMENT_3D('',#34954,#28445,#28446);
#25287=AXIS2_PLACEMENT_3D('',#34957,#28448,#28449);
#25288=AXIS2_PLACEMENT_3D('',#34962,#28451,#28452);
#25289=AXIS2_PLACEMENT_3D('',#34966,#28454,#28455);
#25290=AXIS2_PLACEMENT_3D('',#34969,#28457,#28458);
#25291=AXIS2_PLACEMENT_3D('',#34974,#28460,#28461);
#25292=AXIS2_PLACEMENT_3D('',#34978,#28463,#28464);
#25293=AXIS2_PLACEMENT_3D('',#34981,#28466,#28467);
#25294=AXIS2_PLACEMENT_3D('',#34986,#28469,#28470);
#25295=AXIS2_PLACEMENT_3D('',#34990,#28472,#28473);
#25296=AXIS2_PLACEMENT_3D('',#34993,#28475,#28476);
#25297=AXIS2_PLACEMENT_3D('',#34998,#28478,#28479);
#25298=AXIS2_PLACEMENT_3D('',#35002,#28481,#28482);
#25299=AXIS2_PLACEMENT_3D('',#35005,#28484,#28485);
#25300=AXIS2_PLACEMENT_3D('',#35010,#28487,#28488);
#25301=AXIS2_PLACEMENT_3D('',#35014,#28490,#28491);
#25302=AXIS2_PLACEMENT_3D('',#35017,#28493,#28494);
#25303=AXIS2_PLACEMENT_3D('',#35022,#28496,#28497);
#25304=AXIS2_PLACEMENT_3D('',#35026,#28499,#28500);
#25305=AXIS2_PLACEMENT_3D('',#35029,#28502,#28503);
#25306=AXIS2_PLACEMENT_3D('',#35034,#28505,#28506);
#25307=AXIS2_PLACEMENT_3D('',#35038,#28508,#28509);
#25308=AXIS2_PLACEMENT_3D('',#35041,#28511,#28512);
#25309=AXIS2_PLACEMENT_3D('',#35046,#28514,#28515);
#25310=AXIS2_PLACEMENT_3D('',#35050,#28517,#28518);
#25311=AXIS2_PLACEMENT_3D('',#35053,#28520,#28521);
#25312=AXIS2_PLACEMENT_3D('',#35058,#28523,#28524);
#25313=AXIS2_PLACEMENT_3D('',#35062,#28526,#28527);
#25314=AXIS2_PLACEMENT_3D('',#35065,#28529,#28530);
#25315=AXIS2_PLACEMENT_3D('',#35070,#28532,#28533);
#25316=AXIS2_PLACEMENT_3D('',#35074,#28535,#28536);
#25317=AXIS2_PLACEMENT_3D('',#35077,#28538,#28539);
#25318=AXIS2_PLACEMENT_3D('',#35082,#28541,#28542);
#25319=AXIS2_PLACEMENT_3D('',#35086,#28544,#28545);
#25320=AXIS2_PLACEMENT_3D('',#35089,#28547,#28548);
#25321=AXIS2_PLACEMENT_3D('',#35094,#28550,#28551);
#25322=AXIS2_PLACEMENT_3D('',#35098,#28553,#28554);
#25323=AXIS2_PLACEMENT_3D('',#35101,#28556,#28557);
#25324=AXIS2_PLACEMENT_3D('',#35106,#28559,#28560);
#25325=AXIS2_PLACEMENT_3D('',#35110,#28562,#28563);
#25326=AXIS2_PLACEMENT_3D('',#35113,#28565,#28566);
#25327=AXIS2_PLACEMENT_3D('',#35118,#28568,#28569);
#25328=AXIS2_PLACEMENT_3D('',#35122,#28571,#28572);
#25329=AXIS2_PLACEMENT_3D('',#35125,#28574,#28575);
#25330=AXIS2_PLACEMENT_3D('',#35130,#28577,#28578);
#25331=AXIS2_PLACEMENT_3D('',#35134,#28580,#28581);
#25332=AXIS2_PLACEMENT_3D('',#35137,#28583,#28584);
#25333=AXIS2_PLACEMENT_3D('',#35142,#28586,#28587);
#25334=AXIS2_PLACEMENT_3D('',#35146,#28589,#28590);
#25335=AXIS2_PLACEMENT_3D('',#35149,#28592,#28593);
#25336=AXIS2_PLACEMENT_3D('',#35151,#28594,#28595);
#25337=AXIS2_PLACEMENT_3D('',#35152,#28596,#28597);
#25338=AXIS2_PLACEMENT_3D('',#35156,#28599,#28600);
#25339=AXIS2_PLACEMENT_3D('',#35158,#28602,#28603);
#25340=AXIS2_PLACEMENT_3D('',#35161,#28604,#28605);
#25341=AXIS2_PLACEMENT_3D('',#35164,#28608,#28609);
#25342=AXIS2_PLACEMENT_3D('',#35168,#28612,#28613);
#25343=AXIS2_PLACEMENT_3D('',#35171,#28614,#28615);
#25344=AXIS2_PLACEMENT_3D('',#35174,#28618,#28619);
#25345=AXIS2_PLACEMENT_3D('',#35176,#28621,#28622);
#25346=AXIS2_PLACEMENT_3D('',#35177,#28623,#28624);
#25347=AXIS2_PLACEMENT_3D('',#35180,#28625,#28626);
#25348=AXIS2_PLACEMENT_3D('',#35183,#28629,#28630);
#25349=AXIS2_PLACEMENT_3D('',#35187,#28633,#28634);
#25350=AXIS2_PLACEMENT_3D('',#35190,#28635,#28636);
#25351=AXIS2_PLACEMENT_3D('',#35193,#28639,#28640);
#25352=AXIS2_PLACEMENT_3D('',#35197,#28643,#28644);
#25353=AXIS2_PLACEMENT_3D('',#35198,#28645,#28646);
#25354=AXIS2_PLACEMENT_3D('',#35200,#28648,#28649);
#25355=AXIS2_PLACEMENT_3D('',#35201,#28650,#28651);
#25356=AXIS2_PLACEMENT_3D('',#35204,#28652,#28653);
#25357=AXIS2_PLACEMENT_3D('',#35207,#28656,#28657);
#25358=AXIS2_PLACEMENT_3D('',#35211,#28660,#28661);
#25359=AXIS2_PLACEMENT_3D('',#35214,#28662,#28663);
#25360=AXIS2_PLACEMENT_3D('',#35217,#28666,#28667);
#25361=AXIS2_PLACEMENT_3D('',#35221,#28670,#28671);
#25362=AXIS2_PLACEMENT_3D('',#35222,#28672,#28673);
#25363=AXIS2_PLACEMENT_3D('',#35224,#28675,#28676);
#25364=AXIS2_PLACEMENT_3D('',#35225,#28677,#28678);
#25365=AXIS2_PLACEMENT_3D('',#35229,#28680,#28681);
#25366=AXIS2_PLACEMENT_3D('',#35231,#28683,#28684);
#25367=AXIS2_PLACEMENT_3D('',#35234,#28685,#28686);
#25368=AXIS2_PLACEMENT_3D('',#35237,#28689,#28690);
#25369=AXIS2_PLACEMENT_3D('',#35241,#28693,#28694);
#25370=AXIS2_PLACEMENT_3D('',#35244,#28695,#28696);
#25371=AXIS2_PLACEMENT_3D('',#35247,#28699,#28700);
#25372=AXIS2_PLACEMENT_3D('',#35251,#28703,#28704);
#25373=AXIS2_PLACEMENT_3D('',#35252,#28705,#28706);
#25374=AXIS2_PLACEMENT_3D('',#35254,#28708,#28709);
#25375=AXIS2_PLACEMENT_3D('',#35255,#28710,#28711);
#25376=AXIS2_PLACEMENT_3D('',#35258,#28712,#28713);
#25377=AXIS2_PLACEMENT_3D('',#35261,#28716,#28717);
#25378=AXIS2_PLACEMENT_3D('',#35265,#28720,#28721);
#25379=AXIS2_PLACEMENT_3D('',#35268,#28722,#28723);
#25380=AXIS2_PLACEMENT_3D('',#35271,#28726,#28727);
#25381=AXIS2_PLACEMENT_3D('',#35275,#28730,#28731);
#25382=AXIS2_PLACEMENT_3D('',#35276,#28732,#28733);
#25383=AXIS2_PLACEMENT_3D('',#35278,#28735,#28736);
#25384=AXIS2_PLACEMENT_3D('',#35279,#28737,#28738);
#25385=AXIS2_PLACEMENT_3D('',#35282,#28739,#28740);
#25386=AXIS2_PLACEMENT_3D('',#35285,#28743,#28744);
#25387=AXIS2_PLACEMENT_3D('',#35289,#28747,#28748);
#25388=AXIS2_PLACEMENT_3D('',#35292,#28749,#28750);
#25389=AXIS2_PLACEMENT_3D('',#35295,#28753,#28754);
#25390=AXIS2_PLACEMENT_3D('',#35299,#28756,#28757);
#25391=AXIS2_PLACEMENT_3D('',#35301,#28758,#28759);
#25392=AXIS2_PLACEMENT_3D('',#35303,#28761,#28762);
#25393=AXIS2_PLACEMENT_3D('',#35305,#28764,#28765);
#25394=AXIS2_PLACEMENT_3D('',#35307,#28767,#28768);
#25395=AXIS2_PLACEMENT_3D('',#35310,#28769,#28770);
#25396=AXIS2_PLACEMENT_3D('',#35313,#28773,#28774);
#25397=AXIS2_PLACEMENT_3D('',#35317,#28777,#28778);
#25398=AXIS2_PLACEMENT_3D('',#35320,#28779,#28780);
#25399=AXIS2_PLACEMENT_3D('',#35323,#28783,#28784);
#25400=AXIS2_PLACEMENT_3D('',#35327,#28787,#28788);
#25401=AXIS2_PLACEMENT_3D('',#35328,#28789,#28790);
#25402=AXIS2_PLACEMENT_3D('',#35330,#28792,#28793);
#25403=AXIS2_PLACEMENT_3D('',#35331,#28794,#28795);
#25404=AXIS2_PLACEMENT_3D('',#35334,#28796,#28797);
#25405=AXIS2_PLACEMENT_3D('',#35337,#28800,#28801);
#25406=AXIS2_PLACEMENT_3D('',#35341,#28804,#28805);
#25407=AXIS2_PLACEMENT_3D('',#35344,#28806,#28807);
#25408=AXIS2_PLACEMENT_3D('',#35347,#28810,#28811);
#25409=AXIS2_PLACEMENT_3D('',#35351,#28814,#28815);
#25410=AXIS2_PLACEMENT_3D('',#35352,#28816,#28817);
#25411=AXIS2_PLACEMENT_3D('',#35354,#28819,#28820);
#25412=AXIS2_PLACEMENT_3D('',#35355,#28821,#28822);
#25413=AXIS2_PLACEMENT_3D('',#35359,#28824,#28825);
#25414=AXIS2_PLACEMENT_3D('',#35361,#28827,#28828);
#25415=AXIS2_PLACEMENT_3D('',#35365,#28830,#28831);
#25416=AXIS2_PLACEMENT_3D('',#35368,#28833,#28834);
#25417=AXIS2_PLACEMENT_3D('',#35369,#28835,#28836);
#25418=AXIS2_PLACEMENT_3D('',#35371,#28838,#28839);
#25419=AXIS2_PLACEMENT_3D('',#35373,#28841,#28842);
#25420=AXIS2_PLACEMENT_3D('',#35375,#28844,#28845);
#25421=AXIS2_PLACEMENT_3D('',#35378,#28846,#28847);
#25422=AXIS2_PLACEMENT_3D('',#35381,#28850,#28851);
#25423=AXIS2_PLACEMENT_3D('',#35385,#28854,#28855);
#25424=AXIS2_PLACEMENT_3D('',#35388,#28856,#28857);
#25425=AXIS2_PLACEMENT_3D('',#35391,#28860,#28861);
#25426=AXIS2_PLACEMENT_3D('',#35395,#28864,#28865);
#25427=AXIS2_PLACEMENT_3D('',#35396,#28866,#28867);
#25428=AXIS2_PLACEMENT_3D('',#35398,#28869,#28870);
#25429=AXIS2_PLACEMENT_3D('',#35399,#28871,#28872);
#25430=AXIS2_PLACEMENT_3D('',#35402,#28873,#28874);
#25431=AXIS2_PLACEMENT_3D('',#35405,#28877,#28878);
#25432=AXIS2_PLACEMENT_3D('',#35409,#28881,#28882);
#25433=AXIS2_PLACEMENT_3D('',#35412,#28883,#28884);
#25434=AXIS2_PLACEMENT_3D('',#35415,#28887,#28888);
#25435=AXIS2_PLACEMENT_3D('',#35419,#28891,#28892);
#25436=AXIS2_PLACEMENT_3D('',#35420,#28893,#28894);
#25437=AXIS2_PLACEMENT_3D('',#35422,#28896,#28897);
#25438=AXIS2_PLACEMENT_3D('',#35423,#28898,#28899);
#25439=AXIS2_PLACEMENT_3D('',#35426,#28900,#28901);
#25440=AXIS2_PLACEMENT_3D('',#35429,#28904,#28905);
#25441=AXIS2_PLACEMENT_3D('',#35433,#28908,#28909);
#25442=AXIS2_PLACEMENT_3D('',#35436,#28910,#28911);
#25443=AXIS2_PLACEMENT_3D('',#35439,#28914,#28915);
#25444=AXIS2_PLACEMENT_3D('',#35443,#28917,#28918);
#25445=AXIS2_PLACEMENT_3D('',#35445,#28919,#28920);
#25446=AXIS2_PLACEMENT_3D('',#35447,#28922,#28923);
#25447=AXIS2_PLACEMENT_3D('',#35449,#28925,#28926);
#25448=AXIS2_PLACEMENT_3D('',#35451,#28928,#28929);
#25449=AXIS2_PLACEMENT_3D('',#35454,#28930,#28931);
#25450=AXIS2_PLACEMENT_3D('',#35457,#28934,#28935);
#25451=AXIS2_PLACEMENT_3D('',#35461,#28938,#28939);
#25452=AXIS2_PLACEMENT_3D('',#35464,#28940,#28941);
#25453=AXIS2_PLACEMENT_3D('',#35467,#28944,#28945);
#25454=AXIS2_PLACEMENT_3D('',#35471,#28948,#28949);
#25455=AXIS2_PLACEMENT_3D('',#35472,#28950,#28951);
#25456=AXIS2_PLACEMENT_3D('',#35474,#28953,#28954);
#25457=AXIS2_PLACEMENT_3D('',#35475,#28955,#28956);
#25458=AXIS2_PLACEMENT_3D('',#35478,#28957,#28958);
#25459=AXIS2_PLACEMENT_3D('',#35481,#28961,#28962);
#25460=AXIS2_PLACEMENT_3D('',#35485,#28965,#28966);
#25461=AXIS2_PLACEMENT_3D('',#35488,#28967,#28968);
#25462=AXIS2_PLACEMENT_3D('',#35491,#28971,#28972);
#25463=AXIS2_PLACEMENT_3D('',#35495,#28975,#28976);
#25464=AXIS2_PLACEMENT_3D('',#35496,#28977,#28978);
#25465=AXIS2_PLACEMENT_3D('',#35498,#28980,#28981);
#25466=AXIS2_PLACEMENT_3D('',#35499,#28982,#28983);
#25467=AXIS2_PLACEMENT_3D('',#35502,#28984,#28985);
#25468=AXIS2_PLACEMENT_3D('',#35505,#28988,#28989);
#25469=AXIS2_PLACEMENT_3D('',#35509,#28992,#28993);
#25470=AXIS2_PLACEMENT_3D('',#35512,#28994,#28995);
#25471=AXIS2_PLACEMENT_3D('',#35515,#28998,#28999);
#25472=AXIS2_PLACEMENT_3D('',#35519,#29002,#29003);
#25473=AXIS2_PLACEMENT_3D('',#35520,#29004,#29005);
#25474=AXIS2_PLACEMENT_3D('',#35522,#29007,#29008);
#25475=AXIS2_PLACEMENT_3D('',#35523,#29009,#29010);
#25476=AXIS2_PLACEMENT_3D('',#35527,#29012,#29013);
#25477=AXIS2_PLACEMENT_3D('',#35529,#29015,#29016);
#25478=AXIS2_PLACEMENT_3D('',#35532,#29017,#29018);
#25479=AXIS2_PLACEMENT_3D('',#35535,#29021,#29022);
#25480=AXIS2_PLACEMENT_3D('',#35539,#29025,#29026);
#25481=AXIS2_PLACEMENT_3D('',#35542,#29027,#29028);
#25482=AXIS2_PLACEMENT_3D('',#35545,#29031,#29032);
#25483=AXIS2_PLACEMENT_3D('',#35549,#29035,#29036);
#25484=AXIS2_PLACEMENT_3D('',#35550,#29037,#29038);
#25485=AXIS2_PLACEMENT_3D('',#35552,#29040,#29041);
#25486=AXIS2_PLACEMENT_3D('',#35553,#29042,#29043);
#25487=AXIS2_PLACEMENT_3D('',#35556,#29044,#29045);
#25488=AXIS2_PLACEMENT_3D('',#35559,#29048,#29049);
#25489=AXIS2_PLACEMENT_3D('',#35563,#29052,#29053);
#25490=AXIS2_PLACEMENT_3D('',#35566,#29054,#29055);
#25491=AXIS2_PLACEMENT_3D('',#35569,#29058,#29059);
#25492=AXIS2_PLACEMENT_3D('',#35573,#29062,#29063);
#25493=AXIS2_PLACEMENT_3D('',#35574,#29064,#29065);
#25494=AXIS2_PLACEMENT_3D('',#35576,#29067,#29068);
#25495=AXIS2_PLACEMENT_3D('',#35577,#29069,#29070);
#25496=AXIS2_PLACEMENT_3D('',#35581,#29072,#29073);
#25497=AXIS2_PLACEMENT_3D('',#35583,#29075,#29076);
#25498=AXIS2_PLACEMENT_3D('',#35587,#29078,#29079);
#25499=AXIS2_PLACEMENT_3D('',#35590,#29081,#29082);
#25500=AXIS2_PLACEMENT_3D('',#35591,#29083,#29084);
#25501=AXIS2_PLACEMENT_3D('',#35593,#29086,#29087);
#25502=AXIS2_PLACEMENT_3D('',#35595,#29089,#29090);
#25503=AXIS2_PLACEMENT_3D('',#35597,#29092,#29093);
#25504=AXIS2_PLACEMENT_3D('',#35600,#29094,#29095);
#25505=AXIS2_PLACEMENT_3D('',#35603,#29098,#29099);
#25506=AXIS2_PLACEMENT_3D('',#35607,#29102,#29103);
#25507=AXIS2_PLACEMENT_3D('',#35610,#29104,#29105);
#25508=AXIS2_PLACEMENT_3D('',#35613,#29108,#29109);
#25509=AXIS2_PLACEMENT_3D('',#35617,#29112,#29113);
#25510=AXIS2_PLACEMENT_3D('',#35618,#29114,#29115);
#25511=AXIS2_PLACEMENT_3D('',#35620,#29117,#29118);
#25512=AXIS2_PLACEMENT_3D('',#35621,#29119,#29120);
#25513=AXIS2_PLACEMENT_3D('',#35624,#29121,#29122);
#25514=AXIS2_PLACEMENT_3D('',#35627,#29125,#29126);
#25515=AXIS2_PLACEMENT_3D('',#35631,#29129,#29130);
#25516=AXIS2_PLACEMENT_3D('',#35634,#29131,#29132);
#25517=AXIS2_PLACEMENT_3D('',#35637,#29135,#29136);
#25518=AXIS2_PLACEMENT_3D('',#35641,#29139,#29140);
#25519=AXIS2_PLACEMENT_3D('',#35642,#29141,#29142);
#25520=AXIS2_PLACEMENT_3D('',#35644,#29144,#29145);
#25521=AXIS2_PLACEMENT_3D('',#35645,#29146,#29147);
#25522=AXIS2_PLACEMENT_3D('',#35649,#29149,#29150);
#25523=AXIS2_PLACEMENT_3D('',#35651,#29152,#29153);
#25524=AXIS2_PLACEMENT_3D('',#35654,#29154,#29155);
#25525=AXIS2_PLACEMENT_3D('',#35657,#29158,#29159);
#25526=AXIS2_PLACEMENT_3D('',#35661,#29162,#29163);
#25527=AXIS2_PLACEMENT_3D('',#35662,#29164,#29165);
#25528=AXIS2_PLACEMENT_3D('',#35664,#29167,#29168);
#25529=AXIS2_PLACEMENT_3D('',#35667,#29169,#29170);
#25530=AXIS2_PLACEMENT_3D('',#35670,#29173,#29174);
#25531=AXIS2_PLACEMENT_3D('',#35674,#29177,#29178);
#25532=AXIS2_PLACEMENT_3D('',#35677,#29179,#29180);
#25533=AXIS2_PLACEMENT_3D('',#35680,#29183,#29184);
#25534=AXIS2_PLACEMENT_3D('',#35684,#29187,#29188);
#25535=AXIS2_PLACEMENT_3D('',#35685,#29189,#29190);
#25536=AXIS2_PLACEMENT_3D('',#35687,#29192,#29193);
#25537=AXIS2_PLACEMENT_3D('',#35688,#29194,#29195);
#25538=AXIS2_PLACEMENT_3D('',#35691,#29196,#29197);
#25539=AXIS2_PLACEMENT_3D('',#35694,#29200,#29201);
#25540=AXIS2_PLACEMENT_3D('',#35698,#29204,#29205);
#25541=AXIS2_PLACEMENT_3D('',#35701,#29206,#29207);
#25542=AXIS2_PLACEMENT_3D('',#35704,#29210,#29211);
#25543=AXIS2_PLACEMENT_3D('',#35708,#29214,#29215);
#25544=AXIS2_PLACEMENT_3D('',#35709,#29216,#29217);
#25545=AXIS2_PLACEMENT_3D('',#35711,#29219,#29220);
#25546=AXIS2_PLACEMENT_3D('',#35712,#29221,#29222);
#25547=AXIS2_PLACEMENT_3D('',#35715,#29223,#29224);
#25548=AXIS2_PLACEMENT_3D('',#35718,#29227,#29228);
#25549=AXIS2_PLACEMENT_3D('',#35722,#29231,#29232);
#25550=AXIS2_PLACEMENT_3D('',#35725,#29233,#29234);
#25551=AXIS2_PLACEMENT_3D('',#35728,#29237,#29238);
#25552=AXIS2_PLACEMENT_3D('',#35732,#29241,#29242);
#25553=AXIS2_PLACEMENT_3D('',#35733,#29243,#29244);
#25554=AXIS2_PLACEMENT_3D('',#35735,#29246,#29247);
#25555=AXIS2_PLACEMENT_3D('',#35736,#29248,#29249);
#25556=AXIS2_PLACEMENT_3D('',#35739,#29250,#29251);
#25557=AXIS2_PLACEMENT_3D('',#35742,#29254,#29255);
#25558=AXIS2_PLACEMENT_3D('',#35746,#29258,#29259);
#25559=AXIS2_PLACEMENT_3D('',#35747,#29260,#29261);
#25560=AXIS2_PLACEMENT_3D('',#35749,#29263,#29264);
#25561=AXIS2_PLACEMENT_3D('',#35752,#29265,#29266);
#25562=AXIS2_PLACEMENT_3D('',#35755,#29269,#29270);
#25563=AXIS2_PLACEMENT_3D('',#35759,#29273,#29274);
#25564=AXIS2_PLACEMENT_3D('',#35762,#29275,#29276);
#25565=AXIS2_PLACEMENT_3D('',#35765,#29279,#29280);
#25566=AXIS2_PLACEMENT_3D('',#35767,#29282,#29283);
#25567=AXIS2_PLACEMENT_3D('',#35768,#29284,#29285);
#25568=AXIS2_PLACEMENT_3D('',#35771,#29286,#29287);
#25569=AXIS2_PLACEMENT_3D('',#35774,#29290,#29291);
#25570=AXIS2_PLACEMENT_3D('',#35778,#29294,#29295);
#25571=AXIS2_PLACEMENT_3D('',#35779,#29296,#29297);
#25572=AXIS2_PLACEMENT_3D('',#35781,#29299,#29300);
#25573=AXIS2_PLACEMENT_3D('',#35784,#29301,#29302);
#25574=AXIS2_PLACEMENT_3D('',#35787,#29305,#29306);
#25575=AXIS2_PLACEMENT_3D('',#35789,#29308,#29309);
#25576=AXIS2_PLACEMENT_3D('',#35790,#29310,#29311);
#25577=AXIS2_PLACEMENT_3D('',#35793,#29312,#29313);
#25578=AXIS2_PLACEMENT_3D('',#35796,#29316,#29317);
#25579=AXIS2_PLACEMENT_3D('',#35800,#29320,#29321);
#25580=AXIS2_PLACEMENT_3D('',#35801,#29322,#29323);
#25581=AXIS2_PLACEMENT_3D('',#35803,#29325,#29326);
#25582=AXIS2_PLACEMENT_3D('',#35806,#29327,#29328);
#25583=AXIS2_PLACEMENT_3D('',#35809,#29331,#29332);
#25584=AXIS2_PLACEMENT_3D('',#35811,#29334,#29335);
#25585=AXIS2_PLACEMENT_3D('',#35812,#29336,#29337);
#25586=AXIS2_PLACEMENT_3D('',#35813,#29338,#29339);
#25587=AXIS2_PLACEMENT_3D('',#35814,#29340,#29341);
#25588=AXIS2_PLACEMENT_3D('',#35815,#29342,#29343);
#25589=AXIS2_PLACEMENT_3D('',#35816,#29344,#29345);
#25590=AXIS2_PLACEMENT_3D('',#35817,#29346,#29347);
#25591=AXIS2_PLACEMENT_3D('',#35819,#29349,#29350);
#25592=AXIS2_PLACEMENT_3D('',#35820,#29351,#29352);
#25593=AXIS2_PLACEMENT_3D('',#35821,#29353,#29354);
#25594=AXIS2_PLACEMENT_3D('',#35822,#29355,#29356);
#25595=AXIS2_PLACEMENT_3D('',#35824,#29358,#29359);
#25596=AXIS2_PLACEMENT_3D('',#35825,#29360,#29361);
#25597=AXIS2_PLACEMENT_3D('',#35826,#29362,#29363);
#25598=AXIS2_PLACEMENT_3D('',#35827,#29364,#29365);
#25599=AXIS2_PLACEMENT_3D('',#35828,#29366,#29367);
#25600=AXIS2_PLACEMENT_3D('',#35829,#29368,#29369);
#25601=AXIS2_PLACEMENT_3D('',#35830,#29370,#29371);
#25602=AXIS2_PLACEMENT_3D('',#35831,#29372,#29373);
#25603=AXIS2_PLACEMENT_3D('',#35832,#29374,#29375);
#25604=AXIS2_PLACEMENT_3D('',#35833,#29376,#29377);
#25605=AXIS2_PLACEMENT_3D('',#35834,#29378,#29379);
#25606=AXIS2_PLACEMENT_3D('',#35835,#29380,#29381);
#25607=AXIS2_PLACEMENT_3D('',#35836,#29382,#29383);
#25608=AXIS2_PLACEMENT_3D('',#35837,#29384,#29385);
#25609=AXIS2_PLACEMENT_3D('',#35838,#29386,#29387);
#25610=AXIS2_PLACEMENT_3D('',#35839,#29388,#29389);
#25611=AXIS2_PLACEMENT_3D('',#35840,#29390,#29391);
#25612=AXIS2_PLACEMENT_3D('',#35841,#29392,#29393);
#25613=AXIS2_PLACEMENT_3D('',#35842,#29394,#29395);
#25614=AXIS2_PLACEMENT_3D('',#35843,#29396,#29397);
#25615=AXIS2_PLACEMENT_3D('',#35844,#29398,#29399);
#25616=AXIS2_PLACEMENT_3D('',#35845,#29400,#29401);
#25617=AXIS2_PLACEMENT_3D('',#35846,#29402,#29403);
#25618=AXIS2_PLACEMENT_3D('',#35847,#29404,#29405);
#25619=AXIS2_PLACEMENT_3D('',#35848,#29406,#29407);
#25620=AXIS2_PLACEMENT_3D('',#35849,#29408,#29409);
#25621=AXIS2_PLACEMENT_3D('',#35850,#29410,#29411);
#25622=AXIS2_PLACEMENT_3D('',#35851,#29412,#29413);
#25623=AXIS2_PLACEMENT_3D('',#35852,#29414,#29415);
#25624=AXIS2_PLACEMENT_3D('',#35853,#29416,#29417);
#25625=AXIS2_PLACEMENT_3D('',#35854,#29418,#29419);
#25626=AXIS2_PLACEMENT_3D('',#35857,#29421,#29422);
#25627=AXIS2_PLACEMENT_3D('',#35858,#29423,#29424);
#25628=AXIS2_PLACEMENT_3D('',#35860,#29425,#29426);
#25629=AXIS2_PLACEMENT_3D('',#35861,#29427,#29428);
#25630=AXIS2_PLACEMENT_3D('',#35863,#29430,#29431);
#25631=AXIS2_PLACEMENT_3D('',#35865,#29433,#29434);
#25632=AXIS2_PLACEMENT_3D('',#35866,#29435,#29436);
#25633=AXIS2_PLACEMENT_3D('',#35868,#29437,#29438);
#25634=AXIS2_PLACEMENT_3D('',#35872,#29440,#29441);
#25635=AXIS2_PLACEMENT_3D('',#35873,#29442,#29443);
#25636=AXIS2_PLACEMENT_3D('',#35874,#29444,#29445);
#25637=AXIS2_PLACEMENT_3D('',#35878,#29447,#29448);
#25638=AXIS2_PLACEMENT_3D('',#35879,#29449,#29450);
#25639=AXIS2_PLACEMENT_3D('',#35880,#29451,#29452);
#25640=AXIS2_PLACEMENT_3D('',#35882,#29453,#29454);
#25641=AXIS2_PLACEMENT_3D('',#35883,#29455,#29456);
#25642=AXIS2_PLACEMENT_3D('',#35886,#29458,#29459);
#25643=AXIS2_PLACEMENT_3D('',#35887,#29460,#29461);
#25644=AXIS2_PLACEMENT_3D('',#35889,#29462,#29463);
#25645=AXIS2_PLACEMENT_3D('',#35890,#29464,#29465);
#25646=AXIS2_PLACEMENT_3D('',#35892,#29466,#29467);
#25647=AXIS2_PLACEMENT_3D('',#35895,#29469,#29470);
#25648=AXIS2_PLACEMENT_3D('',#35896,#29471,#29472);
#25649=AXIS2_PLACEMENT_3D('',#35898,#29473,#29474);
#25650=AXIS2_PLACEMENT_3D('',#35900,#29476,#29477);
#25651=AXIS2_PLACEMENT_3D('',#35902,#29478,#29479);
#25652=AXIS2_PLACEMENT_3D('',#35903,#29480,#29481);
#25653=AXIS2_PLACEMENT_3D('',#35907,#29483,#29484);
#25654=AXIS2_PLACEMENT_3D('',#35908,#29485,#29486);
#25655=AXIS2_PLACEMENT_3D('',#35909,#29487,#29488);
#25656=AXIS2_PLACEMENT_3D('',#35913,#29490,#29491);
#25657=AXIS2_PLACEMENT_3D('',#35914,#29492,#29493);
#25658=AXIS2_PLACEMENT_3D('',#35915,#29494,#29495);
#25659=AXIS2_PLACEMENT_3D('',#35917,#29496,#29497);
#25660=AXIS2_PLACEMENT_3D('',#35919,#29499,#29500);
#25661=AXIS2_PLACEMENT_3D('',#35921,#29501,#29502);
#25662=AXIS2_PLACEMENT_3D('',#35923,#29504,#29505);
#25663=AXIS2_PLACEMENT_3D('',#35926,#29507,#29508);
#25664=AXIS2_PLACEMENT_3D('',#35927,#29509,#29510);
#25665=AXIS2_PLACEMENT_3D('',#35929,#29511,#29512);
#25666=AXIS2_PLACEMENT_3D('',#35930,#29513,#29514);
#25667=AXIS2_PLACEMENT_3D('',#35933,#29515,#29516);
#25668=AXIS2_PLACEMENT_3D('',#35934,#29517,#29518);
#25669=AXIS2_PLACEMENT_3D('',#35936,#29520,#29521);
#25670=AXIS2_PLACEMENT_3D('',#35938,#29523,#29524);
#25671=AXIS2_PLACEMENT_3D('',#35940,#29525,#29526);
#25672=AXIS2_PLACEMENT_3D('',#35941,#29527,#29528);
#25673=AXIS2_PLACEMENT_3D('',#35942,#29529,#29530);
#25674=AXIS2_PLACEMENT_3D('',#35945,#29532,#29533);
#25675=AXIS2_PLACEMENT_3D('',#35946,#29534,#29535);
#25676=AXIS2_PLACEMENT_3D('',#35948,#29536,#29537);
#25677=AXIS2_PLACEMENT_3D('',#35949,#29538,#29539);
#25678=AXIS2_PLACEMENT_3D('',#35950,#29540,#29541);
#25679=AXIS2_PLACEMENT_3D('',#35953,#29543,#29544);
#25680=AXIS2_PLACEMENT_3D('',#35954,#29545,#29546);
#25681=AXIS2_PLACEMENT_3D('',#35956,#29548,#29549);
#25682=AXIS2_PLACEMENT_3D('',#35957,#29550,#29551);
#25683=AXIS2_PLACEMENT_3D('',#35959,#29552,#29553);
#25684=AXIS2_PLACEMENT_3D('',#35963,#29555,#29556);
#25685=AXIS2_PLACEMENT_3D('',#35964,#29557,#29558);
#25686=AXIS2_PLACEMENT_3D('',#35965,#29559,#29560);
#25687=AXIS2_PLACEMENT_3D('',#35967,#29561,#29562);
#25688=AXIS2_PLACEMENT_3D('',#35969,#29563,#29564);
#25689=AXIS2_PLACEMENT_3D('',#35971,#29565,#29566);
#25690=AXIS2_PLACEMENT_3D('',#35972,#29567,#29568);
#25691=AXIS2_PLACEMENT_3D('',#35974,#29569,#29570);
#25692=AXIS2_PLACEMENT_3D('',#35976,#29572,#29573);
#25693=AXIS2_PLACEMENT_3D('',#35978,#29574,#29575);
#25694=AXIS2_PLACEMENT_3D('',#35980,#29577,#29578);
#25695=AXIS2_PLACEMENT_3D('',#35982,#29579,#29580);
#25696=AXIS2_PLACEMENT_3D('',#35984,#29582,#29583);
#25697=AXIS2_PLACEMENT_3D('',#35988,#29585,#29586);
#25698=AXIS2_PLACEMENT_3D('',#35989,#29587,#29588);
#25699=AXIS2_PLACEMENT_3D('',#35990,#29589,#29590);
#25700=AXIS2_PLACEMENT_3D('',#35993,#29591,#29592);
#25701=AXIS2_PLACEMENT_3D('',#35994,#29593,#29594);
#25702=AXIS2_PLACEMENT_3D('',#35996,#29596,#29597);
#25703=AXIS2_PLACEMENT_3D('',#35998,#29598,#29599);
#25704=AXIS2_PLACEMENT_3D('',#36000,#29601,#29602);
#25705=AXIS2_PLACEMENT_3D('',#36002,#29603,#29604);
#25706=AXIS2_PLACEMENT_3D('',#36004,#29606,#29607);
#25707=AXIS2_PLACEMENT_3D('',#36006,#29608,#29609);
#25708=AXIS2_PLACEMENT_3D('',#36010,#29611,#29612);
#25709=AXIS2_PLACEMENT_3D('',#36011,#29613,#29614);
#25710=AXIS2_PLACEMENT_3D('',#36012,#29615,#29616);
#25711=AXIS2_PLACEMENT_3D('',#36015,#29617,#29618);
#25712=AXIS2_PLACEMENT_3D('',#36016,#29619,#29620);
#25713=AXIS2_PLACEMENT_3D('',#36018,#29622,#29623);
#25714=AXIS2_PLACEMENT_3D('',#36019,#29624,#29625);
#25715=AXIS2_PLACEMENT_3D('',#36023,#29627,#29628);
#25716=AXIS2_PLACEMENT_3D('',#36036,#29629,#29630);
#25717=AXIS2_PLACEMENT_3D('',#36048,#29631,#29632);
#25718=AXIS2_PLACEMENT_3D('',#36049,#29633,#29634);
#25719=AXIS2_PLACEMENT_3D('',#36051,#29635,#29636);
#25720=AXIS2_PLACEMENT_3D('',#36055,#29638,#29639);
#25721=AXIS2_PLACEMENT_3D('',#36056,#29640,#29641);
#25722=AXIS2_PLACEMENT_3D('',#36057,#29642,#29643);
#25723=AXIS2_PLACEMENT_3D('',#36058,#29644,#29645);
#25724=AXIS2_PLACEMENT_3D('',#36060,#29646,#29647);
#25725=AXIS2_PLACEMENT_3D('',#36062,#29649,#29650);
#25726=AXIS2_PLACEMENT_3D('',#36064,#29651,#29652);
#25727=AXIS2_PLACEMENT_3D('',#36068,#29654,#29655);
#25728=AXIS2_PLACEMENT_3D('',#36069,#29656,#29657);
#25729=AXIS2_PLACEMENT_3D('',#36070,#29658,#29659);
#25730=AXIS2_PLACEMENT_3D('',#36071,#29660,#29661);
#25731=AXIS2_PLACEMENT_3D('',#36073,#29662,#29663);
#25732=AXIS2_PLACEMENT_3D('',#36075,#29665,#29666);
#25733=AXIS2_PLACEMENT_3D('',#36078,#29668,#29669);
#25734=AXIS2_PLACEMENT_3D('',#36079,#29670,#29671);
#25735=AXIS2_PLACEMENT_3D('',#36082,#29673,#29674);
#25736=AXIS2_PLACEMENT_3D('',#36083,#29675,#29676);
#25737=AXIS2_PLACEMENT_3D('',#36086,#29678,#29679);
#25738=AXIS2_PLACEMENT_3D('',#36087,#29680,#29681);
#25739=AXIS2_PLACEMENT_3D('',#36088,#29682,#29683);
#25740=AXIS2_PLACEMENT_3D('',#36091,#29685,#29686);
#25741=AXIS2_PLACEMENT_3D('',#36092,#29687,#29688);
#25742=AXIS2_PLACEMENT_3D('',#36095,#29690,#29691);
#25743=AXIS2_PLACEMENT_3D('',#36096,#29692,#29693);
#25744=AXIS2_PLACEMENT_3D('',#36099,#29695,#29696);
#25745=AXIS2_PLACEMENT_3D('',#36100,#29697,#29698);
#25746=AXIS2_PLACEMENT_3D('',#36101,#29699,#29700);
#25747=AXIS2_PLACEMENT_3D('',#36104,#29702,#29703);
#25748=AXIS2_PLACEMENT_3D('',#36105,#29704,#29705);
#25749=AXIS2_PLACEMENT_3D('',#36106,#29706,#29707);
#25750=AXIS2_PLACEMENT_3D('',#36107,#29708,#29709);
#25751=AXIS2_PLACEMENT_3D('',#36109,#29710,#29711);
#25752=AXIS2_PLACEMENT_3D('',#36112,#29713,#29714);
#25753=AXIS2_PLACEMENT_3D('',#36113,#29715,#29716);
#25754=AXIS2_PLACEMENT_3D('',#36115,#29717,#29718);
#25755=AXIS2_PLACEMENT_3D('',#36118,#29720,#29721);
#25756=AXIS2_PLACEMENT_3D('',#36119,#29722,#29723);
#25757=AXIS2_PLACEMENT_3D('',#36121,#29724,#29725);
#25758=AXIS2_PLACEMENT_3D('',#36124,#29727,#29728);
#25759=AXIS2_PLACEMENT_3D('',#36125,#29729,#29730);
#25760=AXIS2_PLACEMENT_3D('',#36128,#29732,#29733);
#25761=AXIS2_PLACEMENT_3D('',#36129,#29734,#29735);
#25762=AXIS2_PLACEMENT_3D('',#36131,#29736,#29737);
#25763=AXIS2_PLACEMENT_3D('',#36134,#29739,#29740);
#25764=AXIS2_PLACEMENT_3D('',#36135,#29741,#29742);
#25765=AXIS2_PLACEMENT_3D('',#36137,#29743,#29744);
#25766=AXIS2_PLACEMENT_3D('',#36140,#29746,#29747);
#25767=AXIS2_PLACEMENT_3D('',#36141,#29748,#29749);
#25768=AXIS2_PLACEMENT_3D('',#36143,#29750,#29751);
#25769=AXIS2_PLACEMENT_3D('',#36146,#29753,#29754);
#25770=AXIS2_PLACEMENT_3D('',#36147,#29755,#29756);
#25771=AXIS2_PLACEMENT_3D('',#36149,#29757,#29758);
#25772=AXIS2_PLACEMENT_3D('',#36152,#29760,#29761);
#25773=AXIS2_PLACEMENT_3D('',#36153,#29762,#29763);
#25774=AXIS2_PLACEMENT_3D('',#36155,#29764,#29765);
#25775=AXIS2_PLACEMENT_3D('',#36158,#29767,#29768);
#25776=AXIS2_PLACEMENT_3D('',#36159,#29769,#29770);
#25777=AXIS2_PLACEMENT_3D('',#36161,#29771,#29772);
#25778=AXIS2_PLACEMENT_3D('',#36164,#29774,#29775);
#25779=AXIS2_PLACEMENT_3D('',#36165,#29776,#29777);
#25780=AXIS2_PLACEMENT_3D('',#36167,#29778,#29779);
#25781=AXIS2_PLACEMENT_3D('',#36171,#29781,#29782);
#25782=AXIS2_PLACEMENT_3D('',#36172,#29783,#29784);
#25783=AXIS2_PLACEMENT_3D('',#36173,#29785,#29786);
#25784=AXIS2_PLACEMENT_3D('',#36176,#29787,#29788);
#25785=AXIS2_PLACEMENT_3D('',#36177,#29789,#29790);
#25786=AXIS2_PLACEMENT_3D('',#36179,#29792,#29793);
#25787=AXIS2_PLACEMENT_3D('',#36181,#29794,#29795);
#25788=AXIS2_PLACEMENT_3D('',#36182,#29796,#29797);
#25789=AXIS2_PLACEMENT_3D('',#36185,#29799,#29800);
#25790=AXIS2_PLACEMENT_3D('',#36186,#29801,#29802);
#25791=AXIS2_PLACEMENT_3D('',#36188,#29803,#29804);
#25792=AXIS2_PLACEMENT_3D('',#36189,#29805,#29806);
#25793=AXIS2_PLACEMENT_3D('',#36193,#29808,#29809);
#25794=AXIS2_PLACEMENT_3D('',#36194,#29810,#29811);
#25795=AXIS2_PLACEMENT_3D('',#36195,#29812,#29813);
#25796=AXIS2_PLACEMENT_3D('',#36199,#29815,#29816);
#25797=AXIS2_PLACEMENT_3D('',#36200,#29817,#29818);
#25798=AXIS2_PLACEMENT_3D('',#36201,#29819,#29820);
#25799=AXIS2_PLACEMENT_3D('',#36203,#29822,#29823);
#25800=AXIS2_PLACEMENT_3D('',#36204,#29824,#29825);
#25801=AXIS2_PLACEMENT_3D('',#36208,#29827,#29828);
#25802=AXIS2_PLACEMENT_3D('',#36209,#29829,#29830);
#25803=AXIS2_PLACEMENT_3D('',#36212,#29832,#29833);
#25804=AXIS2_PLACEMENT_3D('',#36213,#29834,#29835);
#25805=AXIS2_PLACEMENT_3D('',#36217,#29837,#29838);
#25806=AXIS2_PLACEMENT_3D('',#36218,#29839,#29840);
#25807=AXIS2_PLACEMENT_3D('',#36221,#29842,#29843);
#25808=AXIS2_PLACEMENT_3D('',#36222,#29844,#29845);
#25809=AXIS2_PLACEMENT_3D('',#36224,#29846,#29847);
#25810=AXIS2_PLACEMENT_3D('',#36227,#29849,#29850);
#25811=AXIS2_PLACEMENT_3D('',#36228,#29851,#29852);
#25812=AXIS2_PLACEMENT_3D('',#36229,#29853,#29854);
#25813=AXIS2_PLACEMENT_3D('',#36231,#29855,#29856);
#25814=AXIS2_PLACEMENT_3D('',#36232,#29857,#29858);
#25815=AXIS2_PLACEMENT_3D('',#36234,#29859,#29860);
#25816=AXIS2_PLACEMENT_3D('',#36236,#29862,#29863);
#25817=AXIS2_PLACEMENT_3D('',#36238,#29864,#29865);
#25818=AXIS2_PLACEMENT_3D('',#36240,#29867,#29868);
#25819=AXIS2_PLACEMENT_3D('',#36242,#29869,#29870);
#25820=AXIS2_PLACEMENT_3D('',#36245,#29872,#29873);
#25821=AXIS2_PLACEMENT_3D('',#36246,#29874,#29875);
#25822=AXIS2_PLACEMENT_3D('',#36248,#29876,#29877);
#25823=AXIS2_PLACEMENT_3D('',#36249,#29878,#29879);
#25824=AXIS2_PLACEMENT_3D('',#36251,#29880,#29881);
#25825=AXIS2_PLACEMENT_3D('',#36252,#29882,#29883);
#25826=AXIS2_PLACEMENT_3D('',#36254,#29884,#29885);
#25827=AXIS2_PLACEMENT_3D('',#36256,#29887,#29888);
#25828=AXIS2_PLACEMENT_3D('',#36258,#29889,#29890);
#25829=AXIS2_PLACEMENT_3D('',#36259,#29891,#29892);
#25830=AXIS2_PLACEMENT_3D('',#36261,#29893,#29894);
#25831=AXIS2_PLACEMENT_3D('',#36263,#29896,#29897);
#25832=AXIS2_PLACEMENT_3D('',#36265,#29899,#29900);
#25833=AXIS2_PLACEMENT_3D('',#36267,#29901,#29902);
#25834=AXIS2_PLACEMENT_3D('',#36269,#29904,#29905);
#25835=AXIS2_PLACEMENT_3D('',#36271,#29906,#29907);
#25836=AXIS2_PLACEMENT_3D('',#36272,#29908,#29909);
#25837=AXIS2_PLACEMENT_3D('',#36274,#29910,#29911);
#25838=AXIS2_PLACEMENT_3D('',#36276,#29913,#29914);
#25839=AXIS2_PLACEMENT_3D('',#36278,#29915,#29916);
#25840=AXIS2_PLACEMENT_3D('',#36279,#29917,#29918);
#25841=AXIS2_PLACEMENT_3D('',#36281,#29919,#29920);
#25842=AXIS2_PLACEMENT_3D('',#36283,#29922,#29923);
#25843=AXIS2_PLACEMENT_3D('',#36285,#29924,#29925);
#25844=AXIS2_PLACEMENT_3D('',#36287,#29927,#29928);
#25845=AXIS2_PLACEMENT_3D('',#36288,#29929,#29930);
#25846=AXIS2_PLACEMENT_3D('',#36289,#29931,#29932);
#25847=AXIS2_PLACEMENT_3D('',#36291,#29933,#29934);
#25848=AXIS2_PLACEMENT_3D('',#36295,#29936,#29937);
#25849=AXIS2_PLACEMENT_3D('',#36296,#29938,#29939);
#25850=AXIS2_PLACEMENT_3D('',#36297,#29940,#29941);
#25851=AXIS2_PLACEMENT_3D('',#36299,#29942,#29943);
#25852=AXIS2_PLACEMENT_3D('',#36300,#29944,#29945);
#25853=AXIS2_PLACEMENT_3D('',#36303,#29947,#29948);
#25854=AXIS2_PLACEMENT_3D('',#36304,#29949,#29950);
#25855=AXIS2_PLACEMENT_3D('',#36307,#29951,#29952);
#25856=AXIS2_PLACEMENT_3D('',#36308,#29953,#29954);
#25857=AXIS2_PLACEMENT_3D('',#36310,#29956,#29957);
#25858=AXIS2_PLACEMENT_3D('',#36314,#29959,#29960);
#25859=AXIS2_PLACEMENT_3D('',#36373,#29963,#29964);
#25860=AXIS2_PLACEMENT_3D('',#36374,#29965,#29966);
#25861=AXIS2_PLACEMENT_3D('',#36376,#29967,#29968);
#25862=AXIS2_PLACEMENT_3D('',#36504,#29970,#29971);
#25863=AXIS2_PLACEMENT_3D('',#36506,#29972,#29973);
#25864=AXIS2_PLACEMENT_3D('',#36803,#29975,#29976);
#25865=AXIS2_PLACEMENT_3D('',#36804,#29977,#29978);
#25866=AXIS2_PLACEMENT_3D('',#36805,#29979,#29980);
#25867=AXIS2_PLACEMENT_3D('',#36806,#29981,#29982);
#25868=AXIS2_PLACEMENT_3D('',#36808,#29984,#29985);
#25869=AXIS2_PLACEMENT_3D('',#36828,#29986,#29987);
#25870=AXIS2_PLACEMENT_3D('',#36830,#29988,#29989);
#25871=AXIS2_PLACEMENT_3D('',#36832,#29991,#29992);
#25872=AXIS2_PLACEMENT_3D('',#36913,#29993,#29994);
#25873=AXIS2_PLACEMENT_3D('',#36915,#29995,#29996);
#25874=AXIS2_PLACEMENT_3D('',#36918,#29998,#29999);
#25875=AXIS2_PLACEMENT_3D('',#36919,#30000,#30001);
#25876=AXIS2_PLACEMENT_3D('',#36922,#30003,#30004);
#25877=AXIS2_PLACEMENT_3D('',#36923,#30005,#30006);
#25878=AXIS2_PLACEMENT_3D('',#36925,#30007,#30008);
#25879=AXIS2_PLACEMENT_3D('',#36927,#30009,#30010);
#25880=AXIS2_PLACEMENT_3D('',#36929,#30011,#30012);
#25881=AXIS2_PLACEMENT_3D('',#36930,#30013,#30014);
#25882=AXIS2_PLACEMENT_3D('',#36932,#30015,#30016);
#25883=AXIS2_PLACEMENT_3D('',#36934,#30018,#30019);
#25884=AXIS2_PLACEMENT_3D('',#36936,#30020,#30021);
#25885=AXIS2_PLACEMENT_3D('',#36938,#30022,#30023);
#25886=AXIS2_PLACEMENT_3D('',#36940,#30024,#30025);
#25887=AXIS2_PLACEMENT_3D('',#36941,#30026,#30027);
#25888=AXIS2_PLACEMENT_3D('',#36944,#30029,#30030);
#25889=AXIS2_PLACEMENT_3D('',#36945,#30031,#30032);
#25890=AXIS2_PLACEMENT_3D('',#36948,#30034,#30035);
#25891=AXIS2_PLACEMENT_3D('',#36949,#30036,#30037);
#25892=AXIS2_PLACEMENT_3D('',#36951,#30039,#30040);
#25893=AXIS2_PLACEMENT_3D('',#36954,#30042,#30043);
#25894=AXIS2_PLACEMENT_3D('',#36955,#30044,#30045);
#25895=AXIS2_PLACEMENT_3D('',#36958,#30047,#30048);
#25896=AXIS2_PLACEMENT_3D('',#36959,#30049,#30050);
#25897=AXIS2_PLACEMENT_3D('',#36961,#30052,#30053);
#25898=AXIS2_PLACEMENT_3D('',#36962,#30054,#30055);
#25899=AXIS2_PLACEMENT_3D('',#36963,#30056,#30057);
#25900=AXIS2_PLACEMENT_3D('',#36967,#30059,#30060);
#25901=AXIS2_PLACEMENT_3D('',#36968,#30061,#30062);
#25902=AXIS2_PLACEMENT_3D('',#36969,#30063,#30064);
#25903=AXIS2_PLACEMENT_3D('',#36973,#30066,#30067);
#25904=AXIS2_PLACEMENT_3D('',#36974,#30068,#30069);
#25905=AXIS2_PLACEMENT_3D('',#36975,#30070,#30071);
#25906=AXIS2_PLACEMENT_3D('',#36977,#30073,#30074);
#25907=AXIS2_PLACEMENT_3D('',#36978,#30075,#30076);
#25908=AXIS2_PLACEMENT_3D('',#36980,#30077,#30078);
#25909=AXIS2_PLACEMENT_3D('',#36984,#30080,#30081);
#25910=AXIS2_PLACEMENT_3D('',#36985,#30082,#30083);
#25911=AXIS2_PLACEMENT_3D('',#36986,#30084,#30085);
#25912=AXIS2_PLACEMENT_3D('',#36989,#30086,#30087);
#25913=AXIS2_PLACEMENT_3D('',#36990,#30088,#30089);
#25914=AXIS2_PLACEMENT_3D('',#36992,#30091,#30092);
#25915=AXIS2_PLACEMENT_3D('',#36995,#30093,#30094);
#25916=AXIS2_PLACEMENT_3D('',#36997,#30095,#30096);
#25917=AXIS2_PLACEMENT_3D('',#36999,#30097,#30098);
#25918=AXIS2_PLACEMENT_3D('',#37000,#30099,#30100);
#25919=AXIS2_PLACEMENT_3D('',#37002,#30101,#30102);
#25920=AXIS2_PLACEMENT_3D('',#37004,#30103,#30104);
#25921=AXIS2_PLACEMENT_3D('',#37005,#30105,#30106);
#25922=AXIS2_PLACEMENT_3D('',#37006,#30107,#30108);
#25923=AXIS2_PLACEMENT_3D('',#37007,#30109,#30110);
#25924=AXIS2_PLACEMENT_3D('',#37008,#30111,#30112);
#25925=AXIS2_PLACEMENT_3D('',#37011,#30114,#30115);
#25926=AXIS2_PLACEMENT_3D('',#37012,#30116,#30117);
#25927=AXIS2_PLACEMENT_3D('',#37014,#30118,#30119);
#25928=AXIS2_PLACEMENT_3D('',#37016,#30120,#30121);
#25929=AXIS2_PLACEMENT_3D('',#37018,#30122,#30123);
#25930=AXIS2_PLACEMENT_3D('',#37020,#30124,#30125);
#25931=AXIS2_PLACEMENT_3D('',#37021,#30126,#30127);
#25932=AXIS2_PLACEMENT_3D('',#37024,#30128,#30129);
#25933=AXIS2_PLACEMENT_3D('',#37025,#30130,#30131);
#25934=AXIS2_PLACEMENT_3D('',#37027,#30133,#30134);
#25935=AXIS2_PLACEMENT_3D('',#37030,#30135,#30136);
#25936=AXIS2_PLACEMENT_3D('',#37031,#30137,#30138);
#25937=AXIS2_PLACEMENT_3D('',#37033,#30140,#30141);
#25938=AXIS2_PLACEMENT_3D('',#37036,#30143,#30144);
#25939=AXIS2_PLACEMENT_3D('',#37037,#30145,#30146);
#25940=AXIS2_PLACEMENT_3D('',#37040,#30148,#30149);
#25941=AXIS2_PLACEMENT_3D('',#37041,#30150,#30151);
#25942=AXIS2_PLACEMENT_3D('',#37043,#30153,#30154);
#25943=AXIS2_PLACEMENT_3D('',#37046,#30156,#30157);
#25944=AXIS2_PLACEMENT_3D('',#37047,#30158,#30159);
#25945=AXIS2_PLACEMENT_3D('',#37050,#30161,#30162);
#25946=AXIS2_PLACEMENT_3D('',#37051,#30163,#30164);
#25947=AXIS2_PLACEMENT_3D('',#37053,#30166,#30167);
#25948=AXIS2_PLACEMENT_3D('',#37056,#30169,#30170);
#25949=AXIS2_PLACEMENT_3D('',#37057,#30171,#30172);
#25950=AXIS2_PLACEMENT_3D('',#37060,#30174,#30175);
#25951=AXIS2_PLACEMENT_3D('',#37061,#30176,#30177);
#25952=AXIS2_PLACEMENT_3D('',#37063,#30179,#30180);
#25953=AXIS2_PLACEMENT_3D('',#37065,#30182,#30183);
#25954=AXIS2_PLACEMENT_3D('',#37066,#30184,#30185);
#25955=AXIS2_PLACEMENT_3D('',#37075,#30190,#30191);
#25956=AXIS2_PLACEMENT_3D('',#37084,#30196,#30197);
#25957=AXIS2_PLACEMENT_3D('',#37087,#30200,#30201);
#25958=AXIS2_PLACEMENT_3D('',#37088,#30202,#30203);
#25959=AXIS2_PLACEMENT_3D('',#37090,#30204,#30205);
#25960=AXIS2_PLACEMENT_3D('',#37092,#30206,#30207);
#25961=AXIS2_PLACEMENT_3D('',#37094,#30208,#30209);
#25962=AXIS2_PLACEMENT_3D('',#37099,#30211,#30212);
#25963=AXIS2_PLACEMENT_3D('',#37102,#30214,#30215);
#25964=AXIS2_PLACEMENT_3D('',#37107,#30217,#30218);
#25965=AXIS2_PLACEMENT_3D('',#37110,#30220,#30221);
#25966=AXIS2_PLACEMENT_3D('',#37115,#30223,#30224);
#25967=AXIS2_PLACEMENT_3D('',#37118,#30226,#30227);
#25968=AXIS2_PLACEMENT_3D('',#37123,#30229,#30230);
#25969=AXIS2_PLACEMENT_3D('',#37126,#30232,#30233);
#25970=AXIS2_PLACEMENT_3D('',#37131,#30235,#30236);
#25971=AXIS2_PLACEMENT_3D('',#37134,#30238,#30239);
#25972=AXIS2_PLACEMENT_3D('',#37139,#30241,#30242);
#25973=AXIS2_PLACEMENT_3D('',#37142,#30244,#30245);
#25974=AXIS2_PLACEMENT_3D('',#37144,#30246,#30247);
#25975=AXIS2_PLACEMENT_3D('',#37145,#30248,#30249);
#25976=AXIS2_PLACEMENT_3D('',#37146,#30250,#30251);
#25977=AXIS2_PLACEMENT_3D('',#37147,#30252,#30253);
#25978=AXIS2_PLACEMENT_3D('',#37149,#30254,#30255);
#25979=AXIS2_PLACEMENT_3D('',#37151,#30257,#30258);
#25980=AXIS2_PLACEMENT_3D('',#37153,#30259,#30260);
#25981=AXIS2_PLACEMENT_3D('',#37155,#30262,#30263);
#25982=AXIS2_PLACEMENT_3D('',#37157,#30264,#30265);
#25983=AXIS2_PLACEMENT_3D('',#37159,#30267,#30268);
#25984=AXIS2_PLACEMENT_3D('',#37165,#30272,#30273);
#25985=AXIS2_PLACEMENT_3D('',#37168,#30275,#30276);
#25986=AXIS2_PLACEMENT_3D('',#37169,#30277,#30278);
#25987=AXIS2_PLACEMENT_3D('',#37173,#30281,#30282);
#25988=AXIS2_PLACEMENT_3D('',#37174,#30283,#30284);
#25989=AXIS2_PLACEMENT_3D('',#37175,#30285,#30286);
#25990=AXIS2_PLACEMENT_3D('',#37181,#30290,#30291);
#25991=AXIS2_PLACEMENT_3D('',#37184,#30293,#30294);
#25992=AXIS2_PLACEMENT_3D('',#37185,#30295,#30296);
#25993=AXIS2_PLACEMENT_3D('',#37189,#30299,#30300);
#25994=AXIS2_PLACEMENT_3D('',#37190,#30301,#30302);
#25995=AXIS2_PLACEMENT_3D('',#37191,#30303,#30304);
#25996=AXIS2_PLACEMENT_3D('',#37197,#30308,#30309);
#25997=AXIS2_PLACEMENT_3D('',#37200,#30311,#30312);
#25998=AXIS2_PLACEMENT_3D('',#37201,#30313,#30314);
#25999=AXIS2_PLACEMENT_3D('',#37205,#30317,#30318);
#26000=AXIS2_PLACEMENT_3D('',#37206,#30319,#30320);
#26001=AXIS2_PLACEMENT_3D('',#37207,#30321,#30322);
#26002=AXIS2_PLACEMENT_3D('',#37213,#30326,#30327);
#26003=AXIS2_PLACEMENT_3D('',#37216,#30329,#30330);
#26004=AXIS2_PLACEMENT_3D('',#37217,#30331,#30332);
#26005=AXIS2_PLACEMENT_3D('',#37221,#30335,#30336);
#26006=AXIS2_PLACEMENT_3D('',#37222,#30337,#30338);
#26007=AXIS2_PLACEMENT_3D('',#37223,#30339,#30340);
#26008=AXIS2_PLACEMENT_3D('',#37229,#30344,#30345);
#26009=AXIS2_PLACEMENT_3D('',#37232,#30347,#30348);
#26010=AXIS2_PLACEMENT_3D('',#37233,#30349,#30350);
#26011=AXIS2_PLACEMENT_3D('',#37237,#30353,#30354);
#26012=AXIS2_PLACEMENT_3D('',#37238,#30355,#30356);
#26013=AXIS2_PLACEMENT_3D('',#37239,#30357,#30358);
#26014=AXIS2_PLACEMENT_3D('',#37245,#30362,#30363);
#26015=AXIS2_PLACEMENT_3D('',#37248,#30365,#30366);
#26016=AXIS2_PLACEMENT_3D('',#37249,#30367,#30368);
#26017=AXIS2_PLACEMENT_3D('',#37253,#30371,#30372);
#26018=AXIS2_PLACEMENT_3D('',#37254,#30373,#30374);
#26019=AXIS2_PLACEMENT_3D('',#37255,#30375,#30376);
#26020=AXIS2_PLACEMENT_3D('',#37257,#30377,#30378);
#26021=AXIS2_PLACEMENT_3D('',#37259,#30380,#30381);
#26022=AXIS2_PLACEMENT_3D('',#37260,#30382,#30383);
#26023=AXIS2_PLACEMENT_3D('',#37261,#30384,#30385);
#26024=AXIS2_PLACEMENT_3D('',#37270,#30390,#30391);
#26025=AXIS2_PLACEMENT_3D('',#37276,#30395,#30396);
#26026=AXIS2_PLACEMENT_3D('',#37304,#30411,#30412);
#26027=AXIS2_PLACEMENT_3D('',#37310,#30416,#30417);
#26028=AXIS2_PLACEMENT_3D('',#37314,#30420,#30421);
#26029=AXIS2_PLACEMENT_3D('',#37337,#30434,#30435);
#26030=AXIS2_PLACEMENT_3D('',#37339,#30437,#30438);
#26031=AXIS2_PLACEMENT_3D('',#37349,#30444,#30445);
#26032=AXIS2_PLACEMENT_3D('',#37351,#30447,#30448);
#26033=AXIS2_PLACEMENT_3D('',#37353,#30450,#30451);
#26034=AXIS2_PLACEMENT_3D('',#37355,#30453,#30454);
#26035=AXIS2_PLACEMENT_3D('',#37365,#30460,#30461);
#26036=AXIS2_PLACEMENT_3D('',#37366,#30462,#30463);
#26037=AXIS2_PLACEMENT_3D('',#37369,#30466,#30467);
#26038=AXIS2_PLACEMENT_3D('',#37379,#30472,#30473);
#26039=AXIS2_PLACEMENT_3D('',#37381,#30474,#30475);
#26040=AXIS2_PLACEMENT_3D('',#37383,#30477,#30478);
#26041=AXIS2_PLACEMENT_3D('',#37385,#30480,#30481);
#26042=AXIS2_PLACEMENT_3D('',#37386,#30482,#30483);
#26043=AXIS2_PLACEMENT_3D('',#37388,#30484,#30485);
#26044=AXIS2_PLACEMENT_3D('',#37390,#30487,#30488);
#26045=AXIS2_PLACEMENT_3D('',#37392,#30489,#30490);
#26046=AXIS2_PLACEMENT_3D('',#37394,#30492,#30493);
#26047=AXIS2_PLACEMENT_3D('',#37400,#30497,#30498);
#26048=AXIS2_PLACEMENT_3D('',#37406,#30502,#30503);
#26049=AXIS2_PLACEMENT_3D('',#37409,#30506,#30507);
#26050=AXIS2_PLACEMENT_3D('',#37410,#30508,#30509);
#26051=AXIS2_PLACEMENT_3D('',#37411,#30510,#30511);
#26052=AXIS2_PLACEMENT_3D('',#37417,#30515,#30516);
#26053=AXIS2_PLACEMENT_3D('',#37421,#30519,#30520);
#26054=AXIS2_PLACEMENT_3D('',#37425,#30523,#30524);
#26055=AXIS2_PLACEMENT_3D('',#37427,#30526,#30527);
#26056=AXIS2_PLACEMENT_3D('',#37428,#30528,#30529);
#26057=AXIS2_PLACEMENT_3D('',#37434,#30533,#30534);
#26058=AXIS2_PLACEMENT_3D('',#37438,#30537,#30538);
#26059=AXIS2_PLACEMENT_3D('',#37442,#30541,#30542);
#26060=AXIS2_PLACEMENT_3D('',#37444,#30544,#30545);
#26061=AXIS2_PLACEMENT_3D('',#37445,#30546,#30547);
#26062=AXIS2_PLACEMENT_3D('',#37446,#30548,#30549);
#26063=AXIS2_PLACEMENT_3D('',#37447,#30550,#30551);
#26064=AXIS2_PLACEMENT_3D('',#37450,#30552,#30553);
#26065=AXIS2_PLACEMENT_3D('',#37454,#30555,#30556);
#26066=AXIS2_PLACEMENT_3D('',#37456,#30558,#30559);
#26067=AXIS2_PLACEMENT_3D('',#37460,#30561,#30562);
#26068=AXIS2_PLACEMENT_3D('',#37466,#30565,#30566);
#26069=AXIS2_PLACEMENT_3D('',#37470,#30568,#30569);
#26070=AXIS2_PLACEMENT_3D('',#37474,#30571,#30572);
#26071=AXIS2_PLACEMENT_3D('',#37478,#30575,#30576);
#26072=AXIS2_PLACEMENT_3D('',#37482,#30579,#30580);
#26073=AXIS2_PLACEMENT_3D('',#37484,#30581,#30582);
#26074=AXIS2_PLACEMENT_3D('',#37486,#30584,#30585);
#26075=AXIS2_PLACEMENT_3D('',#37488,#30586,#30587);
#26076=AXIS2_PLACEMENT_3D('',#37491,#30589,#30590);
#26077=AXIS2_PLACEMENT_3D('',#37492,#30591,#30592);
#26078=AXIS2_PLACEMENT_3D('',#37494,#30593,#30594);
#26079=AXIS2_PLACEMENT_3D('',#37497,#30596,#30597);
#26080=AXIS2_PLACEMENT_3D('',#37498,#30598,#30599);
#26081=AXIS2_PLACEMENT_3D('',#37504,#30603,#30604);
#26082=AXIS2_PLACEMENT_3D('',#37507,#30606,#30607);
#26083=AXIS2_PLACEMENT_3D('',#37508,#30608,#30609);
#26084=AXIS2_PLACEMENT_3D('',#37512,#30612,#30613);
#26085=AXIS2_PLACEMENT_3D('',#37513,#30614,#30615);
#26086=AXIS2_PLACEMENT_3D('',#37514,#30616,#30617);
#26087=AXIS2_PLACEMENT_3D('',#37515,#30618,#30619);
#26088=AXIS2_PLACEMENT_3D('',#37517,#30621,#30622);
#26089=AXIS2_PLACEMENT_3D('',#37519,#30623,#30624);
#26090=AXIS2_PLACEMENT_3D('',#37521,#30625,#30626);
#26091=AXIS2_PLACEMENT_3D('',#37523,#30628,#30629);
#26092=AXIS2_PLACEMENT_3D('',#37527,#30632,#30633);
#26093=AXIS2_PLACEMENT_3D('',#37531,#30636,#30637);
#26094=AXIS2_PLACEMENT_3D('',#37540,#30642,#30643);
#26095=AXIS2_PLACEMENT_3D('',#37547,#30648,#30649);
#26096=AXIS2_PLACEMENT_3D('',#37553,#30653,#30654);
#26097=AXIS2_PLACEMENT_3D('',#37556,#30657,#30658);
#26098=AXIS2_PLACEMENT_3D('',#37557,#30659,#30660);
#26099=AXIS2_PLACEMENT_3D('',#37558,#30661,#30662);
#26100=AXIS2_PLACEMENT_3D('',#37559,#30663,#30664);
#26101=AXIS2_PLACEMENT_3D('',#37568,#30669,#30670);
#26102=AXIS2_PLACEMENT_3D('',#37574,#30674,#30675);
#26103=AXIS2_PLACEMENT_3D('',#37580,#30679,#30680);
#26104=AXIS2_PLACEMENT_3D('',#37583,#30683,#30684);
#26105=AXIS2_PLACEMENT_3D('',#37584,#30685,#30686);
#26106=AXIS2_PLACEMENT_3D('',#37593,#30691,#30692);
#26107=AXIS2_PLACEMENT_3D('',#37599,#30696,#30697);
#26108=AXIS2_PLACEMENT_3D('',#37605,#30701,#30702);
#26109=AXIS2_PLACEMENT_3D('',#37608,#30705,#30706);
#26110=AXIS2_PLACEMENT_3D('',#37609,#30707,#30708);
#26111=AXIS2_PLACEMENT_3D('',#37611,#30709,#30710);
#26112=AXIS2_PLACEMENT_3D('',#37614,#30712,#30713);
#26113=AXIS2_PLACEMENT_3D('',#37615,#30714,#30715);
#26114=AXIS2_PLACEMENT_3D('',#37616,#30716,#30717);
#26115=AXIS2_PLACEMENT_3D('',#37625,#30722,#30723);
#26116=AXIS2_PLACEMENT_3D('',#37631,#30727,#30728);
#26117=AXIS2_PLACEMENT_3D('',#37637,#30732,#30733);
#26118=AXIS2_PLACEMENT_3D('',#37640,#30736,#30737);
#26119=AXIS2_PLACEMENT_3D('',#37641,#30738,#30739);
#26120=AXIS2_PLACEMENT_3D('',#37650,#30744,#30745);
#26121=AXIS2_PLACEMENT_3D('',#37656,#30749,#30750);
#26122=AXIS2_PLACEMENT_3D('',#37662,#30754,#30755);
#26123=AXIS2_PLACEMENT_3D('',#37665,#30758,#30759);
#26124=AXIS2_PLACEMENT_3D('',#37666,#30760,#30761);
#26125=AXIS2_PLACEMENT_3D('',#37675,#30766,#30767);
#26126=AXIS2_PLACEMENT_3D('',#37681,#30771,#30772);
#26127=AXIS2_PLACEMENT_3D('',#37687,#30776,#30777);
#26128=AXIS2_PLACEMENT_3D('',#37690,#30780,#30781);
#26129=AXIS2_PLACEMENT_3D('',#37691,#30782,#30783);
#26130=AXIS2_PLACEMENT_3D('',#37700,#30788,#30789);
#26131=AXIS2_PLACEMENT_3D('',#37706,#30793,#30794);
#26132=AXIS2_PLACEMENT_3D('',#37712,#30798,#30799);
#26133=AXIS2_PLACEMENT_3D('',#37715,#30802,#30803);
#26134=AXIS2_PLACEMENT_3D('',#37716,#30804,#30805);
#26135=AXIS2_PLACEMENT_3D('',#37718,#30806,#30807);
#26136=AXIS2_PLACEMENT_3D('',#37721,#30809,#30810);
#26137=AXIS2_PLACEMENT_3D('',#37722,#30811,#30812);
#26138=AXIS2_PLACEMENT_3D('',#37724,#30813,#30814);
#26139=AXIS2_PLACEMENT_3D('',#37727,#30816,#30817);
#26140=AXIS2_PLACEMENT_3D('',#37728,#30818,#30819);
#26141=AXIS2_PLACEMENT_3D('',#37730,#30820,#30821);
#26142=AXIS2_PLACEMENT_3D('',#37733,#30823,#30824);
#26143=AXIS2_PLACEMENT_3D('',#37734,#30825,#30826);
#26144=AXIS2_PLACEMENT_3D('',#37736,#30827,#30828);
#26145=AXIS2_PLACEMENT_3D('',#37739,#30830,#30831);
#26146=AXIS2_PLACEMENT_3D('',#37740,#30832,#30833);
#26147=AXIS2_PLACEMENT_3D('',#37742,#30834,#30835);
#26148=AXIS2_PLACEMENT_3D('',#37743,#30836,#30837);
#26149=AXIS2_PLACEMENT_3D('',#37745,#30838,#30839);
#26150=AXIS2_PLACEMENT_3D('',#37747,#30841,#30842);
#26151=AXIS2_PLACEMENT_3D('',#37748,#30843,#30844);
#26152=AXIS2_PLACEMENT_3D('',#37749,#30845,#30846);
#26153=AXIS2_PLACEMENT_3D('',#37778,#30849,#30850);
#26154=AXIS2_PLACEMENT_3D('',#37785,#30851,#30852);
#26155=AXIS2_PLACEMENT_3D('',#37805,#30853,#30854);
#26156=AXIS2_PLACEMENT_3D('',#37859,#30856,#30857);
#26157=AXIS2_PLACEMENT_3D('',#37907,#30859,#30860);
#26158=AXIS2_PLACEMENT_3D('',#37919,#30862,#30863);
#26159=AXIS2_PLACEMENT_3D('',#37925,#30864,#30865);
#26160=AXIS2_PLACEMENT_3D('',#37949,#30867,#30868);
#26161=AXIS2_PLACEMENT_3D('',#37974,#30870,#30871);
#26162=AXIS2_PLACEMENT_3D('',#37999,#30873,#30874);
#26163=AXIS2_PLACEMENT_3D('',#38048,#30875,#30876);
#26164=AXIS2_PLACEMENT_3D('',#38050,#30877,#30878);
#26165=AXIS2_PLACEMENT_3D('',#38286,#30879,#30880);
#26166=AXIS2_PLACEMENT_3D('',#38334,#30881,#30882);
#26167=AXIS2_PLACEMENT_3D('',#38335,#30883,#30884);
#26168=AXIS2_PLACEMENT_3D('',#38474,#30885,#30886);
#26169=AXIS2_PLACEMENT_3D('',#38475,#30887,#30888);
#26170=AXIS2_PLACEMENT_3D('',#38476,#30889,#30890);
#26171=AXIS2_PLACEMENT_3D('',#38480,#30892,#30893);
#26172=AXIS2_PLACEMENT_3D('',#38481,#30894,#30895);
#26173=AXIS2_PLACEMENT_3D('',#38490,#30900,#30901);
#26174=AXIS2_PLACEMENT_3D('',#38496,#30905,#30906);
#26175=AXIS2_PLACEMENT_3D('',#38502,#30910,#30911);
#26176=AXIS2_PLACEMENT_3D('',#38508,#30915,#30916);
#26177=AXIS2_PLACEMENT_3D('',#38514,#30920,#30921);
#26178=AXIS2_PLACEMENT_3D('',#38517,#30924,#30925);
#26179=AXIS2_PLACEMENT_3D('',#38518,#30926,#30927);
#26180=AXIS2_PLACEMENT_3D('',#38520,#30928,#30929);
#26181=AXIS2_PLACEMENT_3D('',#38521,#30930,#30931);
#26182=AXIS2_PLACEMENT_3D('',#38523,#30933,#30934);
#26183=AXIS2_PLACEMENT_3D('',#38525,#30935,#30936);
#26184=AXIS2_PLACEMENT_3D('',#38527,#30938,#30939);
#26185=AXIS2_PLACEMENT_3D('',#38528,#30940,#30941);
#26186=AXIS2_PLACEMENT_3D('',#38529,#30942,#30943);
#26187=AXIS2_PLACEMENT_3D('',#38554,#30945,#30946);
#26188=AXIS2_PLACEMENT_3D('',#38557,#30948,#30949);
#26189=AXIS2_PLACEMENT_3D('',#38559,#30950,#30951);
#26190=AXIS2_PLACEMENT_3D('',#38576,#30952,#30953);
#26191=AXIS2_PLACEMENT_3D('',#38624,#30955,#30956);
#26192=AXIS2_PLACEMENT_3D('',#38672,#30958,#30959);
#26193=AXIS2_PLACEMENT_3D('',#38726,#30961,#30962);
#26194=AXIS2_PLACEMENT_3D('',#38774,#30964,#30965);
#26195=AXIS2_PLACEMENT_3D('',#38822,#30967,#30968);
#26196=AXIS2_PLACEMENT_3D('',#38873,#30970,#30971);
#26197=AXIS2_PLACEMENT_3D('',#38921,#30973,#30974);
#26198=AXIS2_PLACEMENT_3D('',#38936,#30976,#30977);
#26199=AXIS2_PLACEMENT_3D('',#38945,#30978,#30979);
#26200=AXIS2_PLACEMENT_3D('',#38970,#30981,#30982);
#26201=AXIS2_PLACEMENT_3D('',#38995,#30984,#30985);
#26202=AXIS2_PLACEMENT_3D('',#39019,#30987,#30988);
#26203=AXIS2_PLACEMENT_3D('',#39044,#30990,#30991);
#26204=AXIS2_PLACEMENT_3D('',#39069,#30993,#30994);
#26205=AXIS2_PLACEMENT_3D('',#39093,#30996,#30997);
#26206=AXIS2_PLACEMENT_3D('',#39458,#30999,#31000);
#26207=AXIS2_PLACEMENT_3D('',#39509,#31001,#31002);
#26208=AXIS2_PLACEMENT_3D('',#39510,#31003,#31004);
#26209=AXIS2_PLACEMENT_3D('',#39796,#31005,#31006);
#26210=AXIS2_PLACEMENT_3D('',#39797,#31007,#31008);
#26211=AXIS2_PLACEMENT_3D('',#39798,#31009,#31010);
#26212=AXIS2_PLACEMENT_3D('',#39802,#31012,#31013);
#26213=AXIS2_PLACEMENT_3D('',#39803,#31014,#31015);
#26214=AXIS2_PLACEMENT_3D('',#39806,#31017,#31018);
#26215=AXIS2_PLACEMENT_3D('',#39807,#31019,#31020);
#26216=AXIS2_PLACEMENT_3D('',#39810,#31022,#31023);
#26217=AXIS2_PLACEMENT_3D('',#39811,#31024,#31025);
#26218=AXIS2_PLACEMENT_3D('',#39821,#31026,#31027);
#26219=AXIS2_PLACEMENT_3D('',#39822,#31028,#31029);
#26220=AXIS2_PLACEMENT_3D('',#39832,#31030,#31031);
#26221=AXIS2_PLACEMENT_3D('',#39833,#31032,#31033);
#26222=AXIS2_PLACEMENT_3D('',#39843,#31034,#31035);
#26223=AXIS2_PLACEMENT_3D('',#39844,#31036,#31037);
#26224=AXIS2_PLACEMENT_3D('',#39854,#31038,#31039);
#26225=AXIS2_PLACEMENT_3D('',#39855,#31040,#31041);
#26226=AXIS2_PLACEMENT_3D('',#39865,#31042,#31043);
#26227=AXIS2_PLACEMENT_3D('',#39866,#31044,#31045);
#26228=AXIS2_PLACEMENT_3D('',#39873,#31046,#31047);
#26229=AXIS2_PLACEMENT_3D('',#39877,#31048,#31049);
#26230=AXIS2_PLACEMENT_3D('',#39892,#31054,#31055);
#26231=AXIS2_PLACEMENT_3D('',#39905,#31059,#31060);
#26232=AXIS2_PLACEMENT_3D('',#39918,#31064,#31065);
#26233=AXIS2_PLACEMENT_3D('',#39922,#31069,#31070);
#26234=AXIS2_PLACEMENT_3D('',#39934,#31073,#31074);
#26235=AXIS2_PLACEMENT_3D('',#39941,#31075,#31076);
#26236=AXIS2_PLACEMENT_3D('',#39945,#31077,#31078);
#26237=AXIS2_PLACEMENT_3D('',#39947,#31079,#31080);
#26238=AXIS2_PLACEMENT_3D('',#39951,#31081,#31082);
#26239=AXIS2_PLACEMENT_3D('',#39952,#31083,#31084);
#26240=AXIS2_PLACEMENT_3D('',#39953,#31085,#31086);
#26241=AXIS2_PLACEMENT_3D('',#39954,#31087,#31088);
#26242=AXIS2_PLACEMENT_3D('',#39955,#31089,#31090);
#26243=AXIS2_PLACEMENT_3D('',#39956,#31091,#31092);
#26244=AXIS2_PLACEMENT_3D('',#39957,#31093,#31094);
#26245=AXIS2_PLACEMENT_3D('',#39962,#31095,#31096);
#26246=AXIS2_PLACEMENT_3D('',#39963,#31097,#31098);
#26247=AXIS2_PLACEMENT_3D('',#39966,#31101,#31102);
#26248=AXIS2_PLACEMENT_3D('',#39968,#31103,#31104);
#26249=AXIS2_PLACEMENT_3D('',#39969,#31105,#31106);
#26250=AXIS2_PLACEMENT_3D('',#39971,#31108,#31109);
#26251=AXIS2_PLACEMENT_3D('',#39973,#31111,#31112);
#26252=AXIS2_PLACEMENT_3D('',#39974,#31113,#31114);
#26253=AXIS2_PLACEMENT_3D('',#39975,#31115,#31116);
#26254=AXIS2_PLACEMENT_3D('',#39994,#31118,#31119);
#26255=AXIS2_PLACEMENT_3D('',#39997,#31121,#31122);
#26256=AXIS2_PLACEMENT_3D('',#39999,#31123,#31124);
#26257=AXIS2_PLACEMENT_3D('',#40010,#31125,#31126);
#26258=AXIS2_PLACEMENT_3D('',#40058,#31128,#31129);
#26259=AXIS2_PLACEMENT_3D('',#40109,#31131,#31132);
#26260=AXIS2_PLACEMENT_3D('',#40157,#31134,#31135);
#26261=AXIS2_PLACEMENT_3D('',#40205,#31137,#31138);
#26262=AXIS2_PLACEMENT_3D('',#40259,#31140,#31141);
#26263=AXIS2_PLACEMENT_3D('',#40307,#31143,#31144);
#26264=AXIS2_PLACEMENT_3D('',#40355,#31146,#31147);
#26265=AXIS2_PLACEMENT_3D('',#40409,#31149,#31150);
#26266=AXIS2_PLACEMENT_3D('',#40457,#31152,#31153);
#26267=AXIS2_PLACEMENT_3D('',#40505,#31155,#31156);
#26268=AXIS2_PLACEMENT_3D('',#40553,#31158,#31159);
#26269=AXIS2_PLACEMENT_3D('',#40604,#31161,#31162);
#26270=AXIS2_PLACEMENT_3D('',#40652,#31164,#31165);
#26271=AXIS2_PLACEMENT_3D('',#40700,#31167,#31168);
#26272=AXIS2_PLACEMENT_3D('',#40754,#31170,#31171);
#26273=AXIS2_PLACEMENT_3D('',#40802,#31173,#31174);
#26274=AXIS2_PLACEMENT_3D('',#40850,#31176,#31177);
#26275=AXIS2_PLACEMENT_3D('',#40904,#31179,#31180);
#26276=AXIS2_PLACEMENT_3D('',#40952,#31182,#31183);
#26277=AXIS2_PLACEMENT_3D('',#41000,#31185,#31186);
#26278=AXIS2_PLACEMENT_3D('',#41048,#31188,#31189);
#26279=AXIS2_PLACEMENT_3D('',#41099,#31191,#31192);
#26280=AXIS2_PLACEMENT_3D('',#41147,#31194,#31195);
#26281=AXIS2_PLACEMENT_3D('',#41195,#31197,#31198);
#26282=AXIS2_PLACEMENT_3D('',#41249,#31200,#31201);
#26283=AXIS2_PLACEMENT_3D('',#41297,#31203,#31204);
#26284=AXIS2_PLACEMENT_3D('',#41345,#31206,#31207);
#26285=AXIS2_PLACEMENT_3D('',#41358,#31209,#31210);
#26286=AXIS2_PLACEMENT_3D('',#41364,#31211,#31212);
#26287=AXIS2_PLACEMENT_3D('',#41389,#31214,#31215);
#26288=AXIS2_PLACEMENT_3D('',#41413,#31217,#31218);
#26289=AXIS2_PLACEMENT_3D('',#41438,#31220,#31221);
#26290=AXIS2_PLACEMENT_3D('',#41463,#31223,#31224);
#26291=AXIS2_PLACEMENT_3D('',#41487,#31226,#31227);
#26292=AXIS2_PLACEMENT_3D('',#41512,#31229,#31230);
#26293=AXIS2_PLACEMENT_3D('',#41536,#31232,#31233);
#26294=AXIS2_PLACEMENT_3D('',#41561,#31235,#31236);
#26295=AXIS2_PLACEMENT_3D('',#41585,#31238,#31239);
#26296=AXIS2_PLACEMENT_3D('',#41610,#31241,#31242);
#26297=AXIS2_PLACEMENT_3D('',#41635,#31244,#31245);
#26298=AXIS2_PLACEMENT_3D('',#41659,#31247,#31248);
#26299=AXIS2_PLACEMENT_3D('',#41684,#31250,#31251);
#26300=AXIS2_PLACEMENT_3D('',#41709,#31253,#31254);
#26301=AXIS2_PLACEMENT_3D('',#41733,#31256,#31257);
#26302=AXIS2_PLACEMENT_3D('',#41758,#31259,#31260);
#26303=AXIS2_PLACEMENT_3D('',#41783,#31262,#31263);
#26304=AXIS2_PLACEMENT_3D('',#41807,#31265,#31266);
#26305=AXIS2_PLACEMENT_3D('',#41831,#31268,#31269);
#26306=AXIS2_PLACEMENT_3D('',#41856,#31271,#31272);
#26307=AXIS2_PLACEMENT_3D('',#41881,#31274,#31275);
#26308=AXIS2_PLACEMENT_3D('',#41905,#31277,#31278);
#26309=AXIS2_PLACEMENT_3D('',#41930,#31280,#31281);
#26310=AXIS2_PLACEMENT_3D('',#41955,#31283,#31284);
#26311=AXIS2_PLACEMENT_3D('',#41979,#31286,#31287);
#26312=AXIS2_PLACEMENT_3D('',#42004,#31289,#31290);
#26313=AXIS2_PLACEMENT_3D('',#42029,#31292,#31293);
#26314=AXIS2_PLACEMENT_3D('',#42034,#31295,#31296);
#26315=AXIS2_PLACEMENT_3D('',#42054,#31297,#31298);
#26316=AXIS2_PLACEMENT_3D('',#42103,#31299,#31300);
#26317=AXIS2_PLACEMENT_3D('',#42105,#31301,#31302);
#26318=AXIS2_PLACEMENT_3D('',#42964,#31303,#31304);
#26319=AXIS2_PLACEMENT_3D('',#43014,#31305,#31306);
#26320=AXIS2_PLACEMENT_3D('',#43015,#31307,#31308);
#26321=AXIS2_PLACEMENT_3D('',#43771,#31309,#31310);
#26322=AXIS2_PLACEMENT_3D('',#43774,#31311,#31312);
#26323=AXIS2_PLACEMENT_3D('',#43778,#31315,#31316);
#26324=AXIS2_PLACEMENT_3D('',#43786,#31319,#31320);
#26325=AXIS2_PLACEMENT_3D('',#43792,#31322,#31323);
#26326=AXIS2_PLACEMENT_3D('',#43795,#31324,#31325);
#26327=AXIS2_PLACEMENT_3D('',#43799,#31328,#31329);
#26328=AXIS2_PLACEMENT_3D('',#43807,#31332,#31333);
#26329=AXIS2_PLACEMENT_3D('',#43813,#31335,#31336);
#26330=AXIS2_PLACEMENT_3D('',#43816,#31337,#31338);
#26331=AXIS2_PLACEMENT_3D('',#43820,#31341,#31342);
#26332=AXIS2_PLACEMENT_3D('',#43828,#31345,#31346);
#26333=AXIS2_PLACEMENT_3D('',#43834,#31348,#31349);
#26334=AXIS2_PLACEMENT_3D('',#43837,#31350,#31351);
#26335=AXIS2_PLACEMENT_3D('',#43841,#31354,#31355);
#26336=AXIS2_PLACEMENT_3D('',#43849,#31358,#31359);
#26337=AXIS2_PLACEMENT_3D('',#43855,#31361,#31362);
#26338=AXIS2_PLACEMENT_3D('',#43858,#31363,#31364);
#26339=AXIS2_PLACEMENT_3D('',#43862,#31367,#31368);
#26340=AXIS2_PLACEMENT_3D('',#43870,#31371,#31372);
#26341=AXIS2_PLACEMENT_3D('',#43876,#31374,#31375);
#26342=AXIS2_PLACEMENT_3D('',#43879,#31376,#31377);
#26343=AXIS2_PLACEMENT_3D('',#43883,#31380,#31381);
#26344=AXIS2_PLACEMENT_3D('',#43891,#31384,#31385);
#26345=AXIS2_PLACEMENT_3D('',#43897,#31387,#31388);
#26346=AXIS2_PLACEMENT_3D('',#43900,#31389,#31390);
#26347=AXIS2_PLACEMENT_3D('',#43904,#31393,#31394);
#26348=AXIS2_PLACEMENT_3D('',#43912,#31397,#31398);
#26349=AXIS2_PLACEMENT_3D('',#43918,#31400,#31401);
#26350=AXIS2_PLACEMENT_3D('',#43921,#31402,#31403);
#26351=AXIS2_PLACEMENT_3D('',#43925,#31406,#31407);
#26352=AXIS2_PLACEMENT_3D('',#43933,#31410,#31411);
#26353=AXIS2_PLACEMENT_3D('',#43939,#31413,#31414);
#26354=AXIS2_PLACEMENT_3D('',#43942,#31415,#31416);
#26355=AXIS2_PLACEMENT_3D('',#43946,#31419,#31420);
#26356=AXIS2_PLACEMENT_3D('',#43954,#31423,#31424);
#26357=AXIS2_PLACEMENT_3D('',#43960,#31426,#31427);
#26358=AXIS2_PLACEMENT_3D('',#43963,#31428,#31429);
#26359=AXIS2_PLACEMENT_3D('',#43967,#31432,#31433);
#26360=AXIS2_PLACEMENT_3D('',#43975,#31436,#31437);
#26361=AXIS2_PLACEMENT_3D('',#43981,#31439,#31440);
#26362=AXIS2_PLACEMENT_3D('',#43984,#31441,#31442);
#26363=AXIS2_PLACEMENT_3D('',#43988,#31445,#31446);
#26364=AXIS2_PLACEMENT_3D('',#43996,#31449,#31450);
#26365=AXIS2_PLACEMENT_3D('',#44002,#31452,#31453);
#26366=AXIS2_PLACEMENT_3D('',#44005,#31454,#31455);
#26367=AXIS2_PLACEMENT_3D('',#44009,#31458,#31459);
#26368=AXIS2_PLACEMENT_3D('',#44017,#31462,#31463);
#26369=AXIS2_PLACEMENT_3D('',#44023,#31465,#31466);
#26370=AXIS2_PLACEMENT_3D('',#44026,#31467,#31468);
#26371=AXIS2_PLACEMENT_3D('',#44030,#31471,#31472);
#26372=AXIS2_PLACEMENT_3D('',#44038,#31475,#31476);
#26373=AXIS2_PLACEMENT_3D('',#44044,#31478,#31479);
#26374=AXIS2_PLACEMENT_3D('',#44047,#31480,#31481);
#26375=AXIS2_PLACEMENT_3D('',#44051,#31484,#31485);
#26376=AXIS2_PLACEMENT_3D('',#44059,#31488,#31489);
#26377=AXIS2_PLACEMENT_3D('',#44065,#31491,#31492);
#26378=AXIS2_PLACEMENT_3D('',#44068,#31493,#31494);
#26379=AXIS2_PLACEMENT_3D('',#44072,#31497,#31498);
#26380=AXIS2_PLACEMENT_3D('',#44080,#31501,#31502);
#26381=AXIS2_PLACEMENT_3D('',#44086,#31504,#31505);
#26382=AXIS2_PLACEMENT_3D('',#44089,#31506,#31507);
#26383=AXIS2_PLACEMENT_3D('',#44093,#31510,#31511);
#26384=AXIS2_PLACEMENT_3D('',#44101,#31514,#31515);
#26385=AXIS2_PLACEMENT_3D('',#44107,#31517,#31518);
#26386=AXIS2_PLACEMENT_3D('',#44110,#31519,#31520);
#26387=AXIS2_PLACEMENT_3D('',#44114,#31523,#31524);
#26388=AXIS2_PLACEMENT_3D('',#44122,#31527,#31528);
#26389=AXIS2_PLACEMENT_3D('',#44128,#31530,#31531);
#26390=AXIS2_PLACEMENT_3D('',#44131,#31532,#31533);
#26391=AXIS2_PLACEMENT_3D('',#44136,#31536,#31537);
#26392=AXIS2_PLACEMENT_3D('',#44137,#31538,#31539);
#26393=AXIS2_PLACEMENT_3D('',#44145,#31542,#31543);
#26394=AXIS2_PLACEMENT_3D('',#44151,#31545,#31546);
#26395=AXIS2_PLACEMENT_3D('',#44154,#31547,#31548);
#26396=AXIS2_PLACEMENT_3D('',#44158,#31551,#31552);
#26397=AXIS2_PLACEMENT_3D('',#44166,#31555,#31556);
#26398=AXIS2_PLACEMENT_3D('',#44172,#31558,#31559);
#26399=AXIS2_PLACEMENT_3D('',#44175,#31560,#31561);
#26400=AXIS2_PLACEMENT_3D('',#44179,#31564,#31565);
#26401=AXIS2_PLACEMENT_3D('',#44187,#31568,#31569);
#26402=AXIS2_PLACEMENT_3D('',#44193,#31571,#31572);
#26403=AXIS2_PLACEMENT_3D('',#44196,#31573,#31574);
#26404=AXIS2_PLACEMENT_3D('',#44200,#31577,#31578);
#26405=AXIS2_PLACEMENT_3D('',#44208,#31581,#31582);
#26406=AXIS2_PLACEMENT_3D('',#44214,#31584,#31585);
#26407=AXIS2_PLACEMENT_3D('',#44217,#31586,#31587);
#26408=AXIS2_PLACEMENT_3D('',#44221,#31590,#31591);
#26409=AXIS2_PLACEMENT_3D('',#44229,#31594,#31595);
#26410=AXIS2_PLACEMENT_3D('',#44235,#31597,#31598);
#26411=AXIS2_PLACEMENT_3D('',#44238,#31599,#31600);
#26412=AXIS2_PLACEMENT_3D('',#44242,#31603,#31604);
#26413=AXIS2_PLACEMENT_3D('',#44250,#31607,#31608);
#26414=AXIS2_PLACEMENT_3D('',#44256,#31610,#31611);
#26415=AXIS2_PLACEMENT_3D('',#44259,#31612,#31613);
#26416=AXIS2_PLACEMENT_3D('',#44263,#31616,#31617);
#26417=AXIS2_PLACEMENT_3D('',#44271,#31620,#31621);
#26418=AXIS2_PLACEMENT_3D('',#44277,#31623,#31624);
#26419=AXIS2_PLACEMENT_3D('',#44280,#31625,#31626);
#26420=AXIS2_PLACEMENT_3D('',#44284,#31629,#31630);
#26421=AXIS2_PLACEMENT_3D('',#44292,#31633,#31634);
#26422=AXIS2_PLACEMENT_3D('',#44298,#31636,#31637);
#26423=AXIS2_PLACEMENT_3D('',#44301,#31638,#31639);
#26424=AXIS2_PLACEMENT_3D('',#44305,#31642,#31643);
#26425=AXIS2_PLACEMENT_3D('',#44313,#31646,#31647);
#26426=AXIS2_PLACEMENT_3D('',#44319,#31649,#31650);
#26427=AXIS2_PLACEMENT_3D('',#44322,#31651,#31652);
#26428=AXIS2_PLACEMENT_3D('',#44326,#31655,#31656);
#26429=AXIS2_PLACEMENT_3D('',#44334,#31659,#31660);
#26430=AXIS2_PLACEMENT_3D('',#44340,#31662,#31663);
#26431=AXIS2_PLACEMENT_3D('',#44343,#31664,#31665);
#26432=AXIS2_PLACEMENT_3D('',#44347,#31668,#31669);
#26433=AXIS2_PLACEMENT_3D('',#44355,#31672,#31673);
#26434=AXIS2_PLACEMENT_3D('',#44361,#31675,#31676);
#26435=AXIS2_PLACEMENT_3D('',#44364,#31677,#31678);
#26436=AXIS2_PLACEMENT_3D('',#44368,#31681,#31682);
#26437=AXIS2_PLACEMENT_3D('',#44376,#31685,#31686);
#26438=AXIS2_PLACEMENT_3D('',#44382,#31688,#31689);
#26439=AXIS2_PLACEMENT_3D('',#44385,#31690,#31691);
#26440=AXIS2_PLACEMENT_3D('',#44389,#31694,#31695);
#26441=AXIS2_PLACEMENT_3D('',#44397,#31698,#31699);
#26442=AXIS2_PLACEMENT_3D('',#44403,#31701,#31702);
#26443=AXIS2_PLACEMENT_3D('',#44406,#31703,#31704);
#26444=AXIS2_PLACEMENT_3D('',#44410,#31707,#31708);
#26445=AXIS2_PLACEMENT_3D('',#44418,#31711,#31712);
#26446=AXIS2_PLACEMENT_3D('',#44424,#31714,#31715);
#26447=AXIS2_PLACEMENT_3D('',#44427,#31716,#31717);
#26448=AXIS2_PLACEMENT_3D('',#44431,#31720,#31721);
#26449=AXIS2_PLACEMENT_3D('',#44439,#31724,#31725);
#26450=AXIS2_PLACEMENT_3D('',#44445,#31727,#31728);
#26451=AXIS2_PLACEMENT_3D('',#44448,#31729,#31730);
#26452=AXIS2_PLACEMENT_3D('',#44452,#31733,#31734);
#26453=AXIS2_PLACEMENT_3D('',#44460,#31737,#31738);
#26454=AXIS2_PLACEMENT_3D('',#44466,#31740,#31741);
#26455=AXIS2_PLACEMENT_3D('',#44469,#31742,#31743);
#26456=AXIS2_PLACEMENT_3D('',#44473,#31746,#31747);
#26457=AXIS2_PLACEMENT_3D('',#44481,#31750,#31751);
#26458=AXIS2_PLACEMENT_3D('',#44487,#31753,#31754);
#26459=AXIS2_PLACEMENT_3D('',#44490,#31755,#31756);
#26460=AXIS2_PLACEMENT_3D('',#44494,#31759,#31760);
#26461=AXIS2_PLACEMENT_3D('',#44502,#31763,#31764);
#26462=AXIS2_PLACEMENT_3D('',#44508,#31766,#31767);
#26463=AXIS2_PLACEMENT_3D('',#44509,#31768,#31769);
#26464=AXIS2_PLACEMENT_3D('',#44510,#31770,#31771);
#26465=AXIS2_PLACEMENT_3D('',#44511,#31772,#31773);
#26466=AXIS2_PLACEMENT_3D('',#44512,#31774,#31775);
#26467=AXIS2_PLACEMENT_3D('',#44513,#31776,#31777);
#26468=AXIS2_PLACEMENT_3D('',#44514,#31778,#31779);
#26469=AXIS2_PLACEMENT_3D('',#44515,#31780,#31781);
#26470=AXIS2_PLACEMENT_3D('',#44516,#31782,#31783);
#26471=AXIS2_PLACEMENT_3D('',#44517,#31784,#31785);
#26472=AXIS2_PLACEMENT_3D('',#44518,#31786,#31787);
#26473=AXIS2_PLACEMENT_3D('',#44519,#31788,#31789);
#26474=AXIS2_PLACEMENT_3D('',#44520,#31790,#31791);
#26475=AXIS2_PLACEMENT_3D('',#44521,#31792,#31793);
#26476=AXIS2_PLACEMENT_3D('',#44522,#31794,#31795);
#26477=AXIS2_PLACEMENT_3D('',#44523,#31796,#31797);
#26478=AXIS2_PLACEMENT_3D('',#44524,#31798,#31799);
#26479=AXIS2_PLACEMENT_3D('',#44525,#31800,#31801);
#26480=AXIS2_PLACEMENT_3D('',#44528,#31803,#31804);
#26481=AXIS2_PLACEMENT_3D('',#44529,#31805,#31806);
#26482=AXIS2_PLACEMENT_3D('',#44530,#31807,#31808);
#26483=AXIS2_PLACEMENT_3D('',#44531,#31809,#31810);
#26484=AXIS2_PLACEMENT_3D('',#44532,#31811,#31812);
#26485=AXIS2_PLACEMENT_3D('',#44533,#31813,#31814);
#26486=AXIS2_PLACEMENT_3D('',#44534,#31815,#31816);
#26487=AXIS2_PLACEMENT_3D('',#44535,#31817,#31818);
#26488=AXIS2_PLACEMENT_3D('',#44536,#31819,#31820);
#26489=AXIS2_PLACEMENT_3D('',#44537,#31821,#31822);
#26490=AXIS2_PLACEMENT_3D('',#44538,#31823,#31824);
#26491=AXIS2_PLACEMENT_3D('',#44539,#31825,#31826);
#26492=AXIS2_PLACEMENT_3D('',#44540,#31827,#31828);
#26493=AXIS2_PLACEMENT_3D('',#44541,#31829,#31830);
#26494=AXIS2_PLACEMENT_3D('',#44542,#31831,#31832);
#26495=AXIS2_PLACEMENT_3D('',#44543,#31833,#31834);
#26496=AXIS2_PLACEMENT_3D('',#44544,#31835,#31836);
#26497=AXIS2_PLACEMENT_3D('',#44545,#31837,#31838);
#26498=AXIS2_PLACEMENT_3D('',#44547,#31839,#31840);
#26499=AXIS2_PLACEMENT_3D('',#44551,#31842,#31843);
#26500=AXIS2_PLACEMENT_3D('',#44554,#31845,#31846);
#26501=AXIS2_PLACEMENT_3D('',#44555,#31847,#31848);
#26502=AXIS2_PLACEMENT_3D('',#44563,#31851,#31852);
#26503=AXIS2_PLACEMENT_3D('',#44568,#31854,#31855);
#26504=AXIS2_PLACEMENT_3D('',#44569,#31856,#31857);
#26505=AXIS2_PLACEMENT_3D('',#44571,#31858,#31859);
#26506=AXIS2_PLACEMENT_3D('',#44573,#31861,#31862);
#26507=AXIS2_PLACEMENT_3D('',#44577,#31864,#31865);
#26508=AXIS2_PLACEMENT_3D('',#44578,#31866,#31867);
#26509=AXIS2_PLACEMENT_3D('',#44587,#31872,#31873);
#26510=AXIS2_PLACEMENT_3D('',#44593,#31877,#31878);
#26511=AXIS2_PLACEMENT_3D('',#44599,#31882,#31883);
#26512=AXIS2_PLACEMENT_3D('',#44605,#31887,#31888);
#26513=AXIS2_PLACEMENT_3D('',#44611,#31892,#31893);
#26514=AXIS2_PLACEMENT_3D('',#44614,#31896,#31897);
#26515=AXIS2_PLACEMENT_3D('',#44615,#31898,#31899);
#26516=AXIS2_PLACEMENT_3D('',#44617,#31900,#31901);
#26517=AXIS2_PLACEMENT_3D('',#44618,#31902,#31903);
#26518=AXIS2_PLACEMENT_3D('',#44620,#31905,#31906);
#26519=AXIS2_PLACEMENT_3D('',#44621,#31907,#31908);
#26520=AXIS2_PLACEMENT_3D('',#44622,#31909,#31910);
#26521=AXIS2_PLACEMENT_3D('',#44624,#31911,#31912);
#26522=AXIS2_PLACEMENT_3D('',#44626,#31914,#31915);
#26523=AXIS2_PLACEMENT_3D('',#44627,#31916,#31917);
#26524=AXIS2_PLACEMENT_3D('',#44628,#31918,#31919);
#26525=AXIS2_PLACEMENT_3D('',#44629,#31920,#31921);
#26526=AXIS2_PLACEMENT_3D('',#44648,#31923,#31924);
#26527=AXIS2_PLACEMENT_3D('',#44651,#31926,#31927);
#26528=AXIS2_PLACEMENT_3D('',#44653,#31928,#31929);
#26529=AXIS2_PLACEMENT_3D('',#44664,#31930,#31931);
#26530=AXIS2_PLACEMENT_3D('',#44718,#31933,#31934);
#26531=AXIS2_PLACEMENT_3D('',#44766,#31936,#31937);
#26532=AXIS2_PLACEMENT_3D('',#44814,#31939,#31940);
#26533=AXIS2_PLACEMENT_3D('',#44862,#31942,#31943);
#26534=AXIS2_PLACEMENT_3D('',#44916,#31945,#31946);
#26535=AXIS2_PLACEMENT_3D('',#44964,#31948,#31949);
#26536=AXIS2_PLACEMENT_3D('',#45012,#31951,#31952);
#26537=AXIS2_PLACEMENT_3D('',#45066,#31954,#31955);
#26538=AXIS2_PLACEMENT_3D('',#45114,#31957,#31958);
#26539=AXIS2_PLACEMENT_3D('',#45162,#31960,#31961);
#26540=AXIS2_PLACEMENT_3D('',#45216,#31963,#31964);
#26541=AXIS2_PLACEMENT_3D('',#45264,#31966,#31967);
#26542=AXIS2_PLACEMENT_3D('',#45312,#31969,#31970);
#26543=AXIS2_PLACEMENT_3D('',#45366,#31972,#31973);
#26544=AXIS2_PLACEMENT_3D('',#45414,#31975,#31976);
#26545=AXIS2_PLACEMENT_3D('',#45462,#31978,#31979);
#26546=AXIS2_PLACEMENT_3D('',#45516,#31981,#31982);
#26547=AXIS2_PLACEMENT_3D('',#45564,#31984,#31985);
#26548=AXIS2_PLACEMENT_3D('',#45612,#31987,#31988);
#26549=AXIS2_PLACEMENT_3D('',#45666,#31990,#31991);
#26550=AXIS2_PLACEMENT_3D('',#45714,#31993,#31994);
#26551=AXIS2_PLACEMENT_3D('',#45762,#31996,#31997);
#26552=AXIS2_PLACEMENT_3D('',#45775,#31999,#32000);
#26553=AXIS2_PLACEMENT_3D('',#45781,#32001,#32002);
#26554=AXIS2_PLACEMENT_3D('',#45806,#32004,#32005);
#26555=AXIS2_PLACEMENT_3D('',#45830,#32007,#32008);
#26556=AXIS2_PLACEMENT_3D('',#45855,#32010,#32011);
#26557=AXIS2_PLACEMENT_3D('',#45880,#32013,#32014);
#26558=AXIS2_PLACEMENT_3D('',#45904,#32016,#32017);
#26559=AXIS2_PLACEMENT_3D('',#45929,#32019,#32020);
#26560=AXIS2_PLACEMENT_3D('',#45954,#32022,#32023);
#26561=AXIS2_PLACEMENT_3D('',#45978,#32025,#32026);
#26562=AXIS2_PLACEMENT_3D('',#46003,#32028,#32029);
#26563=AXIS2_PLACEMENT_3D('',#46028,#32031,#32032);
#26564=AXIS2_PLACEMENT_3D('',#46052,#32034,#32035);
#26565=AXIS2_PLACEMENT_3D('',#46077,#32037,#32038);
#26566=AXIS2_PLACEMENT_3D('',#46102,#32040,#32041);
#26567=AXIS2_PLACEMENT_3D('',#46126,#32043,#32044);
#26568=AXIS2_PLACEMENT_3D('',#46151,#32046,#32047);
#26569=AXIS2_PLACEMENT_3D('',#46176,#32049,#32050);
#26570=AXIS2_PLACEMENT_3D('',#46200,#32052,#32053);
#26571=AXIS2_PLACEMENT_3D('',#46225,#32055,#32056);
#26572=AXIS2_PLACEMENT_3D('',#46250,#32058,#32059);
#26573=AXIS2_PLACEMENT_3D('',#46274,#32061,#32062);
#26574=AXIS2_PLACEMENT_3D('',#46298,#32064,#32065);
#26575=AXIS2_PLACEMENT_3D('',#46323,#32067,#32068);
#26576=AXIS2_PLACEMENT_3D('',#46328,#32070,#32071);
#26577=AXIS2_PLACEMENT_3D('',#46349,#32072,#32073);
#26578=AXIS2_PLACEMENT_3D('',#46398,#32074,#32075);
#26579=AXIS2_PLACEMENT_3D('',#46400,#32076,#32077);
#26580=AXIS2_PLACEMENT_3D('',#47132,#32078,#32079);
#26581=AXIS2_PLACEMENT_3D('',#47179,#32080,#32081);
#26582=AXIS2_PLACEMENT_3D('',#47180,#32082,#32083);
#26583=AXIS2_PLACEMENT_3D('',#47812,#32084,#32085);
#26584=AXIS2_PLACEMENT_3D('',#47815,#32086,#32087);
#26585=AXIS2_PLACEMENT_3D('',#47819,#32090,#32091);
#26586=AXIS2_PLACEMENT_3D('',#47827,#32094,#32095);
#26587=AXIS2_PLACEMENT_3D('',#47833,#32097,#32098);
#26588=AXIS2_PLACEMENT_3D('',#47836,#32099,#32100);
#26589=AXIS2_PLACEMENT_3D('',#47840,#32103,#32104);
#26590=AXIS2_PLACEMENT_3D('',#47848,#32107,#32108);
#26591=AXIS2_PLACEMENT_3D('',#47854,#32110,#32111);
#26592=AXIS2_PLACEMENT_3D('',#47857,#32112,#32113);
#26593=AXIS2_PLACEMENT_3D('',#47861,#32116,#32117);
#26594=AXIS2_PLACEMENT_3D('',#47869,#32120,#32121);
#26595=AXIS2_PLACEMENT_3D('',#47875,#32123,#32124);
#26596=AXIS2_PLACEMENT_3D('',#47878,#32125,#32126);
#26597=AXIS2_PLACEMENT_3D('',#47882,#32129,#32130);
#26598=AXIS2_PLACEMENT_3D('',#47890,#32133,#32134);
#26599=AXIS2_PLACEMENT_3D('',#47896,#32136,#32137);
#26600=AXIS2_PLACEMENT_3D('',#47899,#32138,#32139);
#26601=AXIS2_PLACEMENT_3D('',#47903,#32142,#32143);
#26602=AXIS2_PLACEMENT_3D('',#47911,#32146,#32147);
#26603=AXIS2_PLACEMENT_3D('',#47917,#32149,#32150);
#26604=AXIS2_PLACEMENT_3D('',#47920,#32151,#32152);
#26605=AXIS2_PLACEMENT_3D('',#47924,#32155,#32156);
#26606=AXIS2_PLACEMENT_3D('',#47932,#32159,#32160);
#26607=AXIS2_PLACEMENT_3D('',#47938,#32162,#32163);
#26608=AXIS2_PLACEMENT_3D('',#47941,#32164,#32165);
#26609=AXIS2_PLACEMENT_3D('',#47945,#32168,#32169);
#26610=AXIS2_PLACEMENT_3D('',#47953,#32172,#32173);
#26611=AXIS2_PLACEMENT_3D('',#47959,#32175,#32176);
#26612=AXIS2_PLACEMENT_3D('',#47962,#32177,#32178);
#26613=AXIS2_PLACEMENT_3D('',#47966,#32181,#32182);
#26614=AXIS2_PLACEMENT_3D('',#47974,#32185,#32186);
#26615=AXIS2_PLACEMENT_3D('',#47980,#32188,#32189);
#26616=AXIS2_PLACEMENT_3D('',#47983,#32190,#32191);
#26617=AXIS2_PLACEMENT_3D('',#47987,#32194,#32195);
#26618=AXIS2_PLACEMENT_3D('',#47995,#32198,#32199);
#26619=AXIS2_PLACEMENT_3D('',#48001,#32201,#32202);
#26620=AXIS2_PLACEMENT_3D('',#48004,#32203,#32204);
#26621=AXIS2_PLACEMENT_3D('',#48008,#32207,#32208);
#26622=AXIS2_PLACEMENT_3D('',#48016,#32211,#32212);
#26623=AXIS2_PLACEMENT_3D('',#48022,#32214,#32215);
#26624=AXIS2_PLACEMENT_3D('',#48025,#32216,#32217);
#26625=AXIS2_PLACEMENT_3D('',#48029,#32220,#32221);
#26626=AXIS2_PLACEMENT_3D('',#48037,#32224,#32225);
#26627=AXIS2_PLACEMENT_3D('',#48043,#32227,#32228);
#26628=AXIS2_PLACEMENT_3D('',#48046,#32229,#32230);
#26629=AXIS2_PLACEMENT_3D('',#48050,#32233,#32234);
#26630=AXIS2_PLACEMENT_3D('',#48058,#32237,#32238);
#26631=AXIS2_PLACEMENT_3D('',#48064,#32240,#32241);
#26632=AXIS2_PLACEMENT_3D('',#48067,#32242,#32243);
#26633=AXIS2_PLACEMENT_3D('',#48071,#32246,#32247);
#26634=AXIS2_PLACEMENT_3D('',#48079,#32250,#32251);
#26635=AXIS2_PLACEMENT_3D('',#48085,#32253,#32254);
#26636=AXIS2_PLACEMENT_3D('',#48088,#32255,#32256);
#26637=AXIS2_PLACEMENT_3D('',#48092,#32259,#32260);
#26638=AXIS2_PLACEMENT_3D('',#48100,#32263,#32264);
#26639=AXIS2_PLACEMENT_3D('',#48106,#32266,#32267);
#26640=AXIS2_PLACEMENT_3D('',#48109,#32268,#32269);
#26641=AXIS2_PLACEMENT_3D('',#48113,#32272,#32273);
#26642=AXIS2_PLACEMENT_3D('',#48121,#32276,#32277);
#26643=AXIS2_PLACEMENT_3D('',#48127,#32279,#32280);
#26644=AXIS2_PLACEMENT_3D('',#48130,#32281,#32282);
#26645=AXIS2_PLACEMENT_3D('',#48134,#32285,#32286);
#26646=AXIS2_PLACEMENT_3D('',#48142,#32289,#32290);
#26647=AXIS2_PLACEMENT_3D('',#48148,#32292,#32293);
#26648=AXIS2_PLACEMENT_3D('',#48151,#32294,#32295);
#26649=AXIS2_PLACEMENT_3D('',#48155,#32298,#32299);
#26650=AXIS2_PLACEMENT_3D('',#48163,#32302,#32303);
#26651=AXIS2_PLACEMENT_3D('',#48169,#32305,#32306);
#26652=AXIS2_PLACEMENT_3D('',#48172,#32307,#32308);
#26653=AXIS2_PLACEMENT_3D('',#48177,#32311,#32312);
#26654=AXIS2_PLACEMENT_3D('',#48178,#32313,#32314);
#26655=AXIS2_PLACEMENT_3D('',#48186,#32317,#32318);
#26656=AXIS2_PLACEMENT_3D('',#48192,#32320,#32321);
#26657=AXIS2_PLACEMENT_3D('',#48195,#32322,#32323);
#26658=AXIS2_PLACEMENT_3D('',#48199,#32326,#32327);
#26659=AXIS2_PLACEMENT_3D('',#48207,#32330,#32331);
#26660=AXIS2_PLACEMENT_3D('',#48213,#32333,#32334);
#26661=AXIS2_PLACEMENT_3D('',#48216,#32335,#32336);
#26662=AXIS2_PLACEMENT_3D('',#48220,#32339,#32340);
#26663=AXIS2_PLACEMENT_3D('',#48228,#32343,#32344);
#26664=AXIS2_PLACEMENT_3D('',#48234,#32346,#32347);
#26665=AXIS2_PLACEMENT_3D('',#48237,#32348,#32349);
#26666=AXIS2_PLACEMENT_3D('',#48241,#32352,#32353);
#26667=AXIS2_PLACEMENT_3D('',#48249,#32356,#32357);
#26668=AXIS2_PLACEMENT_3D('',#48255,#32359,#32360);
#26669=AXIS2_PLACEMENT_3D('',#48258,#32361,#32362);
#26670=AXIS2_PLACEMENT_3D('',#48262,#32365,#32366);
#26671=AXIS2_PLACEMENT_3D('',#48270,#32369,#32370);
#26672=AXIS2_PLACEMENT_3D('',#48276,#32372,#32373);
#26673=AXIS2_PLACEMENT_3D('',#48279,#32374,#32375);
#26674=AXIS2_PLACEMENT_3D('',#48283,#32378,#32379);
#26675=AXIS2_PLACEMENT_3D('',#48291,#32382,#32383);
#26676=AXIS2_PLACEMENT_3D('',#48297,#32385,#32386);
#26677=AXIS2_PLACEMENT_3D('',#48300,#32387,#32388);
#26678=AXIS2_PLACEMENT_3D('',#48304,#32391,#32392);
#26679=AXIS2_PLACEMENT_3D('',#48312,#32395,#32396);
#26680=AXIS2_PLACEMENT_3D('',#48318,#32398,#32399);
#26681=AXIS2_PLACEMENT_3D('',#48321,#32400,#32401);
#26682=AXIS2_PLACEMENT_3D('',#48325,#32404,#32405);
#26683=AXIS2_PLACEMENT_3D('',#48333,#32408,#32409);
#26684=AXIS2_PLACEMENT_3D('',#48339,#32411,#32412);
#26685=AXIS2_PLACEMENT_3D('',#48342,#32413,#32414);
#26686=AXIS2_PLACEMENT_3D('',#48346,#32417,#32418);
#26687=AXIS2_PLACEMENT_3D('',#48354,#32421,#32422);
#26688=AXIS2_PLACEMENT_3D('',#48360,#32424,#32425);
#26689=AXIS2_PLACEMENT_3D('',#48363,#32426,#32427);
#26690=AXIS2_PLACEMENT_3D('',#48367,#32430,#32431);
#26691=AXIS2_PLACEMENT_3D('',#48375,#32434,#32435);
#26692=AXIS2_PLACEMENT_3D('',#48381,#32437,#32438);
#26693=AXIS2_PLACEMENT_3D('',#48384,#32439,#32440);
#26694=AXIS2_PLACEMENT_3D('',#48388,#32443,#32444);
#26695=AXIS2_PLACEMENT_3D('',#48396,#32447,#32448);
#26696=AXIS2_PLACEMENT_3D('',#48402,#32450,#32451);
#26697=AXIS2_PLACEMENT_3D('',#48405,#32452,#32453);
#26698=AXIS2_PLACEMENT_3D('',#48409,#32456,#32457);
#26699=AXIS2_PLACEMENT_3D('',#48417,#32460,#32461);
#26700=AXIS2_PLACEMENT_3D('',#48423,#32463,#32464);
#26701=AXIS2_PLACEMENT_3D('',#48426,#32465,#32466);
#26702=AXIS2_PLACEMENT_3D('',#48430,#32469,#32470);
#26703=AXIS2_PLACEMENT_3D('',#48438,#32473,#32474);
#26704=AXIS2_PLACEMENT_3D('',#48444,#32476,#32477);
#26705=AXIS2_PLACEMENT_3D('',#48447,#32478,#32479);
#26706=AXIS2_PLACEMENT_3D('',#48451,#32482,#32483);
#26707=AXIS2_PLACEMENT_3D('',#48459,#32486,#32487);
#26708=AXIS2_PLACEMENT_3D('',#48465,#32489,#32490);
#26709=AXIS2_PLACEMENT_3D('',#48468,#32491,#32492);
#26710=AXIS2_PLACEMENT_3D('',#48472,#32495,#32496);
#26711=AXIS2_PLACEMENT_3D('',#48480,#32499,#32500);
#26712=AXIS2_PLACEMENT_3D('',#48486,#32502,#32503);
#26713=AXIS2_PLACEMENT_3D('',#48489,#32504,#32505);
#26714=AXIS2_PLACEMENT_3D('',#48493,#32508,#32509);
#26715=AXIS2_PLACEMENT_3D('',#48501,#32512,#32513);
#26716=AXIS2_PLACEMENT_3D('',#48507,#32515,#32516);
#26717=AXIS2_PLACEMENT_3D('',#48510,#32517,#32518);
#26718=AXIS2_PLACEMENT_3D('',#48514,#32521,#32522);
#26719=AXIS2_PLACEMENT_3D('',#48522,#32525,#32526);
#26720=AXIS2_PLACEMENT_3D('',#48528,#32528,#32529);
#26721=AXIS2_PLACEMENT_3D('',#48531,#32530,#32531);
#26722=AXIS2_PLACEMENT_3D('',#48535,#32534,#32535);
#26723=AXIS2_PLACEMENT_3D('',#48543,#32538,#32539);
#26724=AXIS2_PLACEMENT_3D('',#48549,#32541,#32542);
#26725=AXIS2_PLACEMENT_3D('',#48550,#32543,#32544);
#26726=AXIS2_PLACEMENT_3D('',#48551,#32545,#32546);
#26727=AXIS2_PLACEMENT_3D('',#48552,#32547,#32548);
#26728=AXIS2_PLACEMENT_3D('',#48553,#32549,#32550);
#26729=AXIS2_PLACEMENT_3D('',#48554,#32551,#32552);
#26730=AXIS2_PLACEMENT_3D('',#48555,#32553,#32554);
#26731=AXIS2_PLACEMENT_3D('',#48556,#32555,#32556);
#26732=AXIS2_PLACEMENT_3D('',#48557,#32557,#32558);
#26733=AXIS2_PLACEMENT_3D('',#48558,#32559,#32560);
#26734=AXIS2_PLACEMENT_3D('',#48559,#32561,#32562);
#26735=AXIS2_PLACEMENT_3D('',#48560,#32563,#32564);
#26736=AXIS2_PLACEMENT_3D('',#48561,#32565,#32566);
#26737=AXIS2_PLACEMENT_3D('',#48562,#32567,#32568);
#26738=AXIS2_PLACEMENT_3D('',#48563,#32569,#32570);
#26739=AXIS2_PLACEMENT_3D('',#48564,#32571,#32572);
#26740=AXIS2_PLACEMENT_3D('',#48565,#32573,#32574);
#26741=AXIS2_PLACEMENT_3D('',#48566,#32575,#32576);
#26742=AXIS2_PLACEMENT_3D('',#48569,#32578,#32579);
#26743=AXIS2_PLACEMENT_3D('',#48570,#32580,#32581);
#26744=AXIS2_PLACEMENT_3D('',#48571,#32582,#32583);
#26745=AXIS2_PLACEMENT_3D('',#48572,#32584,#32585);
#26746=AXIS2_PLACEMENT_3D('',#48573,#32586,#32587);
#26747=AXIS2_PLACEMENT_3D('',#48574,#32588,#32589);
#26748=AXIS2_PLACEMENT_3D('',#48575,#32590,#32591);
#26749=AXIS2_PLACEMENT_3D('',#48576,#32592,#32593);
#26750=AXIS2_PLACEMENT_3D('',#48577,#32594,#32595);
#26751=AXIS2_PLACEMENT_3D('',#48578,#32596,#32597);
#26752=AXIS2_PLACEMENT_3D('',#48579,#32598,#32599);
#26753=AXIS2_PLACEMENT_3D('',#48580,#32600,#32601);
#26754=AXIS2_PLACEMENT_3D('',#48581,#32602,#32603);
#26755=AXIS2_PLACEMENT_3D('',#48582,#32604,#32605);
#26756=AXIS2_PLACEMENT_3D('',#48583,#32606,#32607);
#26757=AXIS2_PLACEMENT_3D('',#48584,#32608,#32609);
#26758=AXIS2_PLACEMENT_3D('',#48585,#32610,#32611);
#26759=AXIS2_PLACEMENT_3D('',#48586,#32612,#32613);
#26760=AXIS2_PLACEMENT_3D('',#48588,#32614,#32615);
#26761=AXIS2_PLACEMENT_3D('',#48592,#32617,#32618);
#26762=AXIS2_PLACEMENT_3D('',#48595,#32620,#32621);
#26763=AXIS2_PLACEMENT_3D('',#48596,#32622,#32623);
#26764=AXIS2_PLACEMENT_3D('',#48604,#32626,#32627);
#26765=AXIS2_PLACEMENT_3D('',#48609,#32629,#32630);
#26766=AXIS2_PLACEMENT_3D('',#48610,#32631,#32632);
#26767=AXIS2_PLACEMENT_3D('',#48612,#32633,#32634);
#26768=AXIS2_PLACEMENT_3D('',#48614,#32636,#32637);
#26769=AXIS2_PLACEMENT_3D('',#48618,#32639,#32640);
#26770=AXIS2_PLACEMENT_3D('',#48619,#32641,#32642);
#26771=AXIS2_PLACEMENT_3D('',#48628,#32647,#32648);
#26772=AXIS2_PLACEMENT_3D('',#48634,#32652,#32653);
#26773=AXIS2_PLACEMENT_3D('',#48640,#32657,#32658);
#26774=AXIS2_PLACEMENT_3D('',#48646,#32662,#32663);
#26775=AXIS2_PLACEMENT_3D('',#48652,#32667,#32668);
#26776=AXIS2_PLACEMENT_3D('',#48655,#32671,#32672);
#26777=AXIS2_PLACEMENT_3D('',#48656,#32673,#32674);
#26778=AXIS2_PLACEMENT_3D('',#48658,#32675,#32676);
#26779=AXIS2_PLACEMENT_3D('',#48659,#32677,#32678);
#26780=AXIS2_PLACEMENT_3D('',#48661,#32680,#32681);
#26781=AXIS2_PLACEMENT_3D('',#48662,#32682,#32683);
#26782=AXIS2_PLACEMENT_3D('',#48663,#32684,#32685);
#26783=AXIS2_PLACEMENT_3D('',#48665,#32686,#32687);
#26784=AXIS2_PLACEMENT_3D('',#48667,#32689,#32690);
#26785=AXIS2_PLACEMENT_3D('',#48668,#32691,#32692);
#26786=AXIS2_PLACEMENT_3D('',#48669,#32693,#32694);
#26787=AXIS2_PLACEMENT_3D('',#48670,#32695,#32696);
#26788=AXIS2_PLACEMENT_3D('',#48692,#32698,#32699);
#26789=AXIS2_PLACEMENT_3D('',#48695,#32701,#32702);
#26790=AXIS2_PLACEMENT_3D('',#48697,#32703,#32704);
#26791=AXIS2_PLACEMENT_3D('',#48711,#32705,#32706);
#26792=AXIS2_PLACEMENT_3D('',#48759,#32708,#32709);
#26793=AXIS2_PLACEMENT_3D('',#48807,#32711,#32712);
#26794=AXIS2_PLACEMENT_3D('',#48861,#32714,#32715);
#26795=AXIS2_PLACEMENT_3D('',#48909,#32717,#32718);
#26796=AXIS2_PLACEMENT_3D('',#48963,#32720,#32721);
#26797=AXIS2_PLACEMENT_3D('',#49011,#32723,#32724);
#26798=AXIS2_PLACEMENT_3D('',#49059,#32726,#32727);
#26799=AXIS2_PLACEMENT_3D('',#49113,#32729,#32730);
#26800=AXIS2_PLACEMENT_3D('',#49161,#32732,#32733);
#26801=AXIS2_PLACEMENT_3D('',#49209,#32735,#32736);
#26802=AXIS2_PLACEMENT_3D('',#49263,#32738,#32739);
#26803=AXIS2_PLACEMENT_3D('',#49278,#32741,#32742);
#26804=AXIS2_PLACEMENT_3D('',#49286,#32743,#32744);
#26805=AXIS2_PLACEMENT_3D('',#49311,#32746,#32747);
#26806=AXIS2_PLACEMENT_3D('',#49335,#32749,#32750);
#26807=AXIS2_PLACEMENT_3D('',#49360,#32752,#32753);
#26808=AXIS2_PLACEMENT_3D('',#49385,#32755,#32756);
#26809=AXIS2_PLACEMENT_3D('',#49409,#32758,#32759);
#26810=AXIS2_PLACEMENT_3D('',#49434,#32761,#32762);
#26811=AXIS2_PLACEMENT_3D('',#49459,#32764,#32765);
#26812=AXIS2_PLACEMENT_3D('',#49484,#32767,#32768);
#26813=AXIS2_PLACEMENT_3D('',#49509,#32770,#32771);
#26814=AXIS2_PLACEMENT_3D('',#49533,#32773,#32774);
#26815=AXIS2_PLACEMENT_3D('',#49538,#32776,#32777);
#26816=AXIS2_PLACEMENT_3D('',#49559,#32778,#32779);
#26817=AXIS2_PLACEMENT_3D('',#49611,#32780,#32781);
#26818=AXIS2_PLACEMENT_3D('',#49613,#32782,#32783);
#26819=AXIS2_PLACEMENT_3D('',#50045,#32784,#32785);
#26820=AXIS2_PLACEMENT_3D('',#50095,#32786,#32787);
#26821=AXIS2_PLACEMENT_3D('',#50096,#32788,#32789);
#26822=AXIS2_PLACEMENT_3D('',#50421,#32790,#32791);
#26823=AXIS2_PLACEMENT_3D('',#50422,#32792,#32793);
#26824=AXIS2_PLACEMENT_3D('',#50423,#32794,#32795);
#26825=AXIS2_PLACEMENT_3D('',#50426,#32796,#32797);
#26826=AXIS2_PLACEMENT_3D('',#50430,#32800,#32801);
#26827=AXIS2_PLACEMENT_3D('',#50438,#32804,#32805);
#26828=AXIS2_PLACEMENT_3D('',#50444,#32807,#32808);
#26829=AXIS2_PLACEMENT_3D('',#50447,#32809,#32810);
#26830=AXIS2_PLACEMENT_3D('',#50451,#32813,#32814);
#26831=AXIS2_PLACEMENT_3D('',#50459,#32817,#32818);
#26832=AXIS2_PLACEMENT_3D('',#50465,#32820,#32821);
#26833=AXIS2_PLACEMENT_3D('',#50468,#32822,#32823);
#26834=AXIS2_PLACEMENT_3D('',#50472,#32826,#32827);
#26835=AXIS2_PLACEMENT_3D('',#50480,#32830,#32831);
#26836=AXIS2_PLACEMENT_3D('',#50486,#32833,#32834);
#26837=AXIS2_PLACEMENT_3D('',#50489,#32835,#32836);
#26838=AXIS2_PLACEMENT_3D('',#50493,#32839,#32840);
#26839=AXIS2_PLACEMENT_3D('',#50501,#32843,#32844);
#26840=AXIS2_PLACEMENT_3D('',#50507,#32846,#32847);
#26841=AXIS2_PLACEMENT_3D('',#50510,#32848,#32849);
#26842=AXIS2_PLACEMENT_3D('',#50514,#32852,#32853);
#26843=AXIS2_PLACEMENT_3D('',#50522,#32856,#32857);
#26844=AXIS2_PLACEMENT_3D('',#50528,#32859,#32860);
#26845=AXIS2_PLACEMENT_3D('',#50531,#32861,#32862);
#26846=AXIS2_PLACEMENT_3D('',#50535,#32865,#32866);
#26847=AXIS2_PLACEMENT_3D('',#50543,#32869,#32870);
#26848=AXIS2_PLACEMENT_3D('',#50549,#32872,#32873);
#26849=AXIS2_PLACEMENT_3D('',#50552,#32874,#32875);
#26850=AXIS2_PLACEMENT_3D('',#50556,#32878,#32879);
#26851=AXIS2_PLACEMENT_3D('',#50564,#32882,#32883);
#26852=AXIS2_PLACEMENT_3D('',#50570,#32885,#32886);
#26853=AXIS2_PLACEMENT_3D('',#50573,#32887,#32888);
#26854=AXIS2_PLACEMENT_3D('',#50577,#32891,#32892);
#26855=AXIS2_PLACEMENT_3D('',#50585,#32895,#32896);
#26856=AXIS2_PLACEMENT_3D('',#50591,#32898,#32899);
#26857=AXIS2_PLACEMENT_3D('',#50594,#32900,#32901);
#26858=AXIS2_PLACEMENT_3D('',#50598,#32904,#32905);
#26859=AXIS2_PLACEMENT_3D('',#50606,#32908,#32909);
#26860=AXIS2_PLACEMENT_3D('',#50612,#32911,#32912);
#26861=AXIS2_PLACEMENT_3D('',#50615,#32913,#32914);
#26862=AXIS2_PLACEMENT_3D('',#50619,#32917,#32918);
#26863=AXIS2_PLACEMENT_3D('',#50627,#32921,#32922);
#26864=AXIS2_PLACEMENT_3D('',#50633,#32924,#32925);
#26865=AXIS2_PLACEMENT_3D('',#50636,#32926,#32927);
#26866=AXIS2_PLACEMENT_3D('',#50640,#32930,#32931);
#26867=AXIS2_PLACEMENT_3D('',#50648,#32934,#32935);
#26868=AXIS2_PLACEMENT_3D('',#50654,#32937,#32938);
#26869=AXIS2_PLACEMENT_3D('',#50657,#32939,#32940);
#26870=AXIS2_PLACEMENT_3D('',#50661,#32943,#32944);
#26871=AXIS2_PLACEMENT_3D('',#50669,#32947,#32948);
#26872=AXIS2_PLACEMENT_3D('',#50675,#32950,#32951);
#26873=AXIS2_PLACEMENT_3D('',#50678,#32952,#32953);
#26874=AXIS2_PLACEMENT_3D('',#50682,#32956,#32957);
#26875=AXIS2_PLACEMENT_3D('',#50690,#32960,#32961);
#26876=AXIS2_PLACEMENT_3D('',#50696,#32963,#32964);
#26877=AXIS2_PLACEMENT_3D('',#50699,#32965,#32966);
#26878=AXIS2_PLACEMENT_3D('',#50703,#32969,#32970);
#26879=AXIS2_PLACEMENT_3D('',#50711,#32973,#32974);
#26880=AXIS2_PLACEMENT_3D('',#50717,#32976,#32977);
#26881=AXIS2_PLACEMENT_3D('',#50720,#32978,#32979);
#26882=AXIS2_PLACEMENT_3D('',#50724,#32982,#32983);
#26883=AXIS2_PLACEMENT_3D('',#50732,#32986,#32987);
#26884=AXIS2_PLACEMENT_3D('',#50738,#32989,#32990);
#26885=AXIS2_PLACEMENT_3D('',#50741,#32991,#32992);
#26886=AXIS2_PLACEMENT_3D('',#50745,#32995,#32996);
#26887=AXIS2_PLACEMENT_3D('',#50753,#32999,#33000);
#26888=AXIS2_PLACEMENT_3D('',#50759,#33002,#33003);
#26889=AXIS2_PLACEMENT_3D('',#50762,#33004,#33005);
#26890=AXIS2_PLACEMENT_3D('',#50766,#33008,#33009);
#26891=AXIS2_PLACEMENT_3D('',#50774,#33012,#33013);
#26892=AXIS2_PLACEMENT_3D('',#50780,#33015,#33016);
#26893=AXIS2_PLACEMENT_3D('',#50783,#33017,#33018);
#26894=AXIS2_PLACEMENT_3D('',#50788,#33021,#33022);
#26895=AXIS2_PLACEMENT_3D('',#50789,#33023,#33024);
#26896=AXIS2_PLACEMENT_3D('',#50797,#33027,#33028);
#26897=AXIS2_PLACEMENT_3D('',#50803,#33030,#33031);
#26898=AXIS2_PLACEMENT_3D('',#50806,#33032,#33033);
#26899=AXIS2_PLACEMENT_3D('',#50810,#33036,#33037);
#26900=AXIS2_PLACEMENT_3D('',#50818,#33040,#33041);
#26901=AXIS2_PLACEMENT_3D('',#50824,#33043,#33044);
#26902=AXIS2_PLACEMENT_3D('',#50827,#33045,#33046);
#26903=AXIS2_PLACEMENT_3D('',#50831,#33049,#33050);
#26904=AXIS2_PLACEMENT_3D('',#50839,#33053,#33054);
#26905=AXIS2_PLACEMENT_3D('',#50845,#33056,#33057);
#26906=AXIS2_PLACEMENT_3D('',#50848,#33058,#33059);
#26907=AXIS2_PLACEMENT_3D('',#50852,#33062,#33063);
#26908=AXIS2_PLACEMENT_3D('',#50860,#33066,#33067);
#26909=AXIS2_PLACEMENT_3D('',#50866,#33069,#33070);
#26910=AXIS2_PLACEMENT_3D('',#50869,#33071,#33072);
#26911=AXIS2_PLACEMENT_3D('',#50873,#33075,#33076);
#26912=AXIS2_PLACEMENT_3D('',#50881,#33079,#33080);
#26913=AXIS2_PLACEMENT_3D('',#50887,#33082,#33083);
#26914=AXIS2_PLACEMENT_3D('',#50890,#33084,#33085);
#26915=AXIS2_PLACEMENT_3D('',#50894,#33088,#33089);
#26916=AXIS2_PLACEMENT_3D('',#50902,#33092,#33093);
#26917=AXIS2_PLACEMENT_3D('',#50908,#33095,#33096);
#26918=AXIS2_PLACEMENT_3D('',#50911,#33097,#33098);
#26919=AXIS2_PLACEMENT_3D('',#50915,#33101,#33102);
#26920=AXIS2_PLACEMENT_3D('',#50923,#33105,#33106);
#26921=AXIS2_PLACEMENT_3D('',#50929,#33108,#33109);
#26922=AXIS2_PLACEMENT_3D('',#50932,#33110,#33111);
#26923=AXIS2_PLACEMENT_3D('',#50936,#33114,#33115);
#26924=AXIS2_PLACEMENT_3D('',#50944,#33118,#33119);
#26925=AXIS2_PLACEMENT_3D('',#50950,#33121,#33122);
#26926=AXIS2_PLACEMENT_3D('',#50953,#33123,#33124);
#26927=AXIS2_PLACEMENT_3D('',#50957,#33127,#33128);
#26928=AXIS2_PLACEMENT_3D('',#50965,#33131,#33132);
#26929=AXIS2_PLACEMENT_3D('',#50971,#33134,#33135);
#26930=AXIS2_PLACEMENT_3D('',#50974,#33136,#33137);
#26931=AXIS2_PLACEMENT_3D('',#50978,#33140,#33141);
#26932=AXIS2_PLACEMENT_3D('',#50986,#33144,#33145);
#26933=AXIS2_PLACEMENT_3D('',#50992,#33147,#33148);
#26934=AXIS2_PLACEMENT_3D('',#50995,#33149,#33150);
#26935=AXIS2_PLACEMENT_3D('',#50999,#33153,#33154);
#26936=AXIS2_PLACEMENT_3D('',#51007,#33157,#33158);
#26937=AXIS2_PLACEMENT_3D('',#51013,#33160,#33161);
#26938=AXIS2_PLACEMENT_3D('',#51016,#33162,#33163);
#26939=AXIS2_PLACEMENT_3D('',#51020,#33166,#33167);
#26940=AXIS2_PLACEMENT_3D('',#51028,#33170,#33171);
#26941=AXIS2_PLACEMENT_3D('',#51034,#33173,#33174);
#26942=AXIS2_PLACEMENT_3D('',#51037,#33175,#33176);
#26943=AXIS2_PLACEMENT_3D('',#51041,#33179,#33180);
#26944=AXIS2_PLACEMENT_3D('',#51049,#33183,#33184);
#26945=AXIS2_PLACEMENT_3D('',#51055,#33186,#33187);
#26946=AXIS2_PLACEMENT_3D('',#51058,#33188,#33189);
#26947=AXIS2_PLACEMENT_3D('',#51062,#33192,#33193);
#26948=AXIS2_PLACEMENT_3D('',#51070,#33196,#33197);
#26949=AXIS2_PLACEMENT_3D('',#51076,#33199,#33200);
#26950=AXIS2_PLACEMENT_3D('',#51079,#33201,#33202);
#26951=AXIS2_PLACEMENT_3D('',#51083,#33205,#33206);
#26952=AXIS2_PLACEMENT_3D('',#51091,#33209,#33210);
#26953=AXIS2_PLACEMENT_3D('',#51097,#33212,#33213);
#26954=AXIS2_PLACEMENT_3D('',#51100,#33214,#33215);
#26955=AXIS2_PLACEMENT_3D('',#51104,#33218,#33219);
#26956=AXIS2_PLACEMENT_3D('',#51112,#33222,#33223);
#26957=AXIS2_PLACEMENT_3D('',#51118,#33225,#33226);
#26958=AXIS2_PLACEMENT_3D('',#51121,#33227,#33228);
#26959=AXIS2_PLACEMENT_3D('',#51125,#33231,#33232);
#26960=AXIS2_PLACEMENT_3D('',#51133,#33235,#33236);
#26961=AXIS2_PLACEMENT_3D('',#51139,#33238,#33239);
#26962=AXIS2_PLACEMENT_3D('',#51142,#33240,#33241);
#26963=AXIS2_PLACEMENT_3D('',#51146,#33244,#33245);
#26964=AXIS2_PLACEMENT_3D('',#51154,#33248,#33249);
#26965=AXIS2_PLACEMENT_3D('',#51160,#33251,#33252);
#26966=AXIS2_PLACEMENT_3D('',#51161,#33253,#33254);
#26967=AXIS2_PLACEMENT_3D('',#51162,#33255,#33256);
#26968=AXIS2_PLACEMENT_3D('',#51163,#33257,#33258);
#26969=AXIS2_PLACEMENT_3D('',#51164,#33259,#33260);
#26970=AXIS2_PLACEMENT_3D('',#51165,#33261,#33262);
#26971=AXIS2_PLACEMENT_3D('',#51166,#33263,#33264);
#26972=AXIS2_PLACEMENT_3D('',#51167,#33265,#33266);
#26973=AXIS2_PLACEMENT_3D('',#51168,#33267,#33268);
#26974=AXIS2_PLACEMENT_3D('',#51169,#33269,#33270);
#26975=AXIS2_PLACEMENT_3D('',#51170,#33271,#33272);
#26976=AXIS2_PLACEMENT_3D('',#51171,#33273,#33274);
#26977=AXIS2_PLACEMENT_3D('',#51172,#33275,#33276);
#26978=AXIS2_PLACEMENT_3D('',#51173,#33277,#33278);
#26979=AXIS2_PLACEMENT_3D('',#51174,#33279,#33280);
#26980=AXIS2_PLACEMENT_3D('',#51175,#33281,#33282);
#26981=AXIS2_PLACEMENT_3D('',#51176,#33283,#33284);
#26982=AXIS2_PLACEMENT_3D('',#51177,#33285,#33286);
#26983=AXIS2_PLACEMENT_3D('',#51180,#33288,#33289);
#26984=AXIS2_PLACEMENT_3D('',#51181,#33290,#33291);
#26985=AXIS2_PLACEMENT_3D('',#51182,#33292,#33293);
#26986=AXIS2_PLACEMENT_3D('',#51183,#33294,#33295);
#26987=AXIS2_PLACEMENT_3D('',#51184,#33296,#33297);
#26988=AXIS2_PLACEMENT_3D('',#51185,#33298,#33299);
#26989=AXIS2_PLACEMENT_3D('',#51186,#33300,#33301);
#26990=AXIS2_PLACEMENT_3D('',#51187,#33302,#33303);
#26991=AXIS2_PLACEMENT_3D('',#51188,#33304,#33305);
#26992=AXIS2_PLACEMENT_3D('',#51189,#33306,#33307);
#26993=AXIS2_PLACEMENT_3D('',#51190,#33308,#33309);
#26994=AXIS2_PLACEMENT_3D('',#51191,#33310,#33311);
#26995=AXIS2_PLACEMENT_3D('',#51192,#33312,#33313);
#26996=AXIS2_PLACEMENT_3D('',#51193,#33314,#33315);
#26997=AXIS2_PLACEMENT_3D('',#51194,#33316,#33317);
#26998=AXIS2_PLACEMENT_3D('',#51195,#33318,#33319);
#26999=AXIS2_PLACEMENT_3D('',#51196,#33320,#33321);
#27000=AXIS2_PLACEMENT_3D('',#51197,#33322,#33323);
#27001=AXIS2_PLACEMENT_3D('',#51199,#33324,#33325);
#27002=AXIS2_PLACEMENT_3D('',#51203,#33327,#33328);
#27003=AXIS2_PLACEMENT_3D('',#51206,#33330,#33331);
#27004=AXIS2_PLACEMENT_3D('',#51207,#33332,#33333);
#27005=AXIS2_PLACEMENT_3D('',#51215,#33336,#33337);
#27006=AXIS2_PLACEMENT_3D('',#51220,#33339,#33340);
#27007=AXIS2_PLACEMENT_3D('',#51221,#33341,#33342);
#27008=AXIS2_PLACEMENT_3D('',#51223,#33343,#33344);
#27009=AXIS2_PLACEMENT_3D('',#51225,#33346,#33347);
#27010=AXIS2_PLACEMENT_3D('',#51229,#33349,#33350);
#27011=AXIS2_PLACEMENT_3D('',#51230,#33351,#33352);
#27012=AXIS2_PLACEMENT_3D('',#51239,#33357,#33358);
#27013=AXIS2_PLACEMENT_3D('',#51245,#33362,#33363);
#27014=AXIS2_PLACEMENT_3D('',#51251,#33367,#33368);
#27015=AXIS2_PLACEMENT_3D('',#51257,#33372,#33373);
#27016=AXIS2_PLACEMENT_3D('',#51263,#33377,#33378);
#27017=AXIS2_PLACEMENT_3D('',#51266,#33381,#33382);
#27018=AXIS2_PLACEMENT_3D('',#51267,#33383,#33384);
#27019=AXIS2_PLACEMENT_3D('',#51269,#33385,#33386);
#27020=AXIS2_PLACEMENT_3D('',#51270,#33387,#33388);
#27021=AXIS2_PLACEMENT_3D('',#51272,#33390,#33391);
#27022=AXIS2_PLACEMENT_3D('',#51274,#33392,#33393);
#27023=AXIS2_PLACEMENT_3D('',#51276,#33395,#33396);
#27024=AXIS2_PLACEMENT_3D('',#51277,#33397,#33398);
#27025=AXIS2_PLACEMENT_3D('',#51278,#33399,#33400);
#27026=AXIS2_PLACEMENT_3D('',#51279,#33401,#33402);
#27027=AXIS2_PLACEMENT_3D('',#51301,#33404,#33405);
#27028=AXIS2_PLACEMENT_3D('',#51304,#33407,#33408);
#27029=AXIS2_PLACEMENT_3D('',#51306,#33409,#33410);
#27030=AXIS2_PLACEMENT_3D('',#51320,#33411,#33412);
#27031=AXIS2_PLACEMENT_3D('',#51368,#33414,#33415);
#27032=AXIS2_PLACEMENT_3D('',#51416,#33417,#33418);
#27033=AXIS2_PLACEMENT_3D('',#51470,#33420,#33421);
#27034=AXIS2_PLACEMENT_3D('',#51518,#33423,#33424);
#27035=AXIS2_PLACEMENT_3D('',#51566,#33426,#33427);
#27036=AXIS2_PLACEMENT_3D('',#51620,#33429,#33430);
#27037=AXIS2_PLACEMENT_3D('',#51632,#33432,#33433);
#27038=AXIS2_PLACEMENT_3D('',#51638,#33434,#33435);
#27039=AXIS2_PLACEMENT_3D('',#51663,#33437,#33438);
#27040=AXIS2_PLACEMENT_3D('',#51688,#33440,#33441);
#27041=AXIS2_PLACEMENT_3D('',#51712,#33443,#33444);
#27042=AXIS2_PLACEMENT_3D('',#51737,#33446,#33447);
#27043=AXIS2_PLACEMENT_3D('',#51762,#33449,#33450);
#27044=AXIS2_PLACEMENT_3D('',#51786,#33452,#33453);
#27045=AXIS2_PLACEMENT_3D('',#51791,#33455,#33456);
#27046=AXIS2_PLACEMENT_3D('',#52138,#33457,#33458);
#27047=AXIS2_PLACEMENT_3D('',#52185,#33459,#33460);
#27048=AXIS2_PLACEMENT_3D('',#52186,#33461,#33462);
#27049=AXIS2_PLACEMENT_3D('',#52458,#33463,#33464);
#27050=AXIS2_PLACEMENT_3D('',#52467,#33469,#33470);
#27051=AXIS2_PLACEMENT_3D('',#52476,#33475,#33476);
#27052=AXIS2_PLACEMENT_3D('',#52485,#33481,#33482);
#27053=AXIS2_PLACEMENT_3D('',#52491,#33486,#33487);
#27054=AXIS2_PLACEMENT_3D('',#52494,#33490,#33491);
#27055=AXIS2_PLACEMENT_3D('',#52500,#33495,#33496);
#27056=AXIS2_PLACEMENT_3D('',#52502,#33497,#33498);
#27057=AXIS2_PLACEMENT_3D('',#52513,#33505,#33506);
#27058=AXIS2_PLACEMENT_3D('',#52517,#33509,#33510);
#27059=AXIS2_PLACEMENT_3D('',#52521,#33513,#33514);
#27060=AXIS2_PLACEMENT_3D('',#52525,#33517,#33518);
#27061=AXIS2_PLACEMENT_3D('',#52529,#33521,#33522);
#27062=AXIS2_PLACEMENT_3D('',#52531,#33524,#33525);
#27063=AXIS2_PLACEMENT_3D('',#52533,#33527,#33528);
#27064=AXIS2_PLACEMENT_3D('',#52534,#33529,#33530);
#27065=AXIS2_PLACEMENT_3D('',#52536,#33531,#33532);
#27066=AXIS2_PLACEMENT_3D('',#52537,#33533,#33534);
#27067=AXIS2_PLACEMENT_3D('',#52539,#33536,#33537);
#27068=AXIS2_PLACEMENT_3D('',#52540,#33538,#33539);
#27069=AXIS2_PLACEMENT_3D('',#52541,#33540,#33541);
#27070=AXIS2_PLACEMENT_3D('',#52543,#33542,#33543);
#27071=AXIS2_PLACEMENT_3D('',#52544,#33544,#33545);
#27072=AXIS2_PLACEMENT_3D('',#52546,#33546,#33547);
#27073=AXIS2_PLACEMENT_3D('',#52548,#33549,#33550);
#27074=AXIS2_PLACEMENT_3D('',#52550,#33552,#33553);
#27075=AXIS2_PLACEMENT_3D('',#52551,#33554,#33555);
#27076=AXIS2_PLACEMENT_3D('',#52573,#33557,#33558);
#27077=AXIS2_PLACEMENT_3D('',#52576,#33560,#33561);
#27078=AXIS2_PLACEMENT_3D('',#52578,#33562,#33563);
#27079=AXIS2_PLACEMENT_3D('',#52592,#33564,#33565);
#27080=AXIS2_PLACEMENT_3D('',#52640,#33567,#33568);
#27081=AXIS2_PLACEMENT_3D('',#52688,#33570,#33571);
#27082=AXIS2_PLACEMENT_3D('',#52742,#33573,#33574);
#27083=AXIS2_PLACEMENT_3D('',#52790,#33576,#33577);
#27084=AXIS2_PLACEMENT_3D('',#52838,#33579,#33580);
#27085=AXIS2_PLACEMENT_3D('',#52892,#33582,#33583);
#27086=AXIS2_PLACEMENT_3D('',#52940,#33585,#33586);
#27087=AXIS2_PLACEMENT_3D('',#52988,#33588,#33589);
#27088=AXIS2_PLACEMENT_3D('',#53036,#33591,#33592);
#27089=AXIS2_PLACEMENT_3D('',#53090,#33594,#33595);
#27090=AXIS2_PLACEMENT_3D('',#53138,#33597,#33598);
#27091=AXIS2_PLACEMENT_3D('',#53186,#33600,#33601);
#27092=AXIS2_PLACEMENT_3D('',#53240,#33603,#33604);
#27093=AXIS2_PLACEMENT_3D('',#53288,#33606,#33607);
#27094=AXIS2_PLACEMENT_3D('',#53336,#33609,#33610);
#27095=AXIS2_PLACEMENT_3D('',#53345,#33612,#33613);
#27096=AXIS2_PLACEMENT_3D('',#53346,#33614,#33615);
#27097=AXIS2_PLACEMENT_3D('',#53361,#33617,#33618);
#27098=AXIS2_PLACEMENT_3D('',#53371,#33619,#33620);
#27099=AXIS2_PLACEMENT_3D('',#53395,#33622,#33623);
#27100=AXIS2_PLACEMENT_3D('',#53420,#33625,#33626);
#27101=AXIS2_PLACEMENT_3D('',#53445,#33628,#33629);
#27102=AXIS2_PLACEMENT_3D('',#53469,#33631,#33632);
#27103=AXIS2_PLACEMENT_3D('',#53494,#33634,#33635);
#27104=AXIS2_PLACEMENT_3D('',#53519,#33637,#33638);
#27105=AXIS2_PLACEMENT_3D('',#53543,#33640,#33641);
#27106=AXIS2_PLACEMENT_3D('',#53567,#33643,#33644);
#27107=AXIS2_PLACEMENT_3D('',#53592,#33646,#33647);
#27108=AXIS2_PLACEMENT_3D('',#53617,#33649,#33650);
#27109=AXIS2_PLACEMENT_3D('',#53641,#33652,#33653);
#27110=AXIS2_PLACEMENT_3D('',#53666,#33655,#33656);
#27111=AXIS2_PLACEMENT_3D('',#53691,#33658,#33659);
#27112=AXIS2_PLACEMENT_3D('',#53715,#33661,#33662);
#27113=AXIS2_PLACEMENT_3D('',#53720,#33664,#33665);
#27114=AXIS2_PLACEMENT_3D('',#54280,#33666,#33667);
#27115=AXIS2_PLACEMENT_3D('',#54327,#33668,#33669);
#27116=AXIS2_PLACEMENT_3D('',#54328,#33670,#33671);
#27117=AXIS2_PLACEMENT_3D('',#54813,#33672,#33673);
#27118=AXIS2_PLACEMENT_3D('',#54814,#33674,#33675);
#27119=AXIS2_PLACEMENT_3D('',#54815,#33676,#33677);
#27120=AXIS2_PLACEMENT_3D('',#54824,#33682,#33683);
#27121=AXIS2_PLACEMENT_3D('',#54833,#33688,#33689);
#27122=AXIS2_PLACEMENT_3D('',#54842,#33694,#33695);
#27123=AXIS2_PLACEMENT_3D('',#54848,#33699,#33700);
#27124=AXIS2_PLACEMENT_3D('',#54851,#33703,#33704);
#27125=AXIS2_PLACEMENT_3D('',#54857,#33708,#33709);
#27126=AXIS2_PLACEMENT_3D('',#54859,#33710,#33711);
#27127=AXIS2_PLACEMENT_3D('',#54870,#33718,#33719);
#27128=AXIS2_PLACEMENT_3D('',#54874,#33722,#33723);
#27129=AXIS2_PLACEMENT_3D('',#54878,#33726,#33727);
#27130=AXIS2_PLACEMENT_3D('',#54882,#33730,#33731);
#27131=AXIS2_PLACEMENT_3D('',#54886,#33734,#33735);
#27132=AXIS2_PLACEMENT_3D('',#54888,#33737,#33738);
#27133=AXIS2_PLACEMENT_3D('',#54890,#33740,#33741);
#27134=AXIS2_PLACEMENT_3D('',#54891,#33742,#33743);
#27135=AXIS2_PLACEMENT_3D('',#54893,#33744,#33745);
#27136=AXIS2_PLACEMENT_3D('',#54894,#33746,#33747);
#27137=AXIS2_PLACEMENT_3D('',#54896,#33749,#33750);
#27138=AXIS2_PLACEMENT_3D('',#54898,#33751,#33752);
#27139=AXIS2_PLACEMENT_3D('',#54899,#33753,#33754);
#27140=AXIS2_PLACEMENT_3D('',#54901,#33755,#33756);
#27141=AXIS2_PLACEMENT_3D('',#54903,#33758,#33759);
#27142=AXIS2_PLACEMENT_3D('',#54905,#33761,#33762);
#27143=AXIS2_PLACEMENT_3D('',#54906,#33763,#33764);
#27144=AXIS2_PLACEMENT_3D('',#54907,#33765,#33766);
#27145=AXIS2_PLACEMENT_3D('',#54908,#33767,#33768);
#27146=AXIS2_PLACEMENT_3D('',#54909,#33769,#33770);
#27147=AXIS2_PLACEMENT_3D('',#54910,#33771,#33772);
#27148=AXIS2_PLACEMENT_3D('',#54911,#33773,#33774);
#27149=AXIS2_PLACEMENT_3D('',#54912,#33775,#33776);
#27150=AXIS2_PLACEMENT_3D('',#54913,#33777,#33778);
#27151=AXIS2_PLACEMENT_3D('',#54914,#33779,#33780);
#27152=AXIS2_PLACEMENT_3D('',#54915,#33781,#33782);
#27153=AXIS2_PLACEMENT_3D('',#54916,#33783,#33784);
#27154=AXIS2_PLACEMENT_3D('',#54917,#33785,#33786);
#27155=AXIS2_PLACEMENT_3D('',#54918,#33787,#33788);
#27156=AXIS2_PLACEMENT_3D('',#54919,#33789,#33790);
#27157=AXIS2_PLACEMENT_3D('',#54920,#33791,#33792);
#27158=AXIS2_PLACEMENT_3D('',#54921,#33793,#33794);
#27159=AXIS2_PLACEMENT_3D('',#54922,#33795,#33796);
#27160=AXIS2_PLACEMENT_3D('',#54923,#33797,#33798);
#27161=AXIS2_PLACEMENT_3D('',#54924,#33799,#33800);
#27162=AXIS2_PLACEMENT_3D('',#54925,#33801,#33802);
#27163=AXIS2_PLACEMENT_3D('',#54926,#33803,#33804);
#27164=AXIS2_PLACEMENT_3D('',#54927,#33805,#33806);
#27165=AXIS2_PLACEMENT_3D('',#54928,#33807,#33808);
#27166=AXIS2_PLACEMENT_3D('',#54929,#33809,#33810);
#27167=AXIS2_PLACEMENT_3D('',#54930,#33811,#33812);
#27168=AXIS2_PLACEMENT_3D('',#54931,#33813,#33814);
#27169=AXIS2_PLACEMENT_3D('',#54932,#33815,#33816);
#27170=AXIS2_PLACEMENT_3D('',#54933,#33817,#33818);
#27171=AXIS2_PLACEMENT_3D('',#54934,#33819,#33820);
#27172=AXIS2_PLACEMENT_3D('',#54935,#33821,#33822);
#27173=AXIS2_PLACEMENT_3D('',#54936,#33823,#33824);
#27174=AXIS2_PLACEMENT_3D('',#54937,#33825,#33826);
#27175=AXIS2_PLACEMENT_3D('',#54938,#33827,#33828);
#27176=AXIS2_PLACEMENT_3D('',#54939,#33829,#33830);
#27177=AXIS2_PLACEMENT_3D('',#54940,#33831,#33832);
#27178=AXIS2_PLACEMENT_3D('',#54941,#33833,#33834);
#27179=AXIS2_PLACEMENT_3D('',#54942,#33835,#33836);
#27180=AXIS2_PLACEMENT_3D('',#54943,#33837,#33838);
#27181=AXIS2_PLACEMENT_3D('',#54944,#33839,#33840);
#27182=AXIS2_PLACEMENT_3D('',#54945,#33841,#33842);
#27183=AXIS2_PLACEMENT_3D('',#54946,#33843,#33844);
#27184=AXIS2_PLACEMENT_3D('',#54947,#33845,#33846);
#27185=AXIS2_PLACEMENT_3D('',#54948,#33847,#33848);
#27186=AXIS2_PLACEMENT_3D('',#54949,#33849,#33850);
#27187=AXIS2_PLACEMENT_3D('',#54950,#33851,#33852);
#27188=AXIS2_PLACEMENT_3D('',#54951,#33853,#33854);
#27189=AXIS2_PLACEMENT_3D('',#54952,#33855,#33856);
#27190=AXIS2_PLACEMENT_3D('',#54953,#33857,#33858);
#27191=AXIS2_PLACEMENT_3D('',#54954,#33859,#33860);
#27192=AXIS2_PLACEMENT_3D('',#54955,#33861,#33862);
#27193=AXIS2_PLACEMENT_3D('',#54956,#33863,#33864);
#27194=AXIS2_PLACEMENT_3D('',#54957,#33865,#33866);
#27195=AXIS2_PLACEMENT_3D('',#54958,#33867,#33868);
#27196=DIRECTION('axis',(0.,0.,1.));
#27197=DIRECTION('refdir',(1.,0.,0.));
#27198=DIRECTION('axis',(0.,0.,1.));
#27199=DIRECTION('refdir',(1.,0.,0.));
#27200=DIRECTION('center_axis',(0.,-5.65390683043825E-15,1.));
#27201=DIRECTION('ref_axis',(-1.,-3.05476520284318E-17,0.));
#27202=DIRECTION('center_axis',(0.,0.,1.));
#27203=DIRECTION('ref_axis',(-1.,-6.12323399573677E-17,0.));
#27204=DIRECTION('',(0.382683432365093,-5.25870392309198E-15,0.923879532511285));
#27205=DIRECTION('center_axis',(0.,0.,-1.));
#27206=DIRECTION('ref_axis',(-1.,0.,0.));
#27207=DIRECTION('center_axis',(0.,0.,-1.));
#27208=DIRECTION('ref_axis',(-1.,0.,0.));
#27209=DIRECTION('center_axis',(0.,0.,1.));
#27210=DIRECTION('ref_axis',(-1.,0.,0.));
#27211=DIRECTION('',(-0.707106781186547,-8.65956056235493E-17,-0.707106781186547));
#27212=DIRECTION('center_axis',(0.,0.,-1.));
#27213=DIRECTION('ref_axis',(-1.,-6.12323399573677E-17,0.));
#27214=DIRECTION('center_axis',(0.,0.,1.));
#27215=DIRECTION('ref_axis',(1.,0.,0.));
#27216=DIRECTION('center_axis',(0.,0.,1.));
#27217=DIRECTION('ref_axis',(1.,0.,0.));
#27218=DIRECTION('',(0.,0.,-1.));
#27219=DIRECTION('center_axis',(0.,1.35412816153563E-14,-1.));
#27220=DIRECTION('ref_axis',(-1.,-3.07842030208353E-17,0.));
#27221=DIRECTION('center_axis',(0.,0.,1.));
#27222=DIRECTION('ref_axis',(-1.,-6.12323399573677E-17,0.));
#27223=DIRECTION('',(-0.923879532511286,-5.09732241105372E-15,0.382683432365091));
#27224=DIRECTION('center_axis',(0.,0.,-1.));
#27225=DIRECTION('ref_axis',(-1.,0.,0.));
#27226=DIRECTION('center_axis',(0.,0.,-1.));
#27227=DIRECTION('ref_axis',(-1.,0.,0.));
#27228=DIRECTION('',(0.707106781186547,8.65956056235493E-17,-0.707106781186547));
#27229=DIRECTION('center_axis',(0.,0.,-1.));
#27230=DIRECTION('ref_axis',(-1.,-6.12323399573677E-17,0.));
#27231=DIRECTION('center_axis',(0.,0.,1.));
#27232=DIRECTION('ref_axis',(1.,0.,0.));
#27233=DIRECTION('center_axis',(0.,0.,1.));
#27234=DIRECTION('ref_axis',(1.,0.,0.));
#27235=DIRECTION('center_axis',(0.,0.,-1.));
#27236=DIRECTION('ref_axis',(-1.,0.,0.));
#27237=DIRECTION('center_axis',(0.,0.,-1.));
#27238=DIRECTION('ref_axis',(-1.,0.,0.));
#27239=DIRECTION('center_axis',(0.,0.,-1.));
#27240=DIRECTION('ref_axis',(-1.,0.,0.));
#27241=DIRECTION('center_axis',(0.,0.,-1.));
#27242=DIRECTION('ref_axis',(-1.,0.,0.));
#27243=DIRECTION('center_axis',(0.,0.,-1.));
#27244=DIRECTION('ref_axis',(-1.,0.,0.));
#27245=DIRECTION('center_axis',(0.,0.,-1.));
#27246=DIRECTION('ref_axis',(-1.,0.,0.));
#27247=DIRECTION('center_axis',(0.,1.35412816153564E-14,1.));
#27248=DIRECTION('ref_axis',(-1.,-3.07842030208353E-17,0.));
#27249=DIRECTION('',(-0.923879532511287,-5.32360763351127E-15,-0.38268343236509));
#27250=DIRECTION('center_axis',(0.,0.,1.));
#27251=DIRECTION('ref_axis',(-1.,0.,0.));
#27252=DIRECTION('center_axis',(0.,0.,-1.));
#27253=DIRECTION('ref_axis',(-1.,0.,0.));
#27254=DIRECTION('center_axis',(0.,0.,-1.));
#27255=DIRECTION('ref_axis',(-1.,0.,0.));
#27256=DIRECTION('center_axis',(0.,0.,-1.));
#27257=DIRECTION('ref_axis',(1.,0.,0.));
#27258=DIRECTION('center_axis',(0.,0.,-1.));
#27259=DIRECTION('ref_axis',(1.,0.,0.));
#27260=DIRECTION('center_axis',(0.,0.,-1.));
#27261=DIRECTION('ref_axis',(1.,0.,0.));
#27262=DIRECTION('center_axis',(0.,0.,-1.));
#27263=DIRECTION('ref_axis',(1.,0.,0.));
#27264=DIRECTION('center_axis',(0.,0.,-1.));
#27265=DIRECTION('ref_axis',(1.,0.,0.));
#27266=DIRECTION('center_axis',(0.,0.,-1.));
#27267=DIRECTION('ref_axis',(1.,0.,0.));
#27268=DIRECTION('center_axis',(0.,2.10365780063137E-15,-1.));
#27269=DIRECTION('ref_axis',(-1.,2.95769561248064E-17,0.));
#27270=DIRECTION('center_axis',(0.,0.,1.));
#27271=DIRECTION('ref_axis',(-1.,6.12323399573677E-17,0.));
#27272=DIRECTION('',(0.923879532511287,8.90852054498284E-16,-0.38268343236509));
#27273=DIRECTION('center_axis',(0.,0.,-1.));
#27274=DIRECTION('ref_axis',(-1.,0.,0.));
#27275=DIRECTION('',(-0.707106781186548,8.65956056235493E-17,0.707106781186548));
#27276=DIRECTION('center_axis',(0.,0.,-1.));
#27277=DIRECTION('ref_axis',(-1.,6.12323399573677E-17,0.));
#27278=DIRECTION('center_axis',(0.,-8.62308332460521E-16,-1.));
#27279=DIRECTION('ref_axis',(-1.,3.10731507051551E-17,0.));
#27280=DIRECTION('',(-0.382683432365089,8.55425403093723E-16,0.923879532511287));
#27281=DIRECTION('center_axis',(0.,0.,1.));
#27282=DIRECTION('ref_axis',(-1.,0.,0.));
#27283=DIRECTION('center_axis',(0.,0.,1.));
#27284=DIRECTION('ref_axis',(-1.,0.,0.));
#27285=DIRECTION('center_axis',(0.,0.,1.));
#27286=DIRECTION('ref_axis',(1.,0.,0.));
#27287=DIRECTION('center_axis',(0.,0.,-1.));
#27288=DIRECTION('ref_axis',(-1.,0.,0.));
#27289=DIRECTION('center_axis',(0.,0.,-1.));
#27290=DIRECTION('ref_axis',(-1.,0.,0.));
#27291=DIRECTION('',(0.,0.,-1.));
#27292=DIRECTION('center_axis',(0.,-8.62308332460519E-16,1.));
#27293=DIRECTION('ref_axis',(-1.,3.10731507051551E-17,0.));
#27294=DIRECTION('center_axis',(0.,0.,1.));
#27295=DIRECTION('ref_axis',(-1.,6.12323399573677E-17,0.));
#27296=DIRECTION('',(-0.382683432365089,7.61694994987196E-16,-0.923879532511287));
#27297=DIRECTION('center_axis',(0.,0.,1.));
#27298=DIRECTION('ref_axis',(-1.,0.,0.));
#27299=DIRECTION('',(0.707106781186548,-8.65956056235493E-17,0.707106781186548));
#27300=DIRECTION('center_axis',(0.,0.,-1.));
#27301=DIRECTION('ref_axis',(-1.,6.12323399573677E-17,0.));
#27302=DIRECTION('center_axis',(0.,2.10365780063138E-15,1.));
#27303=DIRECTION('ref_axis',(-1.,2.95769561248064E-17,0.));
#27304=DIRECTION('',(0.923879532511288,6.64566832040743E-16,0.382683432365087));
#27305=DIRECTION('center_axis',(0.,0.,1.));
#27306=DIRECTION('ref_axis',(-1.,0.,0.));
#27307=DIRECTION('center_axis',(0.,0.,1.));
#27308=DIRECTION('ref_axis',(1.,0.,0.));
#27309=DIRECTION('center_axis',(0.,0.,-1.));
#27310=DIRECTION('ref_axis',(-1.,0.,0.));
#27311=DIRECTION('center_axis',(0.,0.,-1.));
#27312=DIRECTION('ref_axis',(1.,0.,0.));
#27313=DIRECTION('center_axis',(0.,0.,-1.));
#27314=DIRECTION('ref_axis',(1.,0.,0.));
#27315=DIRECTION('center_axis',(0.,0.,-1.));
#27316=DIRECTION('ref_axis',(1.,0.,0.));
#27317=DIRECTION('center_axis',(0.,0.,-1.));
#27318=DIRECTION('ref_axis',(1.,0.,0.));
#27319=DIRECTION('',(0.70710678118655,-8.65956056235497E-17,0.707106781186545));
#27320=DIRECTION('center_axis',(0.,0.,1.));
#27321=DIRECTION('ref_axis',(1.,0.,0.));
#27322=DIRECTION('center_axis',(0.,0.,1.));
#27323=DIRECTION('ref_axis',(1.,0.,0.));
#27324=DIRECTION('center_axis',(0.,0.,-1.));
#27325=DIRECTION('ref_axis',(-1.,0.,0.));
#27326=DIRECTION('center_axis',(0.,0.,-1.));
#27327=DIRECTION('ref_axis',(1.,0.,0.));
#27328=DIRECTION('',(0.,0.,-1.));
#27329=DIRECTION('center_axis',(0.,0.,-1.));
#27330=DIRECTION('ref_axis',(1.,0.,0.));
#27331=DIRECTION('',(0.707106781186545,-8.65956056235491E-17,0.70710678118655));
#27332=DIRECTION('center_axis',(0.,0.,1.));
#27333=DIRECTION('ref_axis',(1.,0.,0.));
#27334=DIRECTION('center_axis',(0.,0.,1.));
#27335=DIRECTION('ref_axis',(1.,0.,0.));
#27336=DIRECTION('center_axis',(0.,0.,-1.));
#27337=DIRECTION('ref_axis',(-1.,0.,0.));
#27338=DIRECTION('center_axis',(0.,0.,-1.));
#27339=DIRECTION('ref_axis',(1.,0.,0.));
#27340=DIRECTION('',(0.,0.,-1.));
#27341=DIRECTION('center_axis',(0.,0.,-1.));
#27342=DIRECTION('ref_axis',(1.,0.,0.));
#27343=DIRECTION('',(0.707106781186548,-8.65956056235494E-17,0.707106781186547));
#27344=DIRECTION('center_axis',(0.,0.,1.));
#27345=DIRECTION('ref_axis',(1.,0.,0.));
#27346=DIRECTION('center_axis',(0.,0.,1.));
#27347=DIRECTION('ref_axis',(1.,0.,0.));
#27348=DIRECTION('center_axis',(0.,0.,-1.));
#27349=DIRECTION('ref_axis',(-1.,0.,0.));
#27350=DIRECTION('center_axis',(0.,0.,-1.));
#27351=DIRECTION('ref_axis',(1.,0.,0.));
#27352=DIRECTION('',(0.,0.,-1.));
#27353=DIRECTION('center_axis',(0.,0.,-1.));
#27354=DIRECTION('ref_axis',(1.,0.,0.));
#27355=DIRECTION('',(0.70710678118655,-8.65956056235497E-17,0.707106781186545));
#27356=DIRECTION('center_axis',(0.,0.,1.));
#27357=DIRECTION('ref_axis',(1.,0.,0.));
#27358=DIRECTION('center_axis',(0.,0.,1.));
#27359=DIRECTION('ref_axis',(1.,0.,0.));
#27360=DIRECTION('center_axis',(0.,0.,-1.));
#27361=DIRECTION('ref_axis',(-1.,0.,0.));
#27362=DIRECTION('center_axis',(0.,0.,-1.));
#27363=DIRECTION('ref_axis',(1.,0.,0.));
#27364=DIRECTION('',(0.,0.,-1.));
#27365=DIRECTION('center_axis',(0.,0.,-1.));
#27366=DIRECTION('ref_axis',(1.,0.,0.));
#27367=DIRECTION('',(0.707106781186548,-8.65956056235494E-17,0.707106781186547));
#27368=DIRECTION('center_axis',(0.,0.,1.));
#27369=DIRECTION('ref_axis',(1.,0.,0.));
#27370=DIRECTION('center_axis',(0.,0.,1.));
#27371=DIRECTION('ref_axis',(1.,0.,0.));
#27372=DIRECTION('center_axis',(0.,0.,-1.));
#27373=DIRECTION('ref_axis',(-1.,0.,0.));
#27374=DIRECTION('center_axis',(0.,0.,-1.));
#27375=DIRECTION('ref_axis',(1.,0.,0.));
#27376=DIRECTION('',(0.,0.,-1.));
#27377=DIRECTION('center_axis',(0.,0.,-1.));
#27378=DIRECTION('ref_axis',(1.,0.,0.));
#27379=DIRECTION('',(0.707106781186545,-8.65956056235491E-17,0.70710678118655));
#27380=DIRECTION('center_axis',(0.,0.,1.));
#27381=DIRECTION('ref_axis',(1.,0.,0.));
#27382=DIRECTION('center_axis',(0.,0.,1.));
#27383=DIRECTION('ref_axis',(1.,0.,0.));
#27384=DIRECTION('center_axis',(0.,0.,-1.));
#27385=DIRECTION('ref_axis',(-1.,0.,0.));
#27386=DIRECTION('center_axis',(0.,0.,-1.));
#27387=DIRECTION('ref_axis',(1.,0.,0.));
#27388=DIRECTION('',(0.,0.,-1.));
#27389=DIRECTION('center_axis',(0.,-5.65390683043823E-15,-1.));
#27390=DIRECTION('ref_axis',(-1.,-3.05476520284318E-17,0.));
#27391=DIRECTION('',(0.382683432365092,-5.16497351498544E-15,-0.923879532511286));
#27392=DIRECTION('center_axis',(0.,0.,1.));
#27393=DIRECTION('ref_axis',(-1.,0.,0.));
#27394=DIRECTION('center_axis',(0.,0.,1.));
#27395=DIRECTION('ref_axis',(-1.,0.,0.));
#27396=DIRECTION('center_axis',(0.,0.,1.));
#27397=DIRECTION('ref_axis',(1.,0.,0.));
#27398=DIRECTION('',(0.,0.,-1.));
#27399=DIRECTION('center_axis',(0.,0.,-1.));
#27400=DIRECTION('ref_axis',(1.,0.,0.));
#27401=DIRECTION('center_axis',(0.,0.,1.));
#27402=DIRECTION('ref_axis',(1.,0.,0.));
#27403=DIRECTION('',(0.70710678118655,8.65956056235496E-17,-0.707106781186545));
#27404=DIRECTION('center_axis',(0.,0.,1.));
#27405=DIRECTION('ref_axis',(1.,0.,0.));
#27406=DIRECTION('center_axis',(0.,0.,1.));
#27407=DIRECTION('ref_axis',(1.,0.,0.));
#27408=DIRECTION('center_axis',(0.,0.,1.));
#27409=DIRECTION('ref_axis',(1.,0.,0.));
#27410=DIRECTION('center_axis',(0.,0.,-1.));
#27411=DIRECTION('ref_axis',(1.,0.,0.));
#27412=DIRECTION('',(0.70710678118655,-8.65956056235496E-17,0.707106781186545));
#27413=DIRECTION('center_axis',(0.,0.,-1.));
#27414=DIRECTION('ref_axis',(1.,0.,0.));
#27415=DIRECTION('center_axis',(0.,0.,-1.));
#27416=DIRECTION('ref_axis',(-1.,0.,0.));
#27417=DIRECTION('center_axis',(0.,0.,1.));
#27418=DIRECTION('ref_axis',(1.,0.,0.));
#27419=DIRECTION('center_axis',(0.,0.,1.));
#27420=DIRECTION('ref_axis',(1.,0.,0.));
#27421=DIRECTION('',(0.,0.,1.));
#27422=DIRECTION('center_axis',(0.,0.,1.));
#27423=DIRECTION('ref_axis',(1.,0.,0.));
#27424=DIRECTION('',(-0.857167300702112,-1.04972719113862E-16,0.515038074910054));
#27425=DIRECTION('center_axis',(0.,0.,1.));
#27426=DIRECTION('ref_axis',(1.,0.,0.));
#27427=DIRECTION('center_axis',(0.,0.,1.));
#27428=DIRECTION('ref_axis',(1.,0.,0.));
#27429=DIRECTION('',(0.,0.,1.));
#27430=DIRECTION('center_axis',(0.,0.,1.));
#27431=DIRECTION('ref_axis',(1.,0.,0.));
#27432=DIRECTION('center_axis',(0.,0.,1.));
#27433=DIRECTION('ref_axis',(1.,0.,0.));
#27434=DIRECTION('',(-0.707106781186548,-8.65956056235494E-17,0.707106781186547));
#27435=DIRECTION('center_axis',(0.,0.,1.));
#27436=DIRECTION('ref_axis',(1.,0.,0.));
#27437=DIRECTION('',(-0.857167300702112,-1.04972719113862E-16,0.515038074910054));
#27438=DIRECTION('center_axis',(0.,0.,1.));
#27439=DIRECTION('ref_axis',(1.,0.,0.));
#27440=DIRECTION('center_axis',(0.,0.,1.));
#27441=DIRECTION('ref_axis',(1.,0.,0.));
#27442=DIRECTION('',(0.,0.,1.));
#27443=DIRECTION('center_axis',(0.,0.,1.));
#27444=DIRECTION('ref_axis',(1.,0.,0.));
#27445=DIRECTION('center_axis',(0.,0.,1.));
#27446=DIRECTION('ref_axis',(1.,0.,0.));
#27447=DIRECTION('',(-0.707106781186548,-8.65956056235494E-17,0.707106781186547));
#27448=DIRECTION('center_axis',(0.,0.,1.));
#27449=DIRECTION('ref_axis',(1.,0.,0.));
#27450=DIRECTION('',(-0.857167300702113,-1.04972719113862E-16,0.515038074910054));
#27451=DIRECTION('center_axis',(0.,0.,1.));
#27452=DIRECTION('ref_axis',(1.,0.,0.));
#27453=DIRECTION('center_axis',(0.,0.,1.));
#27454=DIRECTION('ref_axis',(1.,0.,0.));
#27455=DIRECTION('',(0.,0.,1.));
#27456=DIRECTION('center_axis',(0.,0.,1.));
#27457=DIRECTION('ref_axis',(1.,0.,0.));
#27458=DIRECTION('center_axis',(0.,0.,1.));
#27459=DIRECTION('ref_axis',(1.,0.,0.));
#27460=DIRECTION('',(-0.707106781186548,-8.65956056235494E-17,0.707106781186547));
#27461=DIRECTION('center_axis',(0.,0.,1.));
#27462=DIRECTION('ref_axis',(-1.,0.,0.));
#27463=DIRECTION('',(-0.316227766016837,3.87267321454038E-17,-0.948683298050514));
#27464=DIRECTION('center_axis',(0.,0.,-1.));
#27465=DIRECTION('ref_axis',(1.,0.,0.));
#27466=DIRECTION('center_axis',(0.,0.,-1.));
#27467=DIRECTION('ref_axis',(-1.,0.,0.));
#27468=DIRECTION('',(0.,0.,-1.));
#27469=DIRECTION('center_axis',(0.,0.,-1.));
#27470=DIRECTION('ref_axis',(1.,0.,0.));
#27471=DIRECTION('center_axis',(0.,0.,-1.));
#27472=DIRECTION('ref_axis',(-1.,0.,0.));
#27473=DIRECTION('',(0.707106781186546,-8.65956056235491E-17,-0.707106781186549));
#27474=DIRECTION('center_axis',(0.,0.,-1.));
#27475=DIRECTION('ref_axis',(1.,0.,0.));
#27476=DIRECTION('center_axis',(0.,0.,1.));
#27477=DIRECTION('ref_axis',(1.,0.,0.));
#27478=DIRECTION('center_axis',(0.,0.,1.));
#27479=DIRECTION('ref_axis',(-1.,0.,0.));
#27480=DIRECTION('',(-0.316227766016837,3.87267321454038E-17,-0.948683298050514));
#27481=DIRECTION('center_axis',(0.,0.,-1.));
#27482=DIRECTION('ref_axis',(1.,0.,0.));
#27483=DIRECTION('center_axis',(0.,0.,-1.));
#27484=DIRECTION('ref_axis',(-1.,0.,0.));
#27485=DIRECTION('',(0.,0.,-1.));
#27486=DIRECTION('center_axis',(0.,0.,-1.));
#27487=DIRECTION('ref_axis',(1.,0.,0.));
#27488=DIRECTION('center_axis',(0.,0.,-1.));
#27489=DIRECTION('ref_axis',(-1.,0.,0.));
#27490=DIRECTION('',(0.707106781186546,-8.65956056235492E-17,-0.707106781186549));
#27491=DIRECTION('center_axis',(0.,0.,-1.));
#27492=DIRECTION('ref_axis',(1.,0.,0.));
#27493=DIRECTION('center_axis',(0.,0.,1.));
#27494=DIRECTION('ref_axis',(1.,0.,0.));
#27495=DIRECTION('center_axis',(0.,0.,1.));
#27496=DIRECTION('ref_axis',(-1.,0.,0.));
#27497=DIRECTION('',(-0.316227766016842,3.87267321454044E-17,-0.948683298050512));
#27498=DIRECTION('center_axis',(0.,0.,-1.));
#27499=DIRECTION('ref_axis',(1.,0.,0.));
#27500=DIRECTION('center_axis',(0.,0.,-1.));
#27501=DIRECTION('ref_axis',(-1.,0.,0.));
#27502=DIRECTION('',(0.,0.,-1.));
#27503=DIRECTION('center_axis',(0.,0.,-1.));
#27504=DIRECTION('ref_axis',(1.,0.,0.));
#27505=DIRECTION('center_axis',(0.,0.,-1.));
#27506=DIRECTION('ref_axis',(-1.,0.,0.));
#27507=DIRECTION('',(0.707106781186552,-8.65956056235499E-17,-0.707106781186543));
#27508=DIRECTION('center_axis',(0.,0.,-1.));
#27509=DIRECTION('ref_axis',(1.,0.,0.));
#27510=DIRECTION('center_axis',(0.,0.,1.));
#27511=DIRECTION('ref_axis',(1.,0.,0.));
#27512=DIRECTION('center_axis',(0.,0.,1.));
#27513=DIRECTION('ref_axis',(-1.,0.,0.));
#27514=DIRECTION('',(-0.316227766016837,3.87267321454038E-17,-0.948683298050514));
#27515=DIRECTION('center_axis',(0.,0.,-1.));
#27516=DIRECTION('ref_axis',(1.,0.,0.));
#27517=DIRECTION('center_axis',(0.,0.,-1.));
#27518=DIRECTION('ref_axis',(-1.,0.,0.));
#27519=DIRECTION('',(0.,0.,-1.));
#27520=DIRECTION('center_axis',(0.,0.,-1.));
#27521=DIRECTION('ref_axis',(1.,0.,0.));
#27522=DIRECTION('center_axis',(0.,0.,-1.));
#27523=DIRECTION('ref_axis',(-1.,0.,0.));
#27524=DIRECTION('',(0.707106781186546,-8.65956056235492E-17,-0.707106781186549));
#27525=DIRECTION('center_axis',(0.,0.,-1.));
#27526=DIRECTION('ref_axis',(1.,0.,0.));
#27527=DIRECTION('center_axis',(0.,0.,1.));
#27528=DIRECTION('ref_axis',(1.,0.,0.));
#27529=DIRECTION('center_axis',(0.,0.,1.));
#27530=DIRECTION('ref_axis',(-1.,0.,0.));
#27531=DIRECTION('',(-0.316227766016837,3.87267321454038E-17,-0.948683298050514));
#27532=DIRECTION('center_axis',(0.,0.,-1.));
#27533=DIRECTION('ref_axis',(1.,0.,0.));
#27534=DIRECTION('center_axis',(0.,0.,-1.));
#27535=DIRECTION('ref_axis',(-1.,0.,0.));
#27536=DIRECTION('',(0.,0.,-1.));
#27537=DIRECTION('center_axis',(0.,0.,-1.));
#27538=DIRECTION('ref_axis',(1.,0.,0.));
#27539=DIRECTION('center_axis',(0.,0.,-1.));
#27540=DIRECTION('ref_axis',(-1.,0.,0.));
#27541=DIRECTION('',(0.707106781186546,-8.65956056235491E-17,-0.707106781186549));
#27542=DIRECTION('center_axis',(0.,0.,-1.));
#27543=DIRECTION('ref_axis',(1.,0.,0.));
#27544=DIRECTION('center_axis',(0.,0.,1.));
#27545=DIRECTION('ref_axis',(1.,0.,0.));
#27546=DIRECTION('center_axis',(0.,0.,1.));
#27547=DIRECTION('ref_axis',(-1.,0.,0.));
#27548=DIRECTION('',(-0.316227766016842,3.87267321454044E-17,-0.948683298050512));
#27549=DIRECTION('center_axis',(0.,0.,-1.));
#27550=DIRECTION('ref_axis',(1.,0.,0.));
#27551=DIRECTION('center_axis',(0.,0.,-1.));
#27552=DIRECTION('ref_axis',(-1.,0.,0.));
#27553=DIRECTION('',(0.,0.,-1.));
#27554=DIRECTION('center_axis',(0.,0.,-1.));
#27555=DIRECTION('ref_axis',(1.,0.,0.));
#27556=DIRECTION('center_axis',(0.,0.,-1.));
#27557=DIRECTION('ref_axis',(-1.,0.,0.));
#27558=DIRECTION('',(0.707106781186552,-8.65956056235499E-17,-0.707106781186543));
#27559=DIRECTION('center_axis',(0.,0.,-1.));
#27560=DIRECTION('ref_axis',(1.,0.,0.));
#27561=DIRECTION('center_axis',(0.,0.,1.));
#27562=DIRECTION('ref_axis',(1.,0.,0.));
#27563=DIRECTION('center_axis',(0.,0.,-1.));
#27564=DIRECTION('ref_axis',(-1.,0.,0.));
#27565=DIRECTION('',(0.707106781186548,8.65956056235493E-17,-0.707106781186548));
#27566=DIRECTION('center_axis',(0.,0.,1.));
#27567=DIRECTION('ref_axis',(-1.,0.,0.));
#27568=DIRECTION('center_axis',(0.,0.,1.));
#27569=DIRECTION('ref_axis',(-1.,0.,0.));
#27570=DIRECTION('center_axis',(0.,0.,1.));
#27571=DIRECTION('ref_axis',(1.,0.,0.));
#27572=DIRECTION('',(0.,0.,-1.));
#27573=DIRECTION('axis',(0.,0.,1.));
#27574=DIRECTION('refdir',(1.,0.,0.));
#27575=DIRECTION('center_axis',(0.,0.,-1.));
#27576=DIRECTION('ref_axis',(-1.,0.,0.));
#27577=DIRECTION('',(0.857167300702112,-1.04972719113862E-16,-0.515038074910055));
#27578=DIRECTION('center_axis',(0.,0.,-1.));
#27579=DIRECTION('ref_axis',(1.,0.,0.));
#27580=DIRECTION('center_axis',(0.,0.,-1.));
#27581=DIRECTION('ref_axis',(-1.,0.,0.));
#27582=DIRECTION('',(0.,0.,-1.));
#27583=DIRECTION('center_axis',(0.,0.,-1.));
#27584=DIRECTION('ref_axis',(1.,0.,0.));
#27585=DIRECTION('center_axis',(0.,0.,-1.));
#27586=DIRECTION('ref_axis',(-1.,0.,0.));
#27587=DIRECTION('',(0.707106781186548,-8.65956056235494E-17,-0.707106781186547));
#27588=DIRECTION('center_axis',(0.,0.,1.));
#27589=DIRECTION('ref_axis',(-1.,0.,0.));
#27590=DIRECTION('center_axis',(0.,0.,-1.));
#27591=DIRECTION('ref_axis',(-1.,0.,0.));
#27592=DIRECTION('',(0.857167300702112,-1.04972719113862E-16,-0.515038074910055));
#27593=DIRECTION('center_axis',(0.,0.,-1.));
#27594=DIRECTION('ref_axis',(1.,0.,0.));
#27595=DIRECTION('center_axis',(0.,0.,-1.));
#27596=DIRECTION('ref_axis',(-1.,0.,0.));
#27597=DIRECTION('',(0.,0.,-1.));
#27598=DIRECTION('center_axis',(0.,0.,-1.));
#27599=DIRECTION('ref_axis',(1.,0.,0.));
#27600=DIRECTION('center_axis',(0.,0.,-1.));
#27601=DIRECTION('ref_axis',(-1.,0.,0.));
#27602=DIRECTION('',(0.707106781186548,-8.65956056235494E-17,-0.707106781186547));
#27603=DIRECTION('center_axis',(0.,0.,1.));
#27604=DIRECTION('ref_axis',(-1.,0.,0.));
#27605=DIRECTION('center_axis',(0.,0.,-1.));
#27606=DIRECTION('ref_axis',(-1.,0.,0.));
#27607=DIRECTION('',(0.857167300702111,-1.04972719113862E-16,-0.515038074910057));
#27608=DIRECTION('center_axis',(0.,0.,-1.));
#27609=DIRECTION('ref_axis',(1.,0.,0.));
#27610=DIRECTION('center_axis',(0.,0.,-1.));
#27611=DIRECTION('ref_axis',(-1.,0.,0.));
#27612=DIRECTION('',(0.,0.,-1.));
#27613=DIRECTION('center_axis',(0.,0.,-1.));
#27614=DIRECTION('ref_axis',(1.,0.,0.));
#27615=DIRECTION('center_axis',(0.,0.,-1.));
#27616=DIRECTION('ref_axis',(-1.,0.,0.));
#27617=DIRECTION('',(0.70710678118655,-8.65956056235496E-17,-0.707106781186545));
#27618=DIRECTION('center_axis',(0.,0.,1.));
#27619=DIRECTION('ref_axis',(-1.,0.,0.));
#27620=DIRECTION('center_axis',(0.,0.,-1.));
#27621=DIRECTION('ref_axis',(-1.,0.,0.));
#27622=DIRECTION('',(0.857167300702112,-1.04972719113862E-16,-0.515038074910055));
#27623=DIRECTION('center_axis',(0.,0.,-1.));
#27624=DIRECTION('ref_axis',(1.,0.,0.));
#27625=DIRECTION('center_axis',(0.,0.,-1.));
#27626=DIRECTION('ref_axis',(-1.,0.,0.));
#27627=DIRECTION('',(0.,0.,-1.));
#27628=DIRECTION('center_axis',(0.,0.,-1.));
#27629=DIRECTION('ref_axis',(1.,0.,0.));
#27630=DIRECTION('center_axis',(0.,0.,-1.));
#27631=DIRECTION('ref_axis',(-1.,0.,0.));
#27632=DIRECTION('',(0.707106781186548,-8.65956056235494E-17,-0.707106781186547));
#27633=DIRECTION('center_axis',(0.,0.,1.));
#27634=DIRECTION('ref_axis',(-1.,0.,0.));
#27635=DIRECTION('center_axis',(0.,0.,-1.));
#27636=DIRECTION('ref_axis',(-1.,0.,0.));
#27637=DIRECTION('',(0.857167300702112,-1.04972719113862E-16,-0.515038074910055));
#27638=DIRECTION('center_axis',(0.,0.,-1.));
#27639=DIRECTION('ref_axis',(1.,0.,0.));
#27640=DIRECTION('center_axis',(0.,0.,-1.));
#27641=DIRECTION('ref_axis',(-1.,0.,0.));
#27642=DIRECTION('',(0.,0.,-1.));
#27643=DIRECTION('center_axis',(0.,0.,-1.));
#27644=DIRECTION('ref_axis',(1.,0.,0.));
#27645=DIRECTION('center_axis',(0.,0.,-1.));
#27646=DIRECTION('ref_axis',(-1.,0.,0.));
#27647=DIRECTION('',(0.707106781186548,-8.65956056235494E-17,-0.707106781186547));
#27648=DIRECTION('center_axis',(0.,0.,1.));
#27649=DIRECTION('ref_axis',(-1.,0.,0.));
#27650=DIRECTION('center_axis',(0.,0.,-1.));
#27651=DIRECTION('ref_axis',(-1.,0.,0.));
#27652=DIRECTION('',(0.857167300702111,-1.04972719113862E-16,-0.515038074910057));
#27653=DIRECTION('center_axis',(0.,0.,-1.));
#27654=DIRECTION('ref_axis',(1.,0.,0.));
#27655=DIRECTION('center_axis',(0.,0.,-1.));
#27656=DIRECTION('ref_axis',(-1.,0.,0.));
#27657=DIRECTION('',(0.,0.,-1.));
#27658=DIRECTION('center_axis',(0.,0.,-1.));
#27659=DIRECTION('ref_axis',(1.,0.,0.));
#27660=DIRECTION('center_axis',(0.,0.,-1.));
#27661=DIRECTION('ref_axis',(-1.,0.,0.));
#27662=DIRECTION('',(0.70710678118655,-8.65956056235496E-17,-0.707106781186545));
#27663=DIRECTION('center_axis',(0.,0.,1.));
#27664=DIRECTION('ref_axis',(-1.,0.,0.));
#27665=DIRECTION('center_axis',(0.,0.,1.));
#27666=DIRECTION('ref_axis',(1.,0.,0.));
#27667=DIRECTION('',(-0.857167300702111,-1.04972719113862E-16,0.515038074910057));
#27668=DIRECTION('center_axis',(0.,0.,1.));
#27669=DIRECTION('ref_axis',(1.,0.,0.));
#27670=DIRECTION('center_axis',(0.,0.,1.));
#27671=DIRECTION('ref_axis',(1.,0.,0.));
#27672=DIRECTION('',(0.,0.,1.));
#27673=DIRECTION('center_axis',(0.,0.,1.));
#27674=DIRECTION('ref_axis',(1.,0.,0.));
#27675=DIRECTION('center_axis',(0.,0.,1.));
#27676=DIRECTION('ref_axis',(1.,0.,0.));
#27677=DIRECTION('',(-0.707106781186547,-8.65956056235493E-17,0.707106781186547));
#27678=DIRECTION('center_axis',(0.,0.,-1.));
#27679=DIRECTION('ref_axis',(1.,0.,0.));
#27680=DIRECTION('center_axis',(0.,0.,1.));
#27681=DIRECTION('ref_axis',(1.,0.,0.));
#27682=DIRECTION('',(-0.857167300702112,-1.04972719113862E-16,0.515038074910055));
#27683=DIRECTION('center_axis',(0.,0.,1.));
#27684=DIRECTION('ref_axis',(1.,0.,0.));
#27685=DIRECTION('center_axis',(0.,0.,1.));
#27686=DIRECTION('ref_axis',(1.,0.,0.));
#27687=DIRECTION('',(0.,0.,1.));
#27688=DIRECTION('center_axis',(0.,0.,1.));
#27689=DIRECTION('ref_axis',(1.,0.,0.));
#27690=DIRECTION('center_axis',(0.,0.,1.));
#27691=DIRECTION('ref_axis',(1.,0.,0.));
#27692=DIRECTION('',(-0.707106781186549,-8.65956056235495E-17,0.707106781186546));
#27693=DIRECTION('center_axis',(0.,0.,-1.));
#27694=DIRECTION('ref_axis',(1.,0.,0.));
#27695=DIRECTION('center_axis',(0.,0.,1.));
#27696=DIRECTION('ref_axis',(1.,0.,0.));
#27697=DIRECTION('',(-0.857167300702112,-1.04972719113862E-16,0.515038074910055));
#27698=DIRECTION('center_axis',(0.,0.,1.));
#27699=DIRECTION('ref_axis',(1.,0.,0.));
#27700=DIRECTION('center_axis',(0.,0.,1.));
#27701=DIRECTION('ref_axis',(1.,0.,0.));
#27702=DIRECTION('',(0.,0.,1.));
#27703=DIRECTION('center_axis',(0.,0.,1.));
#27704=DIRECTION('ref_axis',(1.,0.,0.));
#27705=DIRECTION('center_axis',(0.,0.,1.));
#27706=DIRECTION('ref_axis',(1.,0.,0.));
#27707=DIRECTION('',(-0.707106781186549,-8.65956056235495E-17,0.707106781186546));
#27708=DIRECTION('center_axis',(0.,0.,-1.));
#27709=DIRECTION('ref_axis',(1.,0.,0.));
#27710=DIRECTION('center_axis',(0.,0.,1.));
#27711=DIRECTION('ref_axis',(1.,0.,0.));
#27712=DIRECTION('',(-0.857167300702112,-1.04972719113862E-16,0.515038074910055));
#27713=DIRECTION('center_axis',(0.,0.,1.));
#27714=DIRECTION('ref_axis',(1.,0.,0.));
#27715=DIRECTION('center_axis',(0.,0.,1.));
#27716=DIRECTION('ref_axis',(1.,0.,0.));
#27717=DIRECTION('',(0.,0.,1.));
#27718=DIRECTION('center_axis',(0.,0.,1.));
#27719=DIRECTION('ref_axis',(1.,0.,0.));
#27720=DIRECTION('center_axis',(0.,0.,1.));
#27721=DIRECTION('ref_axis',(1.,0.,0.));
#27722=DIRECTION('',(-0.707106781186549,-8.65956056235495E-17,0.707106781186546));
#27723=DIRECTION('center_axis',(0.,0.,-1.));
#27724=DIRECTION('ref_axis',(1.,0.,0.));
#27725=DIRECTION('center_axis',(0.,0.,1.));
#27726=DIRECTION('ref_axis',(1.,0.,0.));
#27727=DIRECTION('',(-0.857167300702112,-1.04972719113862E-16,0.515038074910055));
#27728=DIRECTION('center_axis',(0.,0.,1.));
#27729=DIRECTION('ref_axis',(1.,0.,0.));
#27730=DIRECTION('center_axis',(0.,0.,1.));
#27731=DIRECTION('ref_axis',(1.,0.,0.));
#27732=DIRECTION('',(0.,0.,1.));
#27733=DIRECTION('center_axis',(0.,0.,1.));
#27734=DIRECTION('ref_axis',(1.,0.,0.));
#27735=DIRECTION('center_axis',(0.,0.,1.));
#27736=DIRECTION('ref_axis',(1.,0.,0.));
#27737=DIRECTION('',(-0.707106781186549,-8.65956056235495E-17,0.707106781186546));
#27738=DIRECTION('center_axis',(0.,0.,-1.));
#27739=DIRECTION('ref_axis',(1.,0.,0.));
#27740=DIRECTION('center_axis',(0.,0.,1.));
#27741=DIRECTION('ref_axis',(1.,0.,0.));
#27742=DIRECTION('',(-0.857167300702113,-1.04972719113862E-16,0.515038074910054));
#27743=DIRECTION('center_axis',(0.,0.,1.));
#27744=DIRECTION('ref_axis',(1.,0.,0.));
#27745=DIRECTION('center_axis',(0.,0.,1.));
#27746=DIRECTION('ref_axis',(1.,0.,0.));
#27747=DIRECTION('',(0.,0.,1.));
#27748=DIRECTION('center_axis',(0.,0.,1.));
#27749=DIRECTION('ref_axis',(1.,0.,0.));
#27750=DIRECTION('center_axis',(0.,0.,1.));
#27751=DIRECTION('ref_axis',(1.,0.,0.));
#27752=DIRECTION('',(-0.707106781186548,-8.65956056235494E-17,0.707106781186548));
#27753=DIRECTION('center_axis',(0.,0.,-1.));
#27754=DIRECTION('ref_axis',(1.,0.,0.));
#27755=DIRECTION('center_axis',(0.,0.,1.));
#27756=DIRECTION('ref_axis',(1.,0.,0.));
#27757=DIRECTION('',(-0.857167300702111,-1.04972719113862E-16,0.515038074910057));
#27758=DIRECTION('center_axis',(0.,0.,1.));
#27759=DIRECTION('ref_axis',(1.,0.,0.));
#27760=DIRECTION('center_axis',(0.,0.,1.));
#27761=DIRECTION('ref_axis',(1.,0.,0.));
#27762=DIRECTION('',(0.,0.,1.));
#27763=DIRECTION('center_axis',(0.,0.,1.));
#27764=DIRECTION('ref_axis',(1.,0.,0.));
#27765=DIRECTION('center_axis',(0.,0.,1.));
#27766=DIRECTION('ref_axis',(1.,0.,0.));
#27767=DIRECTION('',(-0.707106781186551,-8.65956056235497E-17,0.707106781186544));
#27768=DIRECTION('center_axis',(0.,0.,-1.));
#27769=DIRECTION('ref_axis',(1.,0.,0.));
#27770=DIRECTION('center_axis',(0.,0.,1.));
#27771=DIRECTION('ref_axis',(1.,0.,0.));
#27772=DIRECTION('',(-0.857167300702112,-1.04972719113862E-16,0.515038074910055));
#27773=DIRECTION('center_axis',(0.,0.,1.));
#27774=DIRECTION('ref_axis',(1.,0.,0.));
#27775=DIRECTION('center_axis',(0.,0.,1.));
#27776=DIRECTION('ref_axis',(1.,0.,0.));
#27777=DIRECTION('',(0.,0.,1.));
#27778=DIRECTION('center_axis',(0.,0.,1.));
#27779=DIRECTION('ref_axis',(1.,0.,0.));
#27780=DIRECTION('center_axis',(0.,0.,1.));
#27781=DIRECTION('ref_axis',(1.,0.,0.));
#27782=DIRECTION('',(-0.707106781186549,-8.65956056235495E-17,0.707106781186546));
#27783=DIRECTION('center_axis',(0.,0.,-1.));
#27784=DIRECTION('ref_axis',(1.,0.,0.));
#27785=DIRECTION('center_axis',(0.,0.,1.));
#27786=DIRECTION('ref_axis',(1.,0.,0.));
#27787=DIRECTION('',(-0.857167300702112,-1.04972719113862E-16,0.515038074910055));
#27788=DIRECTION('center_axis',(0.,0.,1.));
#27789=DIRECTION('ref_axis',(1.,0.,0.));
#27790=DIRECTION('center_axis',(0.,0.,1.));
#27791=DIRECTION('ref_axis',(1.,0.,0.));
#27792=DIRECTION('',(0.,0.,1.));
#27793=DIRECTION('center_axis',(0.,0.,1.));
#27794=DIRECTION('ref_axis',(1.,0.,0.));
#27795=DIRECTION('center_axis',(0.,0.,1.));
#27796=DIRECTION('ref_axis',(1.,0.,0.));
#27797=DIRECTION('',(-0.707106781186548,-8.65956056235494E-17,0.707106781186547));
#27798=DIRECTION('center_axis',(0.,0.,-1.));
#27799=DIRECTION('ref_axis',(1.,0.,0.));
#27800=DIRECTION('center_axis',(0.,0.,1.));
#27801=DIRECTION('ref_axis',(1.,0.,0.));
#27802=DIRECTION('',(-0.857167300702112,-1.04972719113862E-16,0.515038074910055));
#27803=DIRECTION('center_axis',(0.,0.,1.));
#27804=DIRECTION('ref_axis',(1.,0.,0.));
#27805=DIRECTION('center_axis',(0.,0.,1.));
#27806=DIRECTION('ref_axis',(1.,0.,0.));
#27807=DIRECTION('',(0.,0.,1.));
#27808=DIRECTION('center_axis',(0.,0.,1.));
#27809=DIRECTION('ref_axis',(1.,0.,0.));
#27810=DIRECTION('center_axis',(0.,0.,1.));
#27811=DIRECTION('ref_axis',(1.,0.,0.));
#27812=DIRECTION('',(-0.707106781186549,-8.65956056235495E-17,0.707106781186546));
#27813=DIRECTION('center_axis',(0.,0.,-1.));
#27814=DIRECTION('ref_axis',(1.,0.,0.));
#27815=DIRECTION('center_axis',(0.,0.,1.));
#27816=DIRECTION('ref_axis',(1.,0.,0.));
#27817=DIRECTION('',(-0.857167300702112,-1.04972719113862E-16,0.515038074910055));
#27818=DIRECTION('center_axis',(0.,0.,1.));
#27819=DIRECTION('ref_axis',(1.,0.,0.));
#27820=DIRECTION('center_axis',(0.,0.,1.));
#27821=DIRECTION('ref_axis',(1.,0.,0.));
#27822=DIRECTION('',(0.,0.,1.));
#27823=DIRECTION('center_axis',(0.,0.,1.));
#27824=DIRECTION('ref_axis',(1.,0.,0.));
#27825=DIRECTION('center_axis',(0.,0.,1.));
#27826=DIRECTION('ref_axis',(1.,0.,0.));
#27827=DIRECTION('',(-0.707106781186547,-8.65956056235493E-17,0.707106781186547));
#27828=DIRECTION('center_axis',(0.,0.,-1.));
#27829=DIRECTION('ref_axis',(1.,0.,0.));
#27830=DIRECTION('center_axis',(0.,0.,1.));
#27831=DIRECTION('ref_axis',(1.,0.,0.));
#27832=DIRECTION('',(-0.857167300702111,-1.04972719113862E-16,0.515038074910057));
#27833=DIRECTION('center_axis',(0.,0.,1.));
#27834=DIRECTION('ref_axis',(1.,0.,0.));
#27835=DIRECTION('center_axis',(0.,0.,1.));
#27836=DIRECTION('ref_axis',(1.,0.,0.));
#27837=DIRECTION('',(0.,0.,1.));
#27838=DIRECTION('center_axis',(0.,0.,1.));
#27839=DIRECTION('ref_axis',(1.,0.,0.));
#27840=DIRECTION('center_axis',(0.,0.,1.));
#27841=DIRECTION('ref_axis',(1.,0.,0.));
#27842=DIRECTION('',(-0.707106781186547,-8.65956056235493E-17,0.707106781186547));
#27843=DIRECTION('center_axis',(0.,0.,-1.));
#27844=DIRECTION('ref_axis',(1.,0.,0.));
#27845=DIRECTION('center_axis',(0.,0.,-1.));
#27846=DIRECTION('ref_axis',(-1.,0.,0.));
#27847=DIRECTION('center_axis',(0.,0.,-1.));
#27848=DIRECTION('ref_axis',(-1.,0.,0.));
#27849=DIRECTION('',(-0.707106781186542,8.65956056235487E-17,0.707106781186553));
#27850=DIRECTION('center_axis',(0.,0.,1.));
#27851=DIRECTION('ref_axis',(-1.,0.,0.));
#27852=DIRECTION('center_axis',(0.,0.,1.));
#27853=DIRECTION('ref_axis',(-1.,0.,0.));
#27854=DIRECTION('center_axis',(0.,0.,1.));
#27855=DIRECTION('ref_axis',(1.,0.,0.));
#27856=DIRECTION('center_axis',(0.,0.,-1.));
#27857=DIRECTION('ref_axis',(-1.,0.,0.));
#27858=DIRECTION('center_axis',(0.,0.,-1.));
#27859=DIRECTION('ref_axis',(-1.,0.,0.));
#27860=DIRECTION('',(0.,0.,-1.));
#27861=DIRECTION('center_axis',(0.,0.,-1.));
#27862=DIRECTION('ref_axis',(-1.,0.,0.));
#27863=DIRECTION('center_axis',(0.,0.,1.));
#27864=DIRECTION('ref_axis',(-1.,0.,0.));
#27865=DIRECTION('center_axis',(0.,0.,1.));
#27866=DIRECTION('ref_axis',(-1.,0.,0.));
#27867=DIRECTION('',(0.707106781186558,-8.65956056235506E-17,0.707106781186537));
#27868=DIRECTION('center_axis',(0.,0.,1.));
#27869=DIRECTION('ref_axis',(-1.,0.,0.));
#27870=DIRECTION('center_axis',(0.,0.,1.));
#27871=DIRECTION('ref_axis',(1.,0.,0.));
#27872=DIRECTION('center_axis',(0.,0.,-1.));
#27873=DIRECTION('ref_axis',(-1.,0.,0.));
#27874=DIRECTION('center_axis',(0.,0.,-1.));
#27875=DIRECTION('ref_axis',(-1.,0.,0.));
#27876=DIRECTION('',(0.707106781186555,8.65956056235503E-17,-0.70710678118654));
#27877=DIRECTION('center_axis',(0.,0.,1.));
#27878=DIRECTION('ref_axis',(-1.,0.,0.));
#27879=DIRECTION('center_axis',(0.,0.,1.));
#27880=DIRECTION('ref_axis',(-1.,0.,0.));
#27881=DIRECTION('center_axis',(0.,0.,1.));
#27882=DIRECTION('ref_axis',(1.,0.,0.));
#27883=DIRECTION('',(0.,0.,-1.));
#27884=DIRECTION('center_axis',(0.,0.,-1.));
#27885=DIRECTION('ref_axis',(-1.,0.,0.));
#27886=DIRECTION('center_axis',(0.,0.,-1.));
#27887=DIRECTION('ref_axis',(-1.,0.,0.));
#27888=DIRECTION('center_axis',(0.,0.,1.));
#27889=DIRECTION('ref_axis',(-1.,0.,0.));
#27890=DIRECTION('',(-0.707106781186544,-8.65956056235488E-17,-0.707106781186551));
#27891=DIRECTION('axis',(0.,0.,1.));
#27892=DIRECTION('refdir',(1.,0.,0.));
#27893=DIRECTION('center_axis',(0.,0.,1.));
#27894=DIRECTION('ref_axis',(1.,0.,0.));
#27895=DIRECTION('',(-0.857167300702118,-1.04972719113863E-16,0.515038074910044));
#27896=DIRECTION('center_axis',(0.,0.,1.));
#27897=DIRECTION('ref_axis',(1.,0.,0.));
#27898=DIRECTION('center_axis',(0.,0.,1.));
#27899=DIRECTION('ref_axis',(1.,0.,0.));
#27900=DIRECTION('',(0.,0.,1.));
#27901=DIRECTION('center_axis',(0.,0.,1.));
#27902=DIRECTION('ref_axis',(1.,0.,0.));
#27903=DIRECTION('center_axis',(0.,0.,1.));
#27904=DIRECTION('ref_axis',(1.,0.,0.));
#27905=DIRECTION('',(-0.707106781186549,-8.65956056235495E-17,0.707106781186546));
#27906=DIRECTION('center_axis',(0.,0.,-1.));
#27907=DIRECTION('ref_axis',(1.,0.,0.));
#27908=DIRECTION('center_axis',(0.,0.,1.));
#27909=DIRECTION('ref_axis',(1.,0.,0.));
#27910=DIRECTION('',(-0.857167300702118,-1.04972719113863E-16,0.515038074910044));
#27911=DIRECTION('center_axis',(0.,0.,1.));
#27912=DIRECTION('ref_axis',(1.,0.,0.));
#27913=DIRECTION('center_axis',(0.,0.,1.));
#27914=DIRECTION('ref_axis',(1.,0.,0.));
#27915=DIRECTION('',(0.,0.,1.));
#27916=DIRECTION('center_axis',(0.,0.,1.));
#27917=DIRECTION('ref_axis',(1.,0.,0.));
#27918=DIRECTION('center_axis',(0.,0.,1.));
#27919=DIRECTION('ref_axis',(1.,0.,0.));
#27920=DIRECTION('',(-0.707106781186549,-8.65956056235495E-17,0.707106781186546));
#27921=DIRECTION('center_axis',(0.,0.,-1.));
#27922=DIRECTION('ref_axis',(1.,0.,0.));
#27923=DIRECTION('center_axis',(0.,0.,-1.));
#27924=DIRECTION('ref_axis',(-1.,0.,0.));
#27925=DIRECTION('',(0.857167300702116,-1.04972719113862E-16,-0.515038074910048));
#27926=DIRECTION('center_axis',(0.,0.,-1.));
#27927=DIRECTION('ref_axis',(1.,0.,0.));
#27928=DIRECTION('center_axis',(0.,0.,-1.));
#27929=DIRECTION('ref_axis',(-1.,0.,0.));
#27930=DIRECTION('',(0.,0.,-1.));
#27931=DIRECTION('center_axis',(0.,0.,-1.));
#27932=DIRECTION('ref_axis',(1.,0.,0.));
#27933=DIRECTION('center_axis',(0.,0.,-1.));
#27934=DIRECTION('ref_axis',(-1.,0.,0.));
#27935=DIRECTION('',(0.707106781186549,-8.65956056235495E-17,-0.707106781186546));
#27936=DIRECTION('center_axis',(0.,0.,1.));
#27937=DIRECTION('ref_axis',(-1.,0.,0.));
#27938=DIRECTION('center_axis',(0.,0.,-1.));
#27939=DIRECTION('ref_axis',(-1.,0.,0.));
#27940=DIRECTION('',(0.857167300702115,-1.04972719113862E-16,-0.51503807491005));
#27941=DIRECTION('center_axis',(0.,0.,-1.));
#27942=DIRECTION('ref_axis',(1.,0.,0.));
#27943=DIRECTION('center_axis',(0.,0.,-1.));
#27944=DIRECTION('ref_axis',(-1.,0.,0.));
#27945=DIRECTION('',(0.,0.,-1.));
#27946=DIRECTION('center_axis',(0.,0.,-1.));
#27947=DIRECTION('ref_axis',(1.,0.,0.));
#27948=DIRECTION('center_axis',(0.,0.,-1.));
#27949=DIRECTION('ref_axis',(-1.,0.,0.));
#27950=DIRECTION('',(0.707106781186549,-8.65956056235495E-17,-0.707106781186546));
#27951=DIRECTION('center_axis',(0.,0.,1.));
#27952=DIRECTION('ref_axis',(-1.,0.,0.));
#27953=DIRECTION('center_axis',(0.,0.,-1.));
#27954=DIRECTION('ref_axis',(-1.,0.,0.));
#27955=DIRECTION('',(0.857167300702115,-1.04972719113862E-16,-0.515038074910049));
#27956=DIRECTION('center_axis',(0.,0.,-1.));
#27957=DIRECTION('ref_axis',(1.,0.,0.));
#27958=DIRECTION('center_axis',(0.,0.,-1.));
#27959=DIRECTION('ref_axis',(-1.,0.,0.));
#27960=DIRECTION('',(0.,0.,-1.));
#27961=DIRECTION('center_axis',(0.,0.,-1.));
#27962=DIRECTION('ref_axis',(1.,0.,0.));
#27963=DIRECTION('center_axis',(0.,0.,-1.));
#27964=DIRECTION('ref_axis',(-1.,0.,0.));
#27965=DIRECTION('',(0.707106781186549,-8.65956056235495E-17,-0.707106781186546));
#27966=DIRECTION('center_axis',(0.,0.,1.));
#27967=DIRECTION('ref_axis',(-1.,0.,0.));
#27968=DIRECTION('center_axis',(0.,0.,-1.));
#27969=DIRECTION('ref_axis',(1.,0.,0.));
#27970=DIRECTION('center_axis',(0.,0.,1.));
#27971=DIRECTION('ref_axis',(1.,0.,0.));
#27972=DIRECTION('',(0.316227766016828,3.87267321454026E-17,0.948683298050517));
#27973=DIRECTION('center_axis',(0.,0.,1.));
#27974=DIRECTION('ref_axis',(1.,0.,0.));
#27975=DIRECTION('center_axis',(0.,0.,1.));
#27976=DIRECTION('ref_axis',(1.,0.,0.));
#27977=DIRECTION('',(0.,0.,1.));
#27978=DIRECTION('center_axis',(0.,0.,1.));
#27979=DIRECTION('ref_axis',(1.,0.,0.));
#27980=DIRECTION('center_axis',(0.,0.,1.));
#27981=DIRECTION('ref_axis',(1.,0.,0.));
#27982=DIRECTION('',(-0.70710678118656,-8.65956056235509E-17,0.707106781186535));
#27983=DIRECTION('center_axis',(0.,0.,1.));
#27984=DIRECTION('ref_axis',(1.,0.,0.));
#27985=DIRECTION('center_axis',(0.,0.,-1.));
#27986=DIRECTION('ref_axis',(-1.,0.,0.));
#27987=DIRECTION('center_axis',(0.,0.,1.));
#27988=DIRECTION('ref_axis',(1.,0.,0.));
#27989=DIRECTION('center_axis',(0.,0.,1.));
#27990=DIRECTION('ref_axis',(1.,0.,0.));
#27991=DIRECTION('',(0.,0.,1.));
#27992=DIRECTION('center_axis',(0.,0.,-1.));
#27993=DIRECTION('ref_axis',(1.,0.,0.));
#27994=DIRECTION('center_axis',(0.,0.,-1.));
#27995=DIRECTION('ref_axis',(1.,0.,0.));
#27996=DIRECTION('center_axis',(0.,0.,1.));
#27997=DIRECTION('ref_axis',(1.,0.,0.));
#27998=DIRECTION('',(0.316227766016838,3.87267321454039E-17,0.948683298050514));
#27999=DIRECTION('center_axis',(0.,0.,1.));
#28000=DIRECTION('ref_axis',(1.,0.,0.));
#28001=DIRECTION('center_axis',(0.,0.,1.));
#28002=DIRECTION('ref_axis',(1.,0.,0.));
#28003=DIRECTION('',(0.,0.,1.));
#28004=DIRECTION('center_axis',(0.,0.,1.));
#28005=DIRECTION('ref_axis',(1.,0.,0.));
#28006=DIRECTION('center_axis',(0.,0.,1.));
#28007=DIRECTION('ref_axis',(1.,0.,0.));
#28008=DIRECTION('',(-0.707106781186573,-8.65956056235524E-17,0.707106781186522));
#28009=DIRECTION('center_axis',(0.,0.,1.));
#28010=DIRECTION('ref_axis',(1.,0.,0.));
#28011=DIRECTION('center_axis',(0.,0.,-1.));
#28012=DIRECTION('ref_axis',(-1.,0.,0.));
#28013=DIRECTION('center_axis',(0.,0.,1.));
#28014=DIRECTION('ref_axis',(1.,0.,0.));
#28015=DIRECTION('center_axis',(0.,0.,1.));
#28016=DIRECTION('ref_axis',(1.,0.,0.));
#28017=DIRECTION('',(0.,0.,1.));
#28018=DIRECTION('center_axis',(0.,0.,-1.));
#28019=DIRECTION('ref_axis',(1.,0.,0.));
#28020=DIRECTION('center_axis',(0.,0.,-1.));
#28021=DIRECTION('ref_axis',(1.,0.,0.));
#28022=DIRECTION('center_axis',(0.,0.,1.));
#28023=DIRECTION('ref_axis',(1.,0.,0.));
#28024=DIRECTION('',(0.316227766016835,3.87267321454036E-17,0.948683298050515));
#28025=DIRECTION('center_axis',(0.,0.,1.));
#28026=DIRECTION('ref_axis',(1.,0.,0.));
#28027=DIRECTION('center_axis',(0.,0.,1.));
#28028=DIRECTION('ref_axis',(1.,0.,0.));
#28029=DIRECTION('',(0.,0.,1.));
#28030=DIRECTION('center_axis',(0.,0.,1.));
#28031=DIRECTION('ref_axis',(1.,0.,0.));
#28032=DIRECTION('center_axis',(0.,0.,1.));
#28033=DIRECTION('ref_axis',(1.,0.,0.));
#28034=DIRECTION('',(-0.70710678118657,-8.6595605623552E-17,0.707106781186526));
#28035=DIRECTION('center_axis',(0.,0.,1.));
#28036=DIRECTION('ref_axis',(1.,0.,0.));
#28037=DIRECTION('center_axis',(0.,0.,-1.));
#28038=DIRECTION('ref_axis',(-1.,0.,0.));
#28039=DIRECTION('center_axis',(0.,0.,1.));
#28040=DIRECTION('ref_axis',(1.,0.,0.));
#28041=DIRECTION('center_axis',(0.,0.,1.));
#28042=DIRECTION('ref_axis',(1.,0.,0.));
#28043=DIRECTION('',(0.,0.,1.));
#28044=DIRECTION('center_axis',(0.,0.,-1.));
#28045=DIRECTION('ref_axis',(1.,0.,0.));
#28046=DIRECTION('center_axis',(0.,0.,-1.));
#28047=DIRECTION('ref_axis',(1.,0.,0.));
#28048=DIRECTION('center_axis',(0.,0.,1.));
#28049=DIRECTION('ref_axis',(1.,0.,0.));
#28050=DIRECTION('',(0.316227766016833,3.87267321454033E-17,0.948683298050515));
#28051=DIRECTION('center_axis',(0.,0.,1.));
#28052=DIRECTION('ref_axis',(1.,0.,0.));
#28053=DIRECTION('center_axis',(0.,0.,1.));
#28054=DIRECTION('ref_axis',(1.,0.,0.));
#28055=DIRECTION('',(0.,0.,1.));
#28056=DIRECTION('center_axis',(0.,0.,1.));
#28057=DIRECTION('ref_axis',(1.,0.,0.));
#28058=DIRECTION('center_axis',(0.,0.,1.));
#28059=DIRECTION('ref_axis',(1.,0.,0.));
#28060=DIRECTION('',(-0.707106781186566,-8.65956056235516E-17,0.707106781186529));
#28061=DIRECTION('center_axis',(0.,0.,1.));
#28062=DIRECTION('ref_axis',(1.,0.,0.));
#28063=DIRECTION('center_axis',(0.,0.,-1.));
#28064=DIRECTION('ref_axis',(-1.,0.,0.));
#28065=DIRECTION('center_axis',(0.,0.,1.));
#28066=DIRECTION('ref_axis',(1.,0.,0.));
#28067=DIRECTION('center_axis',(0.,0.,1.));
#28068=DIRECTION('ref_axis',(1.,0.,0.));
#28069=DIRECTION('',(0.,0.,1.));
#28070=DIRECTION('center_axis',(0.,0.,-1.));
#28071=DIRECTION('ref_axis',(1.,0.,0.));
#28072=DIRECTION('center_axis',(0.,0.,-1.));
#28073=DIRECTION('ref_axis',(1.,0.,0.));
#28074=DIRECTION('center_axis',(0.,0.,1.));
#28075=DIRECTION('ref_axis',(1.,0.,0.));
#28076=DIRECTION('',(0.316227766016833,3.87267321454033E-17,0.948683298050515));
#28077=DIRECTION('center_axis',(0.,0.,1.));
#28078=DIRECTION('ref_axis',(1.,0.,0.));
#28079=DIRECTION('center_axis',(0.,0.,1.));
#28080=DIRECTION('ref_axis',(1.,0.,0.));
#28081=DIRECTION('',(0.,0.,1.));
#28082=DIRECTION('center_axis',(0.,0.,1.));
#28083=DIRECTION('ref_axis',(1.,0.,0.));
#28084=DIRECTION('center_axis',(0.,0.,1.));
#28085=DIRECTION('ref_axis',(1.,0.,0.));
#28086=DIRECTION('',(-0.707106781186566,-8.65956056235516E-17,0.707106781186529));
#28087=DIRECTION('center_axis',(0.,0.,1.));
#28088=DIRECTION('ref_axis',(1.,0.,0.));
#28089=DIRECTION('center_axis',(0.,0.,-1.));
#28090=DIRECTION('ref_axis',(-1.,0.,0.));
#28091=DIRECTION('center_axis',(0.,0.,1.));
#28092=DIRECTION('ref_axis',(1.,0.,0.));
#28093=DIRECTION('center_axis',(0.,0.,1.));
#28094=DIRECTION('ref_axis',(1.,0.,0.));
#28095=DIRECTION('',(0.,0.,1.));
#28096=DIRECTION('center_axis',(0.,0.,-1.));
#28097=DIRECTION('ref_axis',(1.,0.,0.));
#28098=DIRECTION('center_axis',(0.,0.,-1.));
#28099=DIRECTION('ref_axis',(1.,0.,0.));
#28100=DIRECTION('center_axis',(0.,0.,1.));
#28101=DIRECTION('ref_axis',(1.,0.,0.));
#28102=DIRECTION('',(0.316227766016828,3.87267321454026E-17,0.948683298050517));
#28103=DIRECTION('center_axis',(0.,0.,1.));
#28104=DIRECTION('ref_axis',(1.,0.,0.));
#28105=DIRECTION('center_axis',(0.,0.,1.));
#28106=DIRECTION('ref_axis',(1.,0.,0.));
#28107=DIRECTION('',(0.,0.,1.));
#28108=DIRECTION('center_axis',(0.,0.,1.));
#28109=DIRECTION('ref_axis',(1.,0.,0.));
#28110=DIRECTION('center_axis',(0.,0.,1.));
#28111=DIRECTION('ref_axis',(1.,0.,0.));
#28112=DIRECTION('',(-0.70710678118656,-8.65956056235509E-17,0.707106781186535));
#28113=DIRECTION('center_axis',(0.,0.,1.));
#28114=DIRECTION('ref_axis',(1.,0.,0.));
#28115=DIRECTION('center_axis',(0.,0.,-1.));
#28116=DIRECTION('ref_axis',(-1.,0.,0.));
#28117=DIRECTION('center_axis',(0.,0.,1.));
#28118=DIRECTION('ref_axis',(1.,0.,0.));
#28119=DIRECTION('center_axis',(0.,0.,1.));
#28120=DIRECTION('ref_axis',(1.,0.,0.));
#28121=DIRECTION('',(0.,0.,1.));
#28122=DIRECTION('center_axis',(0.,0.,-1.));
#28123=DIRECTION('ref_axis',(1.,0.,0.));
#28124=DIRECTION('center_axis',(0.,0.,-1.));
#28125=DIRECTION('ref_axis',(1.,0.,0.));
#28126=DIRECTION('center_axis',(0.,0.,1.));
#28127=DIRECTION('ref_axis',(1.,0.,0.));
#28128=DIRECTION('',(0.316227766016838,3.87267321454039E-17,0.948683298050514));
#28129=DIRECTION('center_axis',(0.,0.,1.));
#28130=DIRECTION('ref_axis',(1.,0.,0.));
#28131=DIRECTION('center_axis',(0.,0.,1.));
#28132=DIRECTION('ref_axis',(1.,0.,0.));
#28133=DIRECTION('',(0.,0.,1.));
#28134=DIRECTION('center_axis',(0.,0.,1.));
#28135=DIRECTION('ref_axis',(1.,0.,0.));
#28136=DIRECTION('center_axis',(0.,0.,1.));
#28137=DIRECTION('ref_axis',(1.,0.,0.));
#28138=DIRECTION('',(-0.707106781186573,-8.65956056235524E-17,0.707106781186522));
#28139=DIRECTION('center_axis',(0.,0.,1.));
#28140=DIRECTION('ref_axis',(1.,0.,0.));
#28141=DIRECTION('center_axis',(0.,0.,-1.));
#28142=DIRECTION('ref_axis',(-1.,0.,0.));
#28143=DIRECTION('center_axis',(0.,0.,1.));
#28144=DIRECTION('ref_axis',(1.,0.,0.));
#28145=DIRECTION('center_axis',(0.,0.,1.));
#28146=DIRECTION('ref_axis',(1.,0.,0.));
#28147=DIRECTION('',(0.,0.,1.));
#28148=DIRECTION('center_axis',(0.,0.,-1.));
#28149=DIRECTION('ref_axis',(1.,0.,0.));
#28150=DIRECTION('center_axis',(0.,0.,-1.));
#28151=DIRECTION('ref_axis',(1.,0.,0.));
#28152=DIRECTION('center_axis',(0.,0.,1.));
#28153=DIRECTION('ref_axis',(1.,0.,0.));
#28154=DIRECTION('',(0.316227766016833,3.87267321454033E-17,0.948683298050516));
#28155=DIRECTION('center_axis',(0.,0.,1.));
#28156=DIRECTION('ref_axis',(1.,0.,0.));
#28157=DIRECTION('center_axis',(0.,0.,1.));
#28158=DIRECTION('ref_axis',(1.,0.,0.));
#28159=DIRECTION('',(0.,0.,1.));
#28160=DIRECTION('center_axis',(0.,0.,1.));
#28161=DIRECTION('ref_axis',(1.,0.,0.));
#28162=DIRECTION('center_axis',(0.,0.,1.));
#28163=DIRECTION('ref_axis',(1.,0.,0.));
#28164=DIRECTION('',(-0.707106781186566,-8.65956056235516E-17,0.707106781186529));
#28165=DIRECTION('center_axis',(0.,0.,1.));
#28166=DIRECTION('ref_axis',(1.,0.,0.));
#28167=DIRECTION('center_axis',(0.,0.,-1.));
#28168=DIRECTION('ref_axis',(-1.,0.,0.));
#28169=DIRECTION('center_axis',(0.,0.,1.));
#28170=DIRECTION('ref_axis',(1.,0.,0.));
#28171=DIRECTION('center_axis',(0.,0.,1.));
#28172=DIRECTION('ref_axis',(1.,0.,0.));
#28173=DIRECTION('',(0.,0.,1.));
#28174=DIRECTION('center_axis',(0.,0.,-1.));
#28175=DIRECTION('ref_axis',(1.,0.,0.));
#28176=DIRECTION('center_axis',(0.,0.,-1.));
#28177=DIRECTION('ref_axis',(1.,0.,0.));
#28178=DIRECTION('center_axis',(0.,0.,1.));
#28179=DIRECTION('ref_axis',(1.,0.,0.));
#28180=DIRECTION('',(0.316227766016833,3.87267321454033E-17,0.948683298050515));
#28181=DIRECTION('center_axis',(0.,0.,1.));
#28182=DIRECTION('ref_axis',(1.,0.,0.));
#28183=DIRECTION('center_axis',(0.,0.,1.));
#28184=DIRECTION('ref_axis',(1.,0.,0.));
#28185=DIRECTION('',(0.,0.,1.));
#28186=DIRECTION('center_axis',(0.,0.,1.));
#28187=DIRECTION('ref_axis',(1.,0.,0.));
#28188=DIRECTION('center_axis',(0.,0.,1.));
#28189=DIRECTION('ref_axis',(1.,0.,0.));
#28190=DIRECTION('',(-0.707106781186566,-8.65956056235516E-17,0.707106781186529));
#28191=DIRECTION('center_axis',(0.,0.,1.));
#28192=DIRECTION('ref_axis',(1.,0.,0.));
#28193=DIRECTION('center_axis',(0.,0.,-1.));
#28194=DIRECTION('ref_axis',(-1.,0.,0.));
#28195=DIRECTION('center_axis',(0.,0.,1.));
#28196=DIRECTION('ref_axis',(1.,0.,0.));
#28197=DIRECTION('center_axis',(0.,0.,1.));
#28198=DIRECTION('ref_axis',(1.,0.,0.));
#28199=DIRECTION('',(0.,0.,1.));
#28200=DIRECTION('center_axis',(0.,0.,-1.));
#28201=DIRECTION('ref_axis',(1.,0.,0.));
#28202=DIRECTION('center_axis',(0.,0.,-1.));
#28203=DIRECTION('ref_axis',(1.,0.,0.));
#28204=DIRECTION('center_axis',(0.,0.,1.));
#28205=DIRECTION('ref_axis',(1.,0.,0.));
#28206=DIRECTION('',(0.316227766016835,3.87267321454036E-17,0.948683298050515));
#28207=DIRECTION('center_axis',(0.,0.,1.));
#28208=DIRECTION('ref_axis',(1.,0.,0.));
#28209=DIRECTION('center_axis',(0.,0.,1.));
#28210=DIRECTION('ref_axis',(1.,0.,0.));
#28211=DIRECTION('',(0.,0.,1.));
#28212=DIRECTION('center_axis',(0.,0.,1.));
#28213=DIRECTION('ref_axis',(1.,0.,0.));
#28214=DIRECTION('center_axis',(0.,0.,1.));
#28215=DIRECTION('ref_axis',(1.,0.,0.));
#28216=DIRECTION('',(-0.70710678118657,-8.6595605623552E-17,0.707106781186526));
#28217=DIRECTION('center_axis',(0.,0.,1.));
#28218=DIRECTION('ref_axis',(1.,0.,0.));
#28219=DIRECTION('center_axis',(0.,0.,-1.));
#28220=DIRECTION('ref_axis',(-1.,0.,0.));
#28221=DIRECTION('center_axis',(0.,0.,1.));
#28222=DIRECTION('ref_axis',(1.,0.,0.));
#28223=DIRECTION('center_axis',(0.,0.,1.));
#28224=DIRECTION('ref_axis',(1.,0.,0.));
#28225=DIRECTION('',(0.,0.,1.));
#28226=DIRECTION('center_axis',(0.,0.,-1.));
#28227=DIRECTION('ref_axis',(1.,0.,0.));
#28228=DIRECTION('center_axis',(0.,0.,-1.));
#28229=DIRECTION('ref_axis',(1.,0.,0.));
#28230=DIRECTION('center_axis',(0.,0.,1.));
#28231=DIRECTION('ref_axis',(1.,0.,0.));
#28232=DIRECTION('',(0.316227766016833,3.87267321454033E-17,0.948683298050515));
#28233=DIRECTION('center_axis',(0.,0.,1.));
#28234=DIRECTION('ref_axis',(1.,0.,0.));
#28235=DIRECTION('center_axis',(0.,0.,1.));
#28236=DIRECTION('ref_axis',(1.,0.,0.));
#28237=DIRECTION('',(0.,0.,1.));
#28238=DIRECTION('center_axis',(0.,0.,1.));
#28239=DIRECTION('ref_axis',(1.,0.,0.));
#28240=DIRECTION('center_axis',(0.,0.,1.));
#28241=DIRECTION('ref_axis',(1.,0.,0.));
#28242=DIRECTION('',(-0.707106781186566,-8.65956056235516E-17,0.707106781186529));
#28243=DIRECTION('center_axis',(0.,0.,1.));
#28244=DIRECTION('ref_axis',(1.,0.,0.));
#28245=DIRECTION('center_axis',(0.,0.,-1.));
#28246=DIRECTION('ref_axis',(-1.,0.,0.));
#28247=DIRECTION('center_axis',(0.,0.,1.));
#28248=DIRECTION('ref_axis',(1.,0.,0.));
#28249=DIRECTION('center_axis',(0.,0.,1.));
#28250=DIRECTION('ref_axis',(1.,0.,0.));
#28251=DIRECTION('',(0.,0.,1.));
#28252=DIRECTION('center_axis',(0.,0.,-1.));
#28253=DIRECTION('ref_axis',(1.,0.,0.));
#28254=DIRECTION('center_axis',(0.,0.,-1.));
#28255=DIRECTION('ref_axis',(1.,0.,0.));
#28256=DIRECTION('center_axis',(0.,0.,1.));
#28257=DIRECTION('ref_axis',(1.,0.,0.));
#28258=DIRECTION('',(0.316227766016828,3.87267321454026E-17,0.948683298050517));
#28259=DIRECTION('center_axis',(0.,0.,1.));
#28260=DIRECTION('ref_axis',(1.,0.,0.));
#28261=DIRECTION('center_axis',(0.,0.,1.));
#28262=DIRECTION('ref_axis',(1.,0.,0.));
#28263=DIRECTION('',(0.,0.,1.));
#28264=DIRECTION('center_axis',(0.,0.,1.));
#28265=DIRECTION('ref_axis',(1.,0.,0.));
#28266=DIRECTION('center_axis',(0.,0.,1.));
#28267=DIRECTION('ref_axis',(1.,0.,0.));
#28268=DIRECTION('',(-0.70710678118656,-8.65956056235509E-17,0.707106781186535));
#28269=DIRECTION('center_axis',(0.,0.,1.));
#28270=DIRECTION('ref_axis',(1.,0.,0.));
#28271=DIRECTION('center_axis',(0.,0.,-1.));
#28272=DIRECTION('ref_axis',(-1.,0.,0.));
#28273=DIRECTION('center_axis',(0.,0.,1.));
#28274=DIRECTION('ref_axis',(1.,0.,0.));
#28275=DIRECTION('center_axis',(0.,0.,1.));
#28276=DIRECTION('ref_axis',(1.,0.,0.));
#28277=DIRECTION('',(0.,0.,1.));
#28278=DIRECTION('center_axis',(0.,0.,-1.));
#28279=DIRECTION('ref_axis',(1.,0.,0.));
#28280=DIRECTION('center_axis',(0.,0.,-1.));
#28281=DIRECTION('ref_axis',(-1.,0.,0.));
#28282=DIRECTION('center_axis',(0.,0.,-1.));
#28283=DIRECTION('ref_axis',(-1.,0.,0.));
#28284=DIRECTION('',(-0.707106781186555,8.65956056235503E-17,0.70710678118654));
#28285=DIRECTION('center_axis',(0.,0.,1.));
#28286=DIRECTION('ref_axis',(-1.,0.,0.));
#28287=DIRECTION('center_axis',(0.,0.,1.));
#28288=DIRECTION('ref_axis',(-1.,0.,0.));
#28289=DIRECTION('center_axis',(0.,0.,1.));
#28290=DIRECTION('ref_axis',(1.,0.,0.));
#28291=DIRECTION('center_axis',(0.,0.,-1.));
#28292=DIRECTION('ref_axis',(-1.,0.,0.));
#28293=DIRECTION('center_axis',(0.,0.,-1.));
#28294=DIRECTION('ref_axis',(-1.,0.,0.));
#28295=DIRECTION('',(0.,0.,-1.));
#28296=DIRECTION('center_axis',(0.,0.,-1.));
#28297=DIRECTION('ref_axis',(-1.,0.,0.));
#28298=DIRECTION('center_axis',(0.,0.,1.));
#28299=DIRECTION('ref_axis',(1.,0.,0.));
#28300=DIRECTION('center_axis',(0.,0.,1.));
#28301=DIRECTION('ref_axis',(-1.,0.,0.));
#28302=DIRECTION('',(0.707106781186555,-8.65956056235503E-17,0.70710678118654));
#28303=DIRECTION('center_axis',(0.,0.,1.));
#28304=DIRECTION('ref_axis',(-1.,0.,0.));
#28305=DIRECTION('center_axis',(0.,0.,1.));
#28306=DIRECTION('ref_axis',(1.,0.,0.));
#28307=DIRECTION('center_axis',(0.,0.,1.));
#28308=DIRECTION('ref_axis',(1.,0.,0.));
#28309=DIRECTION('center_axis',(0.,0.,1.));
#28310=DIRECTION('ref_axis',(-1.,0.,0.));
#28311=DIRECTION('center_axis',(0.,0.,-1.));
#28312=DIRECTION('ref_axis',(-1.,0.,0.));
#28313=DIRECTION('center_axis',(0.,0.,-1.));
#28314=DIRECTION('ref_axis',(-1.,0.,0.));
#28315=DIRECTION('',(-0.707106781186558,-8.65956056235506E-17,-0.707106781186537));
#28316=DIRECTION('center_axis',(0.,0.,1.));
#28317=DIRECTION('ref_axis',(-1.,0.,0.));
#28318=DIRECTION('center_axis',(0.,0.,1.));
#28319=DIRECTION('ref_axis',(1.,0.,0.));
#28320=DIRECTION('center_axis',(0.,0.,1.));
#28321=DIRECTION('ref_axis',(-1.,0.,0.));
#28322=DIRECTION('center_axis',(0.,0.,1.));
#28323=DIRECTION('ref_axis',(-1.,0.,0.));
#28324=DIRECTION('',(0.,0.,-1.));
#28325=DIRECTION('center_axis',(0.,0.,-1.));
#28326=DIRECTION('ref_axis',(-1.,0.,0.));
#28327=DIRECTION('center_axis',(0.,0.,1.));
#28328=DIRECTION('ref_axis',(1.,0.,0.));
#28329=DIRECTION('center_axis',(0.,0.,-1.));
#28330=DIRECTION('ref_axis',(-1.,0.,0.));
#28331=DIRECTION('center_axis',(0.,0.,-1.));
#28332=DIRECTION('ref_axis',(-1.,0.,0.));
#28333=DIRECTION('',(0.707106781186558,8.65956056235506E-17,-0.707106781186537));
#28334=DIRECTION('center_axis',(0.,0.,1.));
#28335=DIRECTION('ref_axis',(1.,0.,0.));
#28336=DIRECTION('',(0.5,-0.866025403784439,0.));
#28337=DIRECTION('center_axis',(0.,0.,1.));
#28338=DIRECTION('ref_axis',(0.866025403784439,-0.499999999999999,0.));
#28339=DIRECTION('',(-1.,0.,0.));
#28340=DIRECTION('center_axis',(0.,0.,1.));
#28341=DIRECTION('ref_axis',(1.,0.,0.));
#28342=DIRECTION('center_axis',(0.,0.,1.));
#28343=DIRECTION('ref_axis',(-0.425897586725943,0.904771377542978,0.));
#28344=DIRECTION('center_axis',(0.,0.,1.));
#28345=DIRECTION('ref_axis',(1.,0.,0.));
#28346=DIRECTION('',(1.,0.,0.));
#28347=DIRECTION('center_axis',(0.,0.,1.));
#28348=DIRECTION('ref_axis',(0.866025403784438,0.500000000000002,0.));
#28349=DIRECTION('',(-0.5,-0.866025403784439,0.));
#28350=DIRECTION('center_axis',(0.,0.,1.));
#28351=DIRECTION('ref_axis',(-0.425897586725943,-0.904771377542978,0.));
#28352=DIRECTION('',(0.5,0.866025403784439,0.));
#28353=DIRECTION('center_axis',(0.,0.,1.));
#28354=DIRECTION('ref_axis',(0.,1.,0.));
#28355=DIRECTION('',(0.5,-0.866025403784439,0.));
#28356=DIRECTION('center_axis',(0.,0.,1.));
#28357=DIRECTION('ref_axis',(0.570606204206288,-0.821223818286642,0.));
#28358=DIRECTION('center_axis',(0.,0.,1.));
#28359=DIRECTION('ref_axis',(1.,0.,0.));
#28360=DIRECTION('center_axis',(0.,0.,1.));
#28361=DIRECTION('ref_axis',(1.,0.,0.));
#28362=DIRECTION('center_axis',(0.,0.,1.));
#28363=DIRECTION('ref_axis',(0.570606204206288,0.821223818286642,0.));
#28364=DIRECTION('',(-0.5,-0.866025403784439,0.));
#28365=DIRECTION('center_axis',(0.,0.,1.));
#28366=DIRECTION('ref_axis',(0.,-1.,0.));
#28367=DIRECTION('',(-0.5,0.866025403784439,0.));
#28368=DIRECTION('',(1.,0.,0.));
#28369=DIRECTION('center_axis',(0.,0.,1.));
#28370=DIRECTION('ref_axis',(0.86602540378444,0.499999999999997,0.));
#28371=DIRECTION('',(-0.5,-0.866025403784439,0.));
#28372=DIRECTION('center_axis',(0.,0.,1.));
#28373=DIRECTION('ref_axis',(1.,0.,0.));
#28374=DIRECTION('center_axis',(0.,0.,1.));
#28375=DIRECTION('ref_axis',(-0.996503790932232,0.0835475592563362,0.));
#28376=DIRECTION('center_axis',(0.,0.,1.));
#28377=DIRECTION('ref_axis',(1.,0.,0.));
#28378=DIRECTION('',(0.5,-0.866025403784439,0.));
#28379=DIRECTION('center_axis',(0.,0.,1.));
#28380=DIRECTION('ref_axis',(0.866025403784437,-0.500000000000003,0.));
#28381=DIRECTION('',(-1.,0.,0.));
#28382=DIRECTION('center_axis',(0.,0.,1.));
#28383=DIRECTION('ref_axis',(-0.996503790932232,-0.0835475592563325,0.));
#28384=DIRECTION('',(-0.5,0.866025403784439,0.));
#28385=DIRECTION('center_axis',(0.,0.,1.));
#28386=DIRECTION('ref_axis',(-0.866025403784437,0.500000000000003,0.));
#28387=DIRECTION('',(1.,0.,0.));
#28388=DIRECTION('center_axis',(0.,0.,1.));
#28389=DIRECTION('ref_axis',(0.996503790932232,0.0835475592563325,0.));
#28390=DIRECTION('center_axis',(0.,0.,1.));
#28391=DIRECTION('ref_axis',(1.,0.,0.));
#28392=DIRECTION('center_axis',(0.,0.,1.));
#28393=DIRECTION('ref_axis',(1.,0.,0.));
#28394=DIRECTION('center_axis',(0.,0.,1.));
#28395=DIRECTION('ref_axis',(0.996503790932232,-0.0835475592563362,0.));
#28396=DIRECTION('',(-1.,0.,0.));
#28397=DIRECTION('center_axis',(0.,0.,1.));
#28398=DIRECTION('ref_axis',(-0.86602540378444,-0.499999999999997,0.));
#28399=DIRECTION('',(0.5,0.866025403784439,0.));
#28400=DIRECTION('',(0.5,0.866025403784439,0.));
#28401=DIRECTION('center_axis',(0.,0.,1.));
#28402=DIRECTION('ref_axis',(0.,1.,0.));
#28403=DIRECTION('',(0.5,-0.866025403784439,0.));
#28404=DIRECTION('center_axis',(0.,0.,1.));
#28405=DIRECTION('ref_axis',(1.,0.,0.));
#28406=DIRECTION('center_axis',(0.,0.,1.));
#28407=DIRECTION('ref_axis',(-0.570606204206288,-0.821223818286642,0.));
#28408=DIRECTION('center_axis',(0.,0.,1.));
#28409=DIRECTION('ref_axis',(1.,0.,0.));
#28410=DIRECTION('',(-0.5,-0.866025403784439,0.));
#28411=DIRECTION('center_axis',(0.,0.,1.));
#28412=DIRECTION('ref_axis',(0.,-1.,0.));
#28413=DIRECTION('',(-0.5,0.866025403784439,0.));
#28414=DIRECTION('center_axis',(0.,0.,1.));
#28415=DIRECTION('ref_axis',(-0.570606204206288,0.821223818286642,0.));
#28416=DIRECTION('',(-1.,0.,0.));
#28417=DIRECTION('center_axis',(0.,0.,1.));
#28418=DIRECTION('ref_axis',(-0.866025403784438,-0.500000000000002,0.));
#28419=DIRECTION('',(0.5,0.866025403784439,0.));
#28420=DIRECTION('center_axis',(0.,0.,1.));
#28421=DIRECTION('ref_axis',(0.425897586725943,0.904771377542978,0.));
#28422=DIRECTION('center_axis',(0.,0.,1.));
#28423=DIRECTION('ref_axis',(1.,0.,0.));
#28424=DIRECTION('center_axis',(0.,0.,1.));
#28425=DIRECTION('ref_axis',(1.,0.,0.));
#28426=DIRECTION('center_axis',(0.,0.,1.));
#28427=DIRECTION('ref_axis',(0.425897586725943,-0.904771377542978,0.));
#28428=DIRECTION('',(-0.5,0.866025403784439,0.));
#28429=DIRECTION('center_axis',(0.,0.,1.));
#28430=DIRECTION('ref_axis',(-0.866025403784439,0.499999999999999,0.));
#28431=DIRECTION('',(1.,0.,0.));
#28432=DIRECTION('',(-1.,0.,0.));
#28433=DIRECTION('center_axis',(0.,0.,1.));
#28434=DIRECTION('ref_axis',(-0.866025403784441,-0.499999999999996,0.));
#28435=DIRECTION('',(0.5,0.866025403784439,0.));
#28436=DIRECTION('center_axis',(0.,0.,1.));
#28437=DIRECTION('ref_axis',(0.,1.,0.));
#28438=DIRECTION('',(0.5,-0.866025403784439,0.));
#28439=DIRECTION('center_axis',(0.,0.,1.));
#28440=DIRECTION('ref_axis',(0.86602540378444,-0.499999999999997,0.));
#28441=DIRECTION('',(-1.,0.,0.));
#28442=DIRECTION('center_axis',(0.,0.,1.));
#28443=DIRECTION('ref_axis',(-0.86602540378444,-0.499999999999997,0.));
#28444=DIRECTION('',(0.5,0.866025403784439,0.));
#28445=DIRECTION('center_axis',(0.,0.,1.));
#28446=DIRECTION('ref_axis',(3.70074341541719E-15,1.,0.));
#28447=DIRECTION('',(0.5,-0.866025403784439,0.));
#28448=DIRECTION('center_axis',(0.,0.,1.));
#28449=DIRECTION('ref_axis',(0.866025403784439,-0.499999999999999,0.));
#28450=DIRECTION('',(-1.,0.,0.));
#28451=DIRECTION('center_axis',(0.,0.,1.));
#28452=DIRECTION('ref_axis',(-0.86602540378444,-0.499999999999998,0.));
#28453=DIRECTION('',(0.5,0.866025403784439,0.));
#28454=DIRECTION('center_axis',(0.,0.,1.));
#28455=DIRECTION('ref_axis',(-1.85037170770859E-15,1.,0.));
#28456=DIRECTION('',(0.5,-0.866025403784439,0.));
#28457=DIRECTION('center_axis',(0.,0.,1.));
#28458=DIRECTION('ref_axis',(0.86602540378444,-0.499999999999997,0.));
#28459=DIRECTION('',(-0.5,-0.866025403784439,0.));
#28460=DIRECTION('center_axis',(0.,0.,1.));
#28461=DIRECTION('ref_axis',(0.,-1.,0.));
#28462=DIRECTION('',(-0.5,0.866025403784439,0.));
#28463=DIRECTION('center_axis',(0.,0.,1.));
#28464=DIRECTION('ref_axis',(-0.86602540378444,0.499999999999997,0.));
#28465=DIRECTION('',(1.,0.,0.));
#28466=DIRECTION('center_axis',(0.,0.,1.));
#28467=DIRECTION('ref_axis',(0.866025403784439,0.499999999999999,0.));
#28468=DIRECTION('',(-1.,0.,0.));
#28469=DIRECTION('center_axis',(0.,0.,1.));
#28470=DIRECTION('ref_axis',(-0.86602540378444,-0.499999999999997,0.));
#28471=DIRECTION('',(0.5,0.866025403784439,0.));
#28472=DIRECTION('center_axis',(0.,0.,1.));
#28473=DIRECTION('ref_axis',(0.,1.,0.));
#28474=DIRECTION('',(0.5,-0.866025403784439,0.));
#28475=DIRECTION('center_axis',(0.,0.,1.));
#28476=DIRECTION('ref_axis',(0.86602540378444,-0.499999999999997,0.));
#28477=DIRECTION('',(-0.5,-0.866025403784439,0.));
#28478=DIRECTION('center_axis',(0.,0.,1.));
#28479=DIRECTION('ref_axis',(0.,-1.,0.));
#28480=DIRECTION('',(-0.5,0.866025403784439,0.));
#28481=DIRECTION('center_axis',(0.,0.,1.));
#28482=DIRECTION('ref_axis',(-0.86602540378444,0.499999999999997,0.));
#28483=DIRECTION('',(1.,0.,0.));
#28484=DIRECTION('center_axis',(0.,0.,1.));
#28485=DIRECTION('ref_axis',(0.86602540378444,0.499999999999997,0.));
#28486=DIRECTION('',(-1.,0.,0.));
#28487=DIRECTION('center_axis',(0.,0.,1.));
#28488=DIRECTION('ref_axis',(-0.866025403784439,-0.499999999999999,0.));
#28489=DIRECTION('',(0.5,0.866025403784439,0.));
#28490=DIRECTION('center_axis',(0.,0.,1.));
#28491=DIRECTION('ref_axis',(0.,1.,0.));
#28492=DIRECTION('',(0.5,-0.866025403784439,0.));
#28493=DIRECTION('center_axis',(0.,0.,1.));
#28494=DIRECTION('ref_axis',(0.86602540378444,-0.499999999999997,0.));
#28495=DIRECTION('',(-0.5,-0.866025403784439,0.));
#28496=DIRECTION('center_axis',(0.,0.,1.));
#28497=DIRECTION('ref_axis',(1.85037170770859E-15,-1.,0.));
#28498=DIRECTION('',(-0.5,0.866025403784439,0.));
#28499=DIRECTION('center_axis',(0.,0.,1.));
#28500=DIRECTION('ref_axis',(-0.86602540378444,0.499999999999997,0.));
#28501=DIRECTION('',(1.,0.,0.));
#28502=DIRECTION('center_axis',(0.,0.,1.));
#28503=DIRECTION('ref_axis',(0.86602540378444,0.499999999999998,0.));
#28504=DIRECTION('',(-0.5,-0.866025403784439,0.));
#28505=DIRECTION('center_axis',(0.,0.,1.));
#28506=DIRECTION('ref_axis',(-3.70074341541719E-15,-1.,0.));
#28507=DIRECTION('',(-0.5,0.866025403784439,0.));
#28508=DIRECTION('center_axis',(0.,0.,1.));
#28509=DIRECTION('ref_axis',(-0.866025403784439,0.499999999999999,0.));
#28510=DIRECTION('',(1.,0.,0.));
#28511=DIRECTION('center_axis',(0.,0.,1.));
#28512=DIRECTION('ref_axis',(0.86602540378444,0.499999999999997,0.));
#28513=DIRECTION('',(-0.5,-0.866025403784439,0.));
#28514=DIRECTION('center_axis',(0.,0.,1.));
#28515=DIRECTION('ref_axis',(0.,-1.,0.));
#28516=DIRECTION('',(-0.5,0.866025403784439,0.));
#28517=DIRECTION('center_axis',(0.,0.,1.));
#28518=DIRECTION('ref_axis',(-0.86602540378444,0.499999999999997,0.));
#28519=DIRECTION('',(1.,0.,0.));
#28520=DIRECTION('center_axis',(0.,0.,1.));
#28521=DIRECTION('ref_axis',(0.866025403784441,0.499999999999996,0.));
#28522=DIRECTION('',(-1.,0.,0.));
#28523=DIRECTION('center_axis',(0.,0.,1.));
#28524=DIRECTION('ref_axis',(-0.866025403784441,-0.499999999999996,0.));
#28525=DIRECTION('',(0.5,0.866025403784439,0.));
#28526=DIRECTION('center_axis',(0.,0.,1.));
#28527=DIRECTION('ref_axis',(0.,1.,0.));
#28528=DIRECTION('',(0.5,-0.866025403784439,0.));
#28529=DIRECTION('center_axis',(0.,0.,1.));
#28530=DIRECTION('ref_axis',(0.86602540378444,-0.499999999999997,0.));
#28531=DIRECTION('',(-1.,0.,0.));
#28532=DIRECTION('center_axis',(0.,0.,1.));
#28533=DIRECTION('ref_axis',(-0.866025403784439,-0.499999999999999,0.));
#28534=DIRECTION('',(0.5,0.866025403784439,0.));
#28535=DIRECTION('center_axis',(0.,0.,1.));
#28536=DIRECTION('ref_axis',(0.,1.,0.));
#28537=DIRECTION('',(0.5,-0.866025403784439,0.));
#28538=DIRECTION('center_axis',(0.,0.,1.));
#28539=DIRECTION('ref_axis',(0.866025403784439,-0.5,0.));
#28540=DIRECTION('',(-0.5,-0.866025403784439,0.));
#28541=DIRECTION('center_axis',(0.,0.,1.));
#28542=DIRECTION('ref_axis',(0.,-1.,0.));
#28543=DIRECTION('',(-0.5,0.866025403784439,0.));
#28544=DIRECTION('center_axis',(0.,0.,1.));
#28545=DIRECTION('ref_axis',(-0.866025403784438,0.500000000000002,0.));
#28546=DIRECTION('',(1.,0.,0.));
#28547=DIRECTION('center_axis',(0.,0.,1.));
#28548=DIRECTION('ref_axis',(0.866025403784439,0.5,0.));
#28549=DIRECTION('',(-1.,0.,0.));
#28550=DIRECTION('center_axis',(0.,0.,1.));
#28551=DIRECTION('ref_axis',(-0.86602540378444,-0.499999999999997,0.));
#28552=DIRECTION('',(0.5,0.866025403784439,0.));
#28553=DIRECTION('center_axis',(0.,0.,1.));
#28554=DIRECTION('ref_axis',(-6.93889390390722E-16,1.,0.));
#28555=DIRECTION('',(0.5,-0.866025403784439,0.));
#28556=DIRECTION('center_axis',(0.,0.,1.));
#28557=DIRECTION('ref_axis',(0.866025403784439,-0.5,0.));
#28558=DIRECTION('',(-0.5,-0.866025403784439,0.));
#28559=DIRECTION('center_axis',(0.,0.,1.));
#28560=DIRECTION('ref_axis',(6.93889390390722E-16,-1.,0.));
#28561=DIRECTION('',(-0.5,0.866025403784439,0.));
#28562=DIRECTION('center_axis',(0.,0.,1.));
#28563=DIRECTION('ref_axis',(-0.866025403784439,0.5,0.));
#28564=DIRECTION('',(1.,0.,0.));
#28565=DIRECTION('center_axis',(0.,0.,1.));
#28566=DIRECTION('ref_axis',(0.86602540378444,0.499999999999997,0.));
#28567=DIRECTION('',(-1.,0.,0.));
#28568=DIRECTION('center_axis',(0.,0.,1.));
#28569=DIRECTION('ref_axis',(-0.866025403784439,-0.5,0.));
#28570=DIRECTION('',(0.5,0.866025403784439,0.));
#28571=DIRECTION('center_axis',(0.,0.,1.));
#28572=DIRECTION('ref_axis',(0.,1.,0.));
#28573=DIRECTION('',(0.5,-0.866025403784439,0.));
#28574=DIRECTION('center_axis',(0.,0.,1.));
#28575=DIRECTION('ref_axis',(0.866025403784438,-0.500000000000002,0.));
#28576=DIRECTION('',(-0.5,-0.866025403784439,0.));
#28577=DIRECTION('center_axis',(0.,0.,1.));
#28578=DIRECTION('ref_axis',(0.,-1.,0.));
#28579=DIRECTION('',(-0.5,0.866025403784439,0.));
#28580=DIRECTION('center_axis',(0.,0.,1.));
#28581=DIRECTION('ref_axis',(-0.866025403784439,0.5,0.));
#28582=DIRECTION('',(1.,0.,0.));
#28583=DIRECTION('center_axis',(0.,0.,1.));
#28584=DIRECTION('ref_axis',(0.866025403784439,0.499999999999999,0.));
#28585=DIRECTION('',(-0.5,-0.866025403784439,0.));
#28586=DIRECTION('center_axis',(0.,0.,1.));
#28587=DIRECTION('ref_axis',(0.,-1.,0.));
#28588=DIRECTION('',(-0.5,0.866025403784439,0.));
#28589=DIRECTION('center_axis',(0.,0.,1.));
#28590=DIRECTION('ref_axis',(-0.86602540378444,0.499999999999997,0.));
#28591=DIRECTION('',(1.,0.,0.));
#28592=DIRECTION('center_axis',(0.,0.,1.));
#28593=DIRECTION('ref_axis',(0.866025403784441,0.499999999999996,0.));
#28594=DIRECTION('center_axis',(0.,0.,1.));
#28595=DIRECTION('ref_axis',(1.,0.,0.));
#28596=DIRECTION('center_axis',(0.,0.,1.));
#28597=DIRECTION('ref_axis',(0.425897586725943,0.904771377542978,0.));
#28598=DIRECTION('',(0.,0.,-1.));
#28599=DIRECTION('center_axis',(0.,0.,1.));
#28600=DIRECTION('ref_axis',(0.425897586725943,0.904771377542978,0.));
#28601=DIRECTION('',(0.,0.,1.));
#28602=DIRECTION('center_axis',(0.,0.,-1.));
#28603=DIRECTION('ref_axis',(-0.866025403784439,0.499999999999999,0.));
#28604=DIRECTION('center_axis',(0.,0.,1.));
#28605=DIRECTION('ref_axis',(-0.866025403784439,0.499999999999999,0.));
#28606=DIRECTION('',(0.,0.,1.));
#28607=DIRECTION('',(0.,0.,-1.));
#28608=DIRECTION('center_axis',(0.,1.,0.));
#28609=DIRECTION('ref_axis',(1.,0.,0.));
#28610=DIRECTION('',(1.,0.,0.));
#28611=DIRECTION('',(0.,0.,1.));
#28612=DIRECTION('center_axis',(0.,0.,-1.));
#28613=DIRECTION('ref_axis',(0.425897586725943,-0.904771377542978,0.));
#28614=DIRECTION('center_axis',(0.,0.,1.));
#28615=DIRECTION('ref_axis',(0.425897586725943,-0.904771377542978,0.));
#28616=DIRECTION('',(0.,0.,1.));
#28617=DIRECTION('',(0.,0.,-1.));
#28618=DIRECTION('center_axis',(0.,0.,-1.));
#28619=DIRECTION('ref_axis',(-1.,0.,0.));
#28620=DIRECTION('',(-0.5,0.866025403784439,0.));
#28621=DIRECTION('center_axis',(0.,0.,1.));
#28622=DIRECTION('ref_axis',(1.,0.,0.));
#28623=DIRECTION('center_axis',(0.,0.,-1.));
#28624=DIRECTION('ref_axis',(-0.86602540378444,0.499999999999997,0.));
#28625=DIRECTION('center_axis',(0.,0.,1.));
#28626=DIRECTION('ref_axis',(-0.86602540378444,0.499999999999997,0.));
#28627=DIRECTION('',(0.,0.,1.));
#28628=DIRECTION('',(0.,0.,-1.));
#28629=DIRECTION('center_axis',(0.,1.,0.));
#28630=DIRECTION('ref_axis',(1.,0.,0.));
#28631=DIRECTION('',(1.,0.,0.));
#28632=DIRECTION('',(0.,0.,-1.));
#28633=DIRECTION('center_axis',(0.,0.,-1.));
#28634=DIRECTION('ref_axis',(0.,-1.,0.));
#28635=DIRECTION('center_axis',(0.,0.,1.));
#28636=DIRECTION('ref_axis',(0.,-1.,0.));
#28637=DIRECTION('',(0.,0.,1.));
#28638=DIRECTION('',(0.,0.,-1.));
#28639=DIRECTION('center_axis',(0.,0.,-1.));
#28640=DIRECTION('ref_axis',(-1.,0.,0.));
#28641=DIRECTION('',(-0.5,0.866025403784439,0.));
#28642=DIRECTION('',(-0.5,-0.866025403784439,0.));
#28643=DIRECTION('center_axis',(0.,0.,1.));
#28644=DIRECTION('ref_axis',(0.866025403784441,0.499999999999996,0.));
#28645=DIRECTION('center_axis',(0.866025403784439,-0.5,0.));
#28646=DIRECTION('ref_axis',(-0.5,-0.866025403784439,0.));
#28647=DIRECTION('',(0.,0.,1.));
#28648=DIRECTION('center_axis',(0.,0.,-1.));
#28649=DIRECTION('ref_axis',(0.866025403784441,0.499999999999996,0.));
#28650=DIRECTION('center_axis',(0.,0.,-1.));
#28651=DIRECTION('ref_axis',(-0.866025403784439,0.5,0.));
#28652=DIRECTION('center_axis',(0.,0.,1.));
#28653=DIRECTION('ref_axis',(-0.866025403784439,0.5,0.));
#28654=DIRECTION('',(0.,0.,1.));
#28655=DIRECTION('',(0.,0.,-1.));
#28656=DIRECTION('center_axis',(0.,1.,0.));
#28657=DIRECTION('ref_axis',(1.,0.,0.));
#28658=DIRECTION('',(1.,0.,0.));
#28659=DIRECTION('',(0.,0.,-1.));
#28660=DIRECTION('center_axis',(0.,0.,-1.));
#28661=DIRECTION('ref_axis',(0.,-1.,0.));
#28662=DIRECTION('center_axis',(0.,0.,1.));
#28663=DIRECTION('ref_axis',(0.,-1.,0.));
#28664=DIRECTION('',(0.,0.,1.));
#28665=DIRECTION('',(0.,0.,-1.));
#28666=DIRECTION('center_axis',(0.,0.,-1.));
#28667=DIRECTION('ref_axis',(-1.,0.,0.));
#28668=DIRECTION('',(-0.5,0.866025403784439,0.));
#28669=DIRECTION('',(-0.5,-0.866025403784439,0.));
#28670=DIRECTION('center_axis',(0.,0.,1.));
#28671=DIRECTION('ref_axis',(0.866025403784439,0.499999999999999,0.));
#28672=DIRECTION('center_axis',(0.866025403784439,-0.5,0.));
#28673=DIRECTION('ref_axis',(-0.5,-0.866025403784439,0.));
#28674=DIRECTION('',(0.,0.,1.));
#28675=DIRECTION('center_axis',(0.,0.,-1.));
#28676=DIRECTION('ref_axis',(0.866025403784439,0.499999999999999,0.));
#28677=DIRECTION('center_axis',(0.,0.,1.));
#28678=DIRECTION('ref_axis',(0.996503790932232,0.0835475592563325,0.));
#28679=DIRECTION('',(0.,0.,-1.));
#28680=DIRECTION('center_axis',(0.,0.,1.));
#28681=DIRECTION('ref_axis',(0.996503790932232,0.0835475592563325,0.));
#28682=DIRECTION('',(0.,0.,1.));
#28683=DIRECTION('center_axis',(0.,0.,-1.));
#28684=DIRECTION('ref_axis',(0.,1.,0.));
#28685=DIRECTION('center_axis',(0.,0.,1.));
#28686=DIRECTION('ref_axis',(0.,1.,0.));
#28687=DIRECTION('',(0.,0.,1.));
#28688=DIRECTION('',(0.,0.,-1.));
#28689=DIRECTION('center_axis',(0.866025403784439,0.5,0.));
#28690=DIRECTION('ref_axis',(0.5,-0.866025403784439,0.));
#28691=DIRECTION('',(0.5,-0.866025403784439,0.));
#28692=DIRECTION('',(0.,0.,-1.));
#28693=DIRECTION('center_axis',(0.,0.,-1.));
#28694=DIRECTION('ref_axis',(-0.866025403784439,-0.5,0.));
#28695=DIRECTION('center_axis',(0.,0.,1.));
#28696=DIRECTION('ref_axis',(-0.866025403784439,-0.5,0.));
#28697=DIRECTION('',(0.,0.,1.));
#28698=DIRECTION('',(0.,0.,-1.));
#28699=DIRECTION('center_axis',(0.,0.,-1.));
#28700=DIRECTION('ref_axis',(-1.,0.,0.));
#28701=DIRECTION('',(0.5,0.866025403784439,0.));
#28702=DIRECTION('',(-1.,0.,0.));
#28703=DIRECTION('center_axis',(0.,0.,1.));
#28704=DIRECTION('ref_axis',(0.866025403784438,-0.500000000000002,0.));
#28705=DIRECTION('center_axis',(0.,-1.,0.));
#28706=DIRECTION('ref_axis',(-1.,0.,0.));
#28707=DIRECTION('',(0.,0.,1.));
#28708=DIRECTION('center_axis',(0.,0.,-1.));
#28709=DIRECTION('ref_axis',(0.866025403784438,-0.500000000000002,0.));
#28710=DIRECTION('center_axis',(0.,0.,-1.));
#28711=DIRECTION('ref_axis',(-0.866025403784439,0.5,0.));
#28712=DIRECTION('center_axis',(0.,0.,1.));
#28713=DIRECTION('ref_axis',(-0.866025403784439,0.5,0.));
#28714=DIRECTION('',(0.,0.,1.));
#28715=DIRECTION('',(0.,0.,-1.));
#28716=DIRECTION('center_axis',(0.,1.,0.));
#28717=DIRECTION('ref_axis',(1.,0.,0.));
#28718=DIRECTION('',(1.,0.,0.));
#28719=DIRECTION('',(0.,0.,-1.));
#28720=DIRECTION('center_axis',(0.,0.,-1.));
#28721=DIRECTION('ref_axis',(6.93889390390722E-16,-1.,0.));
#28722=DIRECTION('center_axis',(0.,0.,1.));
#28723=DIRECTION('ref_axis',(6.93889390390722E-16,-1.,0.));
#28724=DIRECTION('',(0.,0.,1.));
#28725=DIRECTION('',(0.,0.,-1.));
#28726=DIRECTION('center_axis',(0.,0.,-1.));
#28727=DIRECTION('ref_axis',(-1.,0.,0.));
#28728=DIRECTION('',(-0.5,0.866025403784439,0.));
#28729=DIRECTION('',(-0.5,-0.866025403784439,0.));
#28730=DIRECTION('center_axis',(0.,0.,1.));
#28731=DIRECTION('ref_axis',(0.86602540378444,0.499999999999997,0.));
#28732=DIRECTION('center_axis',(0.866025403784439,-0.5,0.));
#28733=DIRECTION('ref_axis',(-0.5,-0.866025403784439,0.));
#28734=DIRECTION('',(0.,0.,1.));
#28735=DIRECTION('center_axis',(0.,0.,-1.));
#28736=DIRECTION('ref_axis',(0.86602540378444,0.499999999999997,0.));
#28737=DIRECTION('center_axis',(0.,0.,-1.));
#28738=DIRECTION('ref_axis',(0.86602540378444,0.499999999999997,0.));
#28739=DIRECTION('center_axis',(0.,0.,1.));
#28740=DIRECTION('ref_axis',(0.86602540378444,0.499999999999997,0.));
#28741=DIRECTION('',(0.,0.,1.));
#28742=DIRECTION('',(0.,0.,-1.));
#28743=DIRECTION('center_axis',(0.866025403784439,-0.5,0.));
#28744=DIRECTION('ref_axis',(-0.5,-0.866025403784439,0.));
#28745=DIRECTION('',(-0.5,-0.866025403784439,0.));
#28746=DIRECTION('',(0.,0.,1.));
#28747=DIRECTION('center_axis',(0.,0.,-1.));
#28748=DIRECTION('ref_axis',(-0.86602540378444,-0.499999999999997,0.));
#28749=DIRECTION('center_axis',(0.,0.,1.));
#28750=DIRECTION('ref_axis',(-0.86602540378444,-0.499999999999997,0.));
#28751=DIRECTION('',(0.,0.,1.));
#28752=DIRECTION('',(0.,0.,-1.));
#28753=DIRECTION('center_axis',(0.,0.,-1.));
#28754=DIRECTION('ref_axis',(-1.,0.,0.));
#28755=DIRECTION('',(-1.,0.,0.));
#28756=DIRECTION('center_axis',(0.,0.,1.));
#28757=DIRECTION('ref_axis',(0.996503790932232,-0.0835475592563362,0.));
#28758=DIRECTION('center_axis',(0.,0.,1.));
#28759=DIRECTION('ref_axis',(1.,0.,0.));
#28760=DIRECTION('',(0.5,0.866025403784439,0.));
#28761=DIRECTION('center_axis',(0.,-1.,0.));
#28762=DIRECTION('ref_axis',(-1.,0.,0.));
#28763=DIRECTION('',(0.,0.,1.));
#28764=DIRECTION('center_axis',(0.,0.,-1.));
#28765=DIRECTION('ref_axis',(0.996503790932232,-0.0835475592563362,0.));
#28766=DIRECTION('',(0.,0.,-1.));
#28767=DIRECTION('center_axis',(0.,0.,-1.));
#28768=DIRECTION('ref_axis',(-6.93889390390722E-16,1.,0.));
#28769=DIRECTION('center_axis',(0.,0.,1.));
#28770=DIRECTION('ref_axis',(-6.93889390390722E-16,1.,0.));
#28771=DIRECTION('',(0.,0.,1.));
#28772=DIRECTION('',(0.,0.,-1.));
#28773=DIRECTION('center_axis',(0.866025403784439,0.5,0.));
#28774=DIRECTION('ref_axis',(0.5,-0.866025403784439,0.));
#28775=DIRECTION('',(0.5,-0.866025403784439,0.));
#28776=DIRECTION('',(0.,0.,-1.));
#28777=DIRECTION('center_axis',(0.,0.,-1.));
#28778=DIRECTION('ref_axis',(-0.86602540378444,-0.499999999999997,0.));
#28779=DIRECTION('center_axis',(0.,0.,1.));
#28780=DIRECTION('ref_axis',(-0.86602540378444,-0.499999999999997,0.));
#28781=DIRECTION('',(0.,0.,1.));
#28782=DIRECTION('',(0.,0.,-1.));
#28783=DIRECTION('center_axis',(0.,0.,-1.));
#28784=DIRECTION('ref_axis',(-1.,0.,0.));
#28785=DIRECTION('',(0.5,0.866025403784439,0.));
#28786=DIRECTION('',(-1.,0.,0.));
#28787=DIRECTION('center_axis',(0.,0.,1.));
#28788=DIRECTION('ref_axis',(0.866025403784439,-0.5,0.));
#28789=DIRECTION('center_axis',(0.,-1.,0.));
#28790=DIRECTION('ref_axis',(-1.,0.,0.));
#28791=DIRECTION('',(0.,0.,1.));
#28792=DIRECTION('center_axis',(0.,0.,-1.));
#28793=DIRECTION('ref_axis',(0.866025403784439,-0.5,0.));
#28794=DIRECTION('center_axis',(0.,0.,-1.));
#28795=DIRECTION('ref_axis',(-0.866025403784438,0.500000000000002,0.));
#28796=DIRECTION('center_axis',(0.,0.,1.));
#28797=DIRECTION('ref_axis',(-0.866025403784438,0.500000000000002,0.));
#28798=DIRECTION('',(0.,0.,1.));
#28799=DIRECTION('',(0.,0.,-1.));
#28800=DIRECTION('center_axis',(0.,1.,0.));
#28801=DIRECTION('ref_axis',(1.,0.,0.));
#28802=DIRECTION('',(1.,0.,0.));
#28803=DIRECTION('',(0.,0.,-1.));
#28804=DIRECTION('center_axis',(0.,0.,-1.));
#28805=DIRECTION('ref_axis',(0.,-1.,0.));
#28806=DIRECTION('center_axis',(0.,0.,1.));
#28807=DIRECTION('ref_axis',(0.,-1.,0.));
#28808=DIRECTION('',(0.,0.,1.));
#28809=DIRECTION('',(0.,0.,-1.));
#28810=DIRECTION('center_axis',(0.,0.,-1.));
#28811=DIRECTION('ref_axis',(-1.,0.,0.));
#28812=DIRECTION('',(-0.5,0.866025403784439,0.));
#28813=DIRECTION('',(-0.5,-0.866025403784439,0.));
#28814=DIRECTION('center_axis',(0.,0.,1.));
#28815=DIRECTION('ref_axis',(0.866025403784439,0.5,0.));
#28816=DIRECTION('center_axis',(0.866025403784439,-0.5,0.));
#28817=DIRECTION('ref_axis',(-0.5,-0.866025403784439,0.));
#28818=DIRECTION('',(0.,0.,1.));
#28819=DIRECTION('center_axis',(0.,0.,-1.));
#28820=DIRECTION('ref_axis',(0.866025403784439,0.5,0.));
#28821=DIRECTION('center_axis',(0.,0.,1.));
#28822=DIRECTION('ref_axis',(-0.996503790932232,-0.0835475592563325,0.));
#28823=DIRECTION('',(0.,0.,-1.));
#28824=DIRECTION('center_axis',(0.,0.,1.));
#28825=DIRECTION('ref_axis',(-0.996503790932232,-0.0835475592563325,0.));
#28826=DIRECTION('',(0.,0.,1.));
#28827=DIRECTION('center_axis',(0.,0.,-1.));
#28828=DIRECTION('ref_axis',(-1.,0.,0.));
#28829=DIRECTION('',(-1.,0.,0.));
#28830=DIRECTION('center_axis',(0.,0.,1.));
#28831=DIRECTION('ref_axis',(0.866025403784437,-0.500000000000003,0.));
#28832=DIRECTION('',(0.5,-0.866025403784439,0.));
#28833=DIRECTION('center_axis',(0.,0.,1.));
#28834=DIRECTION('ref_axis',(1.,0.,0.));
#28835=DIRECTION('center_axis',(0.,-1.,0.));
#28836=DIRECTION('ref_axis',(-1.,0.,0.));
#28837=DIRECTION('',(0.,0.,1.));
#28838=DIRECTION('center_axis',(0.,0.,-1.));
#28839=DIRECTION('ref_axis',(0.866025403784437,-0.500000000000003,0.));
#28840=DIRECTION('',(0.,0.,-1.));
#28841=DIRECTION('center_axis',(0.866025403784439,0.5,0.));
#28842=DIRECTION('ref_axis',(0.5,-0.866025403784439,0.));
#28843=DIRECTION('',(0.,0.,-1.));
#28844=DIRECTION('center_axis',(0.,0.,-1.));
#28845=DIRECTION('ref_axis',(0.,1.,0.));
#28846=DIRECTION('center_axis',(0.,0.,1.));
#28847=DIRECTION('ref_axis',(0.,1.,0.));
#28848=DIRECTION('',(0.,0.,1.));
#28849=DIRECTION('',(0.,0.,-1.));
#28850=DIRECTION('center_axis',(0.866025403784439,0.5,0.));
#28851=DIRECTION('ref_axis',(0.5,-0.866025403784439,0.));
#28852=DIRECTION('',(0.5,-0.866025403784439,0.));
#28853=DIRECTION('',(0.,0.,-1.));
#28854=DIRECTION('center_axis',(0.,0.,-1.));
#28855=DIRECTION('ref_axis',(-0.866025403784439,-0.499999999999999,0.));
#28856=DIRECTION('center_axis',(0.,0.,1.));
#28857=DIRECTION('ref_axis',(-0.866025403784439,-0.499999999999999,0.));
#28858=DIRECTION('',(0.,0.,1.));
#28859=DIRECTION('',(0.,0.,-1.));
#28860=DIRECTION('center_axis',(0.,0.,-1.));
#28861=DIRECTION('ref_axis',(-1.,0.,0.));
#28862=DIRECTION('',(0.5,0.866025403784439,0.));
#28863=DIRECTION('',(-1.,0.,0.));
#28864=DIRECTION('center_axis',(0.,0.,1.));
#28865=DIRECTION('ref_axis',(0.866025403784439,-0.5,0.));
#28866=DIRECTION('center_axis',(0.,-1.,0.));
#28867=DIRECTION('ref_axis',(-1.,0.,0.));
#28868=DIRECTION('',(0.,0.,1.));
#28869=DIRECTION('center_axis',(0.,0.,-1.));
#28870=DIRECTION('ref_axis',(0.866025403784439,-0.5,0.));
#28871=DIRECTION('center_axis',(0.,0.,-1.));
#28872=DIRECTION('ref_axis',(0.,1.,0.));
#28873=DIRECTION('center_axis',(0.,0.,1.));
#28874=DIRECTION('ref_axis',(0.,1.,0.));
#28875=DIRECTION('',(0.,0.,1.));
#28876=DIRECTION('',(0.,0.,-1.));
#28877=DIRECTION('center_axis',(0.866025403784439,0.5,0.));
#28878=DIRECTION('ref_axis',(0.5,-0.866025403784439,0.));
#28879=DIRECTION('',(0.5,-0.866025403784439,0.));
#28880=DIRECTION('',(0.,0.,-1.));
#28881=DIRECTION('center_axis',(0.,0.,-1.));
#28882=DIRECTION('ref_axis',(-0.866025403784441,-0.499999999999996,0.));
#28883=DIRECTION('center_axis',(0.,0.,1.));
#28884=DIRECTION('ref_axis',(-0.866025403784441,-0.499999999999996,0.));
#28885=DIRECTION('',(0.,0.,1.));
#28886=DIRECTION('',(0.,0.,-1.));
#28887=DIRECTION('center_axis',(0.,0.,-1.));
#28888=DIRECTION('ref_axis',(-1.,0.,0.));
#28889=DIRECTION('',(0.5,0.866025403784439,0.));
#28890=DIRECTION('',(-1.,0.,0.));
#28891=DIRECTION('center_axis',(0.,0.,1.));
#28892=DIRECTION('ref_axis',(0.86602540378444,-0.499999999999997,0.));
#28893=DIRECTION('center_axis',(0.,-1.,0.));
#28894=DIRECTION('ref_axis',(-1.,0.,0.));
#28895=DIRECTION('',(0.,0.,1.));
#28896=DIRECTION('center_axis',(0.,0.,-1.));
#28897=DIRECTION('ref_axis',(0.86602540378444,-0.499999999999997,0.));
#28898=DIRECTION('center_axis',(0.,0.,-1.));
#28899=DIRECTION('ref_axis',(0.866025403784439,-0.499999999999999,0.));
#28900=DIRECTION('center_axis',(0.,0.,1.));
#28901=DIRECTION('ref_axis',(0.866025403784439,-0.499999999999999,0.));
#28902=DIRECTION('',(0.,0.,1.));
#28903=DIRECTION('',(0.,0.,-1.));
#28904=DIRECTION('center_axis',(0.,-1.,0.));
#28905=DIRECTION('ref_axis',(-1.,0.,0.));
#28906=DIRECTION('',(-1.,0.,0.));
#28907=DIRECTION('',(0.,0.,1.));
#28908=DIRECTION('center_axis',(0.,0.,-1.));
#28909=DIRECTION('ref_axis',(0.,-1.,0.));
#28910=DIRECTION('center_axis',(0.,0.,1.));
#28911=DIRECTION('ref_axis',(0.,-1.,0.));
#28912=DIRECTION('',(0.,0.,1.));
#28913=DIRECTION('',(0.,0.,-1.));
#28914=DIRECTION('center_axis',(0.,0.,-1.));
#28915=DIRECTION('ref_axis',(-1.,0.,0.));
#28916=DIRECTION('',(-0.5,-0.866025403784439,0.));
#28917=DIRECTION('center_axis',(0.,0.,1.));
#28918=DIRECTION('ref_axis',(0.570606204206288,0.821223818286642,0.));
#28919=DIRECTION('center_axis',(0.,0.,1.));
#28920=DIRECTION('ref_axis',(1.,0.,0.));
#28921=DIRECTION('',(-0.5,0.866025403784439,0.));
#28922=DIRECTION('center_axis',(0.866025403784439,-0.5,0.));
#28923=DIRECTION('ref_axis',(-0.5,-0.866025403784439,0.));
#28924=DIRECTION('',(0.,0.,1.));
#28925=DIRECTION('center_axis',(0.,0.,-1.));
#28926=DIRECTION('ref_axis',(0.570606204206288,0.821223818286642,0.));
#28927=DIRECTION('',(0.,0.,-1.));
#28928=DIRECTION('center_axis',(0.,0.,-1.));
#28929=DIRECTION('ref_axis',(-0.86602540378444,0.499999999999997,0.));
#28930=DIRECTION('center_axis',(0.,0.,1.));
#28931=DIRECTION('ref_axis',(-0.86602540378444,0.499999999999997,0.));
#28932=DIRECTION('',(0.,0.,1.));
#28933=DIRECTION('',(0.,0.,-1.));
#28934=DIRECTION('center_axis',(0.,1.,0.));
#28935=DIRECTION('ref_axis',(1.,0.,0.));
#28936=DIRECTION('',(1.,0.,0.));
#28937=DIRECTION('',(0.,0.,-1.));
#28938=DIRECTION('center_axis',(0.,0.,-1.));
#28939=DIRECTION('ref_axis',(0.,-1.,0.));
#28940=DIRECTION('center_axis',(0.,0.,1.));
#28941=DIRECTION('ref_axis',(0.,-1.,0.));
#28942=DIRECTION('',(0.,0.,1.));
#28943=DIRECTION('',(0.,0.,-1.));
#28944=DIRECTION('center_axis',(0.,0.,-1.));
#28945=DIRECTION('ref_axis',(-1.,0.,0.));
#28946=DIRECTION('',(-0.5,0.866025403784439,0.));
#28947=DIRECTION('',(-0.5,-0.866025403784439,0.));
#28948=DIRECTION('center_axis',(0.,0.,1.));
#28949=DIRECTION('ref_axis',(0.866025403784441,0.499999999999996,0.));
#28950=DIRECTION('center_axis',(0.866025403784439,-0.5,0.));
#28951=DIRECTION('ref_axis',(-0.5,-0.866025403784439,0.));
#28952=DIRECTION('',(0.,0.,1.));
#28953=DIRECTION('center_axis',(0.,0.,-1.));
#28954=DIRECTION('ref_axis',(0.866025403784441,0.499999999999996,0.));
#28955=DIRECTION('center_axis',(0.,0.,-1.));
#28956=DIRECTION('ref_axis',(-0.866025403784439,0.499999999999999,0.));
#28957=DIRECTION('center_axis',(0.,0.,1.));
#28958=DIRECTION('ref_axis',(-0.866025403784439,0.499999999999999,0.));
#28959=DIRECTION('',(0.,0.,1.));
#28960=DIRECTION('',(0.,0.,-1.));
#28961=DIRECTION('center_axis',(0.,1.,0.));
#28962=DIRECTION('ref_axis',(1.,0.,0.));
#28963=DIRECTION('',(1.,0.,0.));
#28964=DIRECTION('',(0.,0.,-1.));
#28965=DIRECTION('center_axis',(0.,0.,-1.));
#28966=DIRECTION('ref_axis',(-3.70074341541719E-15,-1.,0.));
#28967=DIRECTION('center_axis',(0.,0.,1.));
#28968=DIRECTION('ref_axis',(-3.70074341541719E-15,-1.,0.));
#28969=DIRECTION('',(0.,0.,1.));
#28970=DIRECTION('',(0.,0.,-1.));
#28971=DIRECTION('center_axis',(0.,0.,-1.));
#28972=DIRECTION('ref_axis',(-1.,0.,0.));
#28973=DIRECTION('',(-0.5,0.866025403784439,0.));
#28974=DIRECTION('',(-0.5,-0.866025403784439,0.));
#28975=DIRECTION('center_axis',(0.,0.,1.));
#28976=DIRECTION('ref_axis',(0.86602540378444,0.499999999999997,0.));
#28977=DIRECTION('center_axis',(0.866025403784439,-0.5,0.));
#28978=DIRECTION('ref_axis',(-0.5,-0.866025403784439,0.));
#28979=DIRECTION('',(0.,0.,1.));
#28980=DIRECTION('center_axis',(0.,0.,-1.));
#28981=DIRECTION('ref_axis',(0.86602540378444,0.499999999999997,0.));
#28982=DIRECTION('center_axis',(0.,0.,-1.));
#28983=DIRECTION('ref_axis',(-0.86602540378444,0.499999999999997,0.));
#28984=DIRECTION('center_axis',(0.,0.,1.));
#28985=DIRECTION('ref_axis',(-0.86602540378444,0.499999999999997,0.));
#28986=DIRECTION('',(0.,0.,1.));
#28987=DIRECTION('',(0.,0.,-1.));
#28988=DIRECTION('center_axis',(0.,1.,0.));
#28989=DIRECTION('ref_axis',(1.,0.,0.));
#28990=DIRECTION('',(1.,0.,0.));
#28991=DIRECTION('',(0.,0.,-1.));
#28992=DIRECTION('center_axis',(0.,0.,-1.));
#28993=DIRECTION('ref_axis',(1.85037170770859E-15,-1.,0.));
#28994=DIRECTION('center_axis',(0.,0.,1.));
#28995=DIRECTION('ref_axis',(1.85037170770859E-15,-1.,0.));
#28996=DIRECTION('',(0.,0.,1.));
#28997=DIRECTION('',(0.,0.,-1.));
#28998=DIRECTION('center_axis',(0.,0.,-1.));
#28999=DIRECTION('ref_axis',(-1.,0.,0.));
#29000=DIRECTION('',(-0.5,0.866025403784439,0.));
#29001=DIRECTION('',(-0.5,-0.866025403784439,0.));
#29002=DIRECTION('center_axis',(0.,0.,1.));
#29003=DIRECTION('ref_axis',(0.86602540378444,0.499999999999998,0.));
#29004=DIRECTION('center_axis',(0.866025403784439,-0.5,0.));
#29005=DIRECTION('ref_axis',(-0.5,-0.866025403784439,0.));
#29006=DIRECTION('',(0.,0.,1.));
#29007=DIRECTION('center_axis',(0.,0.,-1.));
#29008=DIRECTION('ref_axis',(0.86602540378444,0.499999999999998,0.));
#29009=DIRECTION('center_axis',(0.,0.,1.));
#29010=DIRECTION('ref_axis',(0.570606204206288,-0.821223818286642,0.));
#29011=DIRECTION('',(0.,0.,-1.));
#29012=DIRECTION('center_axis',(0.,0.,1.));
#29013=DIRECTION('ref_axis',(0.570606204206288,-0.821223818286642,0.));
#29014=DIRECTION('',(0.,0.,1.));
#29015=DIRECTION('center_axis',(0.,0.,-1.));
#29016=DIRECTION('ref_axis',(0.,1.,0.));
#29017=DIRECTION('center_axis',(0.,0.,1.));
#29018=DIRECTION('ref_axis',(0.,1.,0.));
#29019=DIRECTION('',(0.,0.,1.));
#29020=DIRECTION('',(0.,0.,-1.));
#29021=DIRECTION('center_axis',(0.866025403784439,0.5,0.));
#29022=DIRECTION('ref_axis',(0.5,-0.866025403784439,0.));
#29023=DIRECTION('',(0.5,-0.866025403784439,0.));
#29024=DIRECTION('',(0.,0.,-1.));
#29025=DIRECTION('center_axis',(0.,0.,-1.));
#29026=DIRECTION('ref_axis',(-0.866025403784439,-0.499999999999999,0.));
#29027=DIRECTION('center_axis',(0.,0.,1.));
#29028=DIRECTION('ref_axis',(-0.866025403784439,-0.499999999999999,0.));
#29029=DIRECTION('',(0.,0.,1.));
#29030=DIRECTION('',(0.,0.,-1.));
#29031=DIRECTION('center_axis',(0.,0.,-1.));
#29032=DIRECTION('ref_axis',(-1.,0.,0.));
#29033=DIRECTION('',(0.5,0.866025403784439,0.));
#29034=DIRECTION('',(-1.,0.,0.));
#29035=DIRECTION('center_axis',(0.,0.,1.));
#29036=DIRECTION('ref_axis',(0.86602540378444,-0.499999999999997,0.));
#29037=DIRECTION('center_axis',(0.,-1.,0.));
#29038=DIRECTION('ref_axis',(-1.,0.,0.));
#29039=DIRECTION('',(0.,0.,1.));
#29040=DIRECTION('center_axis',(0.,0.,-1.));
#29041=DIRECTION('ref_axis',(0.86602540378444,-0.499999999999997,0.));
#29042=DIRECTION('center_axis',(0.,0.,-1.));
#29043=DIRECTION('ref_axis',(-0.86602540378444,0.499999999999997,0.));
#29044=DIRECTION('center_axis',(0.,0.,1.));
#29045=DIRECTION('ref_axis',(-0.86602540378444,0.499999999999997,0.));
#29046=DIRECTION('',(0.,0.,1.));
#29047=DIRECTION('',(0.,0.,-1.));
#29048=DIRECTION('center_axis',(0.,1.,0.));
#29049=DIRECTION('ref_axis',(1.,0.,0.));
#29050=DIRECTION('',(1.,0.,0.));
#29051=DIRECTION('',(0.,0.,-1.));
#29052=DIRECTION('center_axis',(0.,0.,-1.));
#29053=DIRECTION('ref_axis',(0.,-1.,0.));
#29054=DIRECTION('center_axis',(0.,0.,1.));
#29055=DIRECTION('ref_axis',(0.,-1.,0.));
#29056=DIRECTION('',(0.,0.,1.));
#29057=DIRECTION('',(0.,0.,-1.));
#29058=DIRECTION('center_axis',(0.,0.,-1.));
#29059=DIRECTION('ref_axis',(-1.,0.,0.));
#29060=DIRECTION('',(-0.5,0.866025403784439,0.));
#29061=DIRECTION('',(-0.5,-0.866025403784439,0.));
#29062=DIRECTION('center_axis',(0.,0.,1.));
#29063=DIRECTION('ref_axis',(0.86602540378444,0.499999999999997,0.));
#29064=DIRECTION('center_axis',(0.866025403784439,-0.5,0.));
#29065=DIRECTION('ref_axis',(-0.5,-0.866025403784439,0.));
#29066=DIRECTION('',(0.,0.,1.));
#29067=DIRECTION('center_axis',(0.,0.,-1.));
#29068=DIRECTION('ref_axis',(0.86602540378444,0.499999999999997,0.));
#29069=DIRECTION('center_axis',(0.,0.,1.));
#29070=DIRECTION('ref_axis',(-0.425897586725943,-0.904771377542978,0.));
#29071=DIRECTION('',(0.,0.,-1.));
#29072=DIRECTION('center_axis',(0.,0.,1.));
#29073=DIRECTION('ref_axis',(-0.425897586725943,-0.904771377542978,0.));
#29074=DIRECTION('',(0.,0.,1.));
#29075=DIRECTION('center_axis',(0.,0.,-1.));
#29076=DIRECTION('ref_axis',(-1.,0.,0.));
#29077=DIRECTION('',(-0.5,-0.866025403784439,0.));
#29078=DIRECTION('center_axis',(0.,0.,1.));
#29079=DIRECTION('ref_axis',(0.866025403784438,0.500000000000002,0.));
#29080=DIRECTION('',(1.,0.,0.));
#29081=DIRECTION('center_axis',(0.,0.,1.));
#29082=DIRECTION('ref_axis',(1.,0.,0.));
#29083=DIRECTION('center_axis',(0.866025403784439,-0.5,0.));
#29084=DIRECTION('ref_axis',(-0.5,-0.866025403784439,0.));
#29085=DIRECTION('',(0.,0.,1.));
#29086=DIRECTION('center_axis',(0.,0.,-1.));
#29087=DIRECTION('ref_axis',(0.866025403784438,0.500000000000002,0.));
#29088=DIRECTION('',(0.,0.,-1.));
#29089=DIRECTION('center_axis',(0.,1.,0.));
#29090=DIRECTION('ref_axis',(1.,0.,0.));
#29091=DIRECTION('',(0.,0.,-1.));
#29092=DIRECTION('center_axis',(0.,0.,-1.));
#29093=DIRECTION('ref_axis',(0.,1.,0.));
#29094=DIRECTION('center_axis',(0.,0.,1.));
#29095=DIRECTION('ref_axis',(0.,1.,0.));
#29096=DIRECTION('',(0.,0.,1.));
#29097=DIRECTION('',(0.,0.,-1.));
#29098=DIRECTION('center_axis',(0.866025403784439,0.5,0.));
#29099=DIRECTION('ref_axis',(0.5,-0.866025403784439,0.));
#29100=DIRECTION('',(0.5,-0.866025403784439,0.));
#29101=DIRECTION('',(0.,0.,-1.));
#29102=DIRECTION('center_axis',(0.,0.,-1.));
#29103=DIRECTION('ref_axis',(-0.86602540378444,-0.499999999999997,0.));
#29104=DIRECTION('center_axis',(0.,0.,1.));
#29105=DIRECTION('ref_axis',(-0.86602540378444,-0.499999999999997,0.));
#29106=DIRECTION('',(0.,0.,1.));
#29107=DIRECTION('',(0.,0.,-1.));
#29108=DIRECTION('center_axis',(0.,0.,-1.));
#29109=DIRECTION('ref_axis',(-1.,0.,0.));
#29110=DIRECTION('',(0.5,0.866025403784439,0.));
#29111=DIRECTION('',(-1.,0.,0.));
#29112=DIRECTION('center_axis',(0.,0.,1.));
#29113=DIRECTION('ref_axis',(0.86602540378444,-0.499999999999997,0.));
#29114=DIRECTION('center_axis',(0.,-1.,0.));
#29115=DIRECTION('ref_axis',(-1.,0.,0.));
#29116=DIRECTION('',(0.,0.,1.));
#29117=DIRECTION('center_axis',(0.,0.,-1.));
#29118=DIRECTION('ref_axis',(0.86602540378444,-0.499999999999997,0.));
#29119=DIRECTION('center_axis',(0.,0.,-1.));
#29120=DIRECTION('ref_axis',(-0.86602540378444,0.499999999999997,0.));
#29121=DIRECTION('center_axis',(0.,0.,1.));
#29122=DIRECTION('ref_axis',(-0.86602540378444,0.499999999999997,0.));
#29123=DIRECTION('',(0.,0.,1.));
#29124=DIRECTION('',(0.,0.,-1.));
#29125=DIRECTION('center_axis',(0.,1.,0.));
#29126=DIRECTION('ref_axis',(1.,0.,0.));
#29127=DIRECTION('',(1.,0.,0.));
#29128=DIRECTION('',(0.,0.,-1.));
#29129=DIRECTION('center_axis',(0.,0.,-1.));
#29130=DIRECTION('ref_axis',(0.,-1.,0.));
#29131=DIRECTION('center_axis',(0.,0.,1.));
#29132=DIRECTION('ref_axis',(0.,-1.,0.));
#29133=DIRECTION('',(0.,0.,1.));
#29134=DIRECTION('',(0.,0.,-1.));
#29135=DIRECTION('center_axis',(0.,0.,-1.));
#29136=DIRECTION('ref_axis',(-1.,0.,0.));
#29137=DIRECTION('',(-0.5,0.866025403784439,0.));
#29138=DIRECTION('',(-0.5,-0.866025403784439,0.));
#29139=DIRECTION('center_axis',(0.,0.,1.));
#29140=DIRECTION('ref_axis',(0.866025403784439,0.499999999999999,0.));
#29141=DIRECTION('center_axis',(0.866025403784439,-0.5,0.));
#29142=DIRECTION('ref_axis',(-0.5,-0.866025403784439,0.));
#29143=DIRECTION('',(0.,0.,1.));
#29144=DIRECTION('center_axis',(0.,0.,-1.));
#29145=DIRECTION('ref_axis',(0.866025403784439,0.499999999999999,0.));
#29146=DIRECTION('center_axis',(0.,0.,1.));
#29147=DIRECTION('ref_axis',(-0.570606204206288,0.821223818286642,0.));
#29148=DIRECTION('',(0.,0.,-1.));
#29149=DIRECTION('center_axis',(0.,0.,1.));
#29150=DIRECTION('ref_axis',(-0.570606204206288,0.821223818286642,0.));
#29151=DIRECTION('',(0.,0.,1.));
#29152=DIRECTION('center_axis',(0.,0.,-1.));
#29153=DIRECTION('ref_axis',(0.,-1.,0.));
#29154=DIRECTION('center_axis',(0.,0.,1.));
#29155=DIRECTION('ref_axis',(0.,-1.,0.));
#29156=DIRECTION('',(0.,0.,1.));
#29157=DIRECTION('',(0.,0.,-1.));
#29158=DIRECTION('center_axis',(0.,0.,-1.));
#29159=DIRECTION('ref_axis',(-1.,0.,0.));
#29160=DIRECTION('',(-0.5,0.866025403784439,0.));
#29161=DIRECTION('',(-0.5,-0.866025403784439,0.));
#29162=DIRECTION('center_axis',(0.,0.,1.));
#29163=DIRECTION('ref_axis',(1.,0.,0.));
#29164=DIRECTION('center_axis',(0.866025403784439,-0.5,0.));
#29165=DIRECTION('ref_axis',(-0.5,-0.866025403784439,0.));
#29166=DIRECTION('',(0.,0.,-1.));
#29167=DIRECTION('center_axis',(0.,0.,-1.));
#29168=DIRECTION('ref_axis',(-1.85037170770859E-15,1.,0.));
#29169=DIRECTION('center_axis',(0.,0.,1.));
#29170=DIRECTION('ref_axis',(-1.85037170770859E-15,1.,0.));
#29171=DIRECTION('',(0.,0.,1.));
#29172=DIRECTION('',(0.,0.,-1.));
#29173=DIRECTION('center_axis',(0.866025403784439,0.5,0.));
#29174=DIRECTION('ref_axis',(0.5,-0.866025403784439,0.));
#29175=DIRECTION('',(0.5,-0.866025403784439,0.));
#29176=DIRECTION('',(0.,0.,-1.));
#29177=DIRECTION('center_axis',(0.,0.,-1.));
#29178=DIRECTION('ref_axis',(-0.86602540378444,-0.499999999999998,0.));
#29179=DIRECTION('center_axis',(0.,0.,1.));
#29180=DIRECTION('ref_axis',(-0.86602540378444,-0.499999999999998,0.));
#29181=DIRECTION('',(0.,0.,1.));
#29182=DIRECTION('',(0.,0.,-1.));
#29183=DIRECTION('center_axis',(0.,0.,-1.));
#29184=DIRECTION('ref_axis',(-1.,0.,0.));
#29185=DIRECTION('',(0.5,0.866025403784439,0.));
#29186=DIRECTION('',(-1.,0.,0.));
#29187=DIRECTION('center_axis',(0.,0.,1.));
#29188=DIRECTION('ref_axis',(0.86602540378444,-0.499999999999997,0.));
#29189=DIRECTION('center_axis',(0.,-1.,0.));
#29190=DIRECTION('ref_axis',(-1.,0.,0.));
#29191=DIRECTION('',(0.,0.,1.));
#29192=DIRECTION('center_axis',(0.,0.,-1.));
#29193=DIRECTION('ref_axis',(0.86602540378444,-0.499999999999997,0.));
#29194=DIRECTION('center_axis',(0.,0.,-1.));
#29195=DIRECTION('ref_axis',(3.70074341541719E-15,1.,0.));
#29196=DIRECTION('center_axis',(0.,0.,1.));
#29197=DIRECTION('ref_axis',(3.70074341541719E-15,1.,0.));
#29198=DIRECTION('',(0.,0.,1.));
#29199=DIRECTION('',(0.,0.,-1.));
#29200=DIRECTION('center_axis',(0.866025403784439,0.5,0.));
#29201=DIRECTION('ref_axis',(0.5,-0.866025403784439,0.));
#29202=DIRECTION('',(0.5,-0.866025403784439,0.));
#29203=DIRECTION('',(0.,0.,-1.));
#29204=DIRECTION('center_axis',(0.,0.,-1.));
#29205=DIRECTION('ref_axis',(-0.86602540378444,-0.499999999999997,0.));
#29206=DIRECTION('center_axis',(0.,0.,1.));
#29207=DIRECTION('ref_axis',(-0.86602540378444,-0.499999999999997,0.));
#29208=DIRECTION('',(0.,0.,1.));
#29209=DIRECTION('',(0.,0.,-1.));
#29210=DIRECTION('center_axis',(0.,0.,-1.));
#29211=DIRECTION('ref_axis',(-1.,0.,0.));
#29212=DIRECTION('',(0.5,0.866025403784439,0.));
#29213=DIRECTION('',(-1.,0.,0.));
#29214=DIRECTION('center_axis',(0.,0.,1.));
#29215=DIRECTION('ref_axis',(0.866025403784439,-0.499999999999999,0.));
#29216=DIRECTION('center_axis',(0.,-1.,0.));
#29217=DIRECTION('ref_axis',(-1.,0.,0.));
#29218=DIRECTION('',(0.,0.,1.));
#29219=DIRECTION('center_axis',(0.,0.,-1.));
#29220=DIRECTION('ref_axis',(0.866025403784439,-0.499999999999999,0.));
#29221=DIRECTION('center_axis',(0.,0.,-1.));
#29222=DIRECTION('ref_axis',(0.,1.,0.));
#29223=DIRECTION('center_axis',(0.,0.,1.));
#29224=DIRECTION('ref_axis',(0.,1.,0.));
#29225=DIRECTION('',(0.,0.,1.));
#29226=DIRECTION('',(0.,0.,-1.));
#29227=DIRECTION('center_axis',(0.866025403784439,0.5,0.));
#29228=DIRECTION('ref_axis',(0.5,-0.866025403784439,0.));
#29229=DIRECTION('',(0.5,-0.866025403784439,0.));
#29230=DIRECTION('',(0.,0.,-1.));
#29231=DIRECTION('center_axis',(0.,0.,-1.));
#29232=DIRECTION('ref_axis',(-0.866025403784441,-0.499999999999996,0.));
#29233=DIRECTION('center_axis',(0.,0.,1.));
#29234=DIRECTION('ref_axis',(-0.866025403784441,-0.499999999999996,0.));
#29235=DIRECTION('',(0.,0.,1.));
#29236=DIRECTION('',(0.,0.,-1.));
#29237=DIRECTION('center_axis',(0.,0.,-1.));
#29238=DIRECTION('ref_axis',(-1.,0.,0.));
#29239=DIRECTION('',(0.5,0.866025403784439,0.));
#29240=DIRECTION('',(-1.,0.,0.));
#29241=DIRECTION('center_axis',(0.,0.,1.));
#29242=DIRECTION('ref_axis',(0.86602540378444,-0.499999999999997,0.));
#29243=DIRECTION('center_axis',(0.,-1.,0.));
#29244=DIRECTION('ref_axis',(-1.,0.,0.));
#29245=DIRECTION('',(0.,0.,1.));
#29246=DIRECTION('center_axis',(0.,0.,-1.));
#29247=DIRECTION('ref_axis',(0.86602540378444,-0.499999999999997,0.));
#29248=DIRECTION('center_axis',(0.,0.,-1.));
#29249=DIRECTION('ref_axis',(-0.866025403784438,-0.500000000000002,0.));
#29250=DIRECTION('center_axis',(0.,0.,1.));
#29251=DIRECTION('ref_axis',(-0.866025403784438,-0.500000000000002,0.));
#29252=DIRECTION('',(0.,0.,1.));
#29253=DIRECTION('',(0.,0.,-1.));
#29254=DIRECTION('center_axis',(0.,0.,-1.));
#29255=DIRECTION('ref_axis',(-1.,0.,0.));
#29256=DIRECTION('',(0.5,0.866025403784439,0.));
#29257=DIRECTION('',(-1.,0.,0.));
#29258=DIRECTION('center_axis',(0.,0.,1.));
#29259=DIRECTION('ref_axis',(1.,0.,0.));
#29260=DIRECTION('center_axis',(0.,-1.,0.));
#29261=DIRECTION('ref_axis',(-1.,0.,0.));
#29262=DIRECTION('',(0.,0.,-1.));
#29263=DIRECTION('center_axis',(0.,0.,-1.));
#29264=DIRECTION('ref_axis',(0.,1.,0.));
#29265=DIRECTION('center_axis',(0.,0.,1.));
#29266=DIRECTION('ref_axis',(0.,1.,0.));
#29267=DIRECTION('',(0.,0.,1.));
#29268=DIRECTION('',(0.,0.,-1.));
#29269=DIRECTION('center_axis',(0.866025403784439,0.5,0.));
#29270=DIRECTION('ref_axis',(0.5,-0.866025403784439,0.));
#29271=DIRECTION('',(0.5,-0.866025403784439,0.));
#29272=DIRECTION('',(0.,0.,1.));
#29273=DIRECTION('center_axis',(0.,0.,-1.));
#29274=DIRECTION('ref_axis',(-0.570606204206288,-0.821223818286642,0.));
#29275=DIRECTION('center_axis',(0.,0.,1.));
#29276=DIRECTION('ref_axis',(-0.570606204206288,-0.821223818286642,0.));
#29277=DIRECTION('',(0.,0.,1.));
#29278=DIRECTION('',(0.,0.,-1.));
#29279=DIRECTION('center_axis',(0.,0.,-1.));
#29280=DIRECTION('ref_axis',(-1.,0.,0.));
#29281=DIRECTION('',(0.5,0.866025403784439,0.));
#29282=DIRECTION('center_axis',(0.,0.,1.));
#29283=DIRECTION('ref_axis',(1.,0.,0.));
#29284=DIRECTION('center_axis',(0.,0.,-1.));
#29285=DIRECTION('ref_axis',(-0.866025403784437,0.500000000000003,0.));
#29286=DIRECTION('center_axis',(0.,0.,1.));
#29287=DIRECTION('ref_axis',(-0.866025403784437,0.500000000000003,0.));
#29288=DIRECTION('',(0.,0.,1.));
#29289=DIRECTION('',(0.,0.,-1.));
#29290=DIRECTION('center_axis',(0.,0.,-1.));
#29291=DIRECTION('ref_axis',(-1.,0.,0.));
#29292=DIRECTION('',(1.,0.,0.));
#29293=DIRECTION('',(-0.5,0.866025403784439,0.));
#29294=DIRECTION('center_axis',(0.,0.,1.));
#29295=DIRECTION('ref_axis',(1.,0.,0.));
#29296=DIRECTION('center_axis',(-0.866025403784439,-0.5,0.));
#29297=DIRECTION('ref_axis',(-0.5,0.866025403784439,0.));
#29298=DIRECTION('',(0.,0.,-1.));
#29299=DIRECTION('center_axis',(0.,0.,-1.));
#29300=DIRECTION('ref_axis',(-0.996503790932232,0.0835475592563362,0.));
#29301=DIRECTION('center_axis',(0.,0.,1.));
#29302=DIRECTION('ref_axis',(-0.996503790932232,0.0835475592563362,0.));
#29303=DIRECTION('',(0.,0.,1.));
#29304=DIRECTION('',(0.,0.,-1.));
#29305=DIRECTION('center_axis',(0.,0.,-1.));
#29306=DIRECTION('ref_axis',(-1.,0.,0.));
#29307=DIRECTION('',(1.,0.,0.));
#29308=DIRECTION('center_axis',(0.,0.,1.));
#29309=DIRECTION('ref_axis',(1.,0.,0.));
#29310=DIRECTION('center_axis',(0.,0.,-1.));
#29311=DIRECTION('ref_axis',(0.,1.,0.));
#29312=DIRECTION('center_axis',(0.,0.,1.));
#29313=DIRECTION('ref_axis',(0.,1.,0.));
#29314=DIRECTION('',(0.,0.,1.));
#29315=DIRECTION('',(0.,0.,-1.));
#29316=DIRECTION('center_axis',(0.,0.,-1.));
#29317=DIRECTION('ref_axis',(-1.,0.,0.));
#29318=DIRECTION('',(0.5,-0.866025403784439,0.));
#29319=DIRECTION('',(0.5,0.866025403784439,0.));
#29320=DIRECTION('center_axis',(0.,0.,1.));
#29321=DIRECTION('ref_axis',(1.,0.,0.));
#29322=DIRECTION('center_axis',(-0.866025403784439,0.5,0.));
#29323=DIRECTION('ref_axis',(0.5,0.866025403784439,0.));
#29324=DIRECTION('',(0.,0.,-1.));
#29325=DIRECTION('center_axis',(0.,0.,-1.));
#29326=DIRECTION('ref_axis',(-0.425897586725943,0.904771377542978,0.));
#29327=DIRECTION('center_axis',(0.,0.,1.));
#29328=DIRECTION('ref_axis',(-0.425897586725943,0.904771377542978,0.));
#29329=DIRECTION('',(0.,0.,1.));
#29330=DIRECTION('',(0.,0.,-1.));
#29331=DIRECTION('center_axis',(0.,0.,-1.));
#29332=DIRECTION('ref_axis',(-1.,0.,0.));
#29333=DIRECTION('',(0.5,-0.866025403784439,0.));
#29334=DIRECTION('center_axis',(0.,0.,1.));
#29335=DIRECTION('ref_axis',(1.,0.,0.));
#29336=DIRECTION('center_axis',(0.,0.,1.));
#29337=DIRECTION('ref_axis',(1.,0.,0.));
#29338=DIRECTION('center_axis',(0.,0.,1.));
#29339=DIRECTION('ref_axis',(1.,0.,0.));
#29340=DIRECTION('center_axis',(0.,0.,1.));
#29341=DIRECTION('ref_axis',(1.,0.,0.));
#29342=DIRECTION('center_axis',(0.,0.,1.));
#29343=DIRECTION('ref_axis',(1.,0.,0.));
#29344=DIRECTION('center_axis',(0.,0.,1.));
#29345=DIRECTION('ref_axis',(1.,0.,0.));
#29346=DIRECTION('center_axis',(0.,0.,1.));
#29347=DIRECTION('ref_axis',(1.,0.,0.));
#29348=DIRECTION('',(0.,0.,1.));
#29349=DIRECTION('center_axis',(0.,0.,1.));
#29350=DIRECTION('ref_axis',(1.,0.,0.));
#29351=DIRECTION('center_axis',(0.,0.,1.));
#29352=DIRECTION('ref_axis',(1.,0.,0.));
#29353=DIRECTION('center_axis',(0.,0.,1.));
#29354=DIRECTION('ref_axis',(1.,0.,0.));
#29355=DIRECTION('center_axis',(0.,0.,1.));
#29356=DIRECTION('ref_axis',(1.,0.,0.));
#29357=DIRECTION('',(0.,0.,1.));
#29358=DIRECTION('center_axis',(0.,0.,1.));
#29359=DIRECTION('ref_axis',(1.,0.,0.));
#29360=DIRECTION('center_axis',(0.,0.,1.));
#29361=DIRECTION('ref_axis',(1.,0.,0.));
#29362=DIRECTION('center_axis',(-0.866025403784439,0.5,0.));
#29363=DIRECTION('ref_axis',(0.5,0.866025403784439,0.));
#29364=DIRECTION('center_axis',(-0.866025403784439,0.5,0.));
#29365=DIRECTION('ref_axis',(0.5,0.866025403784439,0.));
#29366=DIRECTION('center_axis',(-0.866025403784439,0.5,0.));
#29367=DIRECTION('ref_axis',(0.5,0.866025403784439,0.));
#29368=DIRECTION('center_axis',(-0.866025403784439,0.5,0.));
#29369=DIRECTION('ref_axis',(0.5,0.866025403784439,0.));
#29370=DIRECTION('center_axis',(-0.866025403784439,-0.5,0.));
#29371=DIRECTION('ref_axis',(-0.5,0.866025403784439,0.));
#29372=DIRECTION('center_axis',(-0.866025403784439,-0.5,0.));
#29373=DIRECTION('ref_axis',(-0.5,0.866025403784439,0.));
#29374=DIRECTION('center_axis',(-0.866025403784439,0.5,0.));
#29375=DIRECTION('ref_axis',(0.5,0.866025403784439,0.));
#29376=DIRECTION('center_axis',(-0.866025403784439,-0.5,0.));
#29377=DIRECTION('ref_axis',(-0.5,0.866025403784439,0.));
#29378=DIRECTION('center_axis',(-0.866025403784439,0.5,0.));
#29379=DIRECTION('ref_axis',(0.5,0.866025403784439,0.));
#29380=DIRECTION('center_axis',(0.866025403784439,0.5,0.));
#29381=DIRECTION('ref_axis',(0.5,-0.866025403784439,0.));
#29382=DIRECTION('center_axis',(-0.866025403784439,-0.5,0.));
#29383=DIRECTION('ref_axis',(-0.5,0.866025403784439,0.));
#29384=DIRECTION('center_axis',(-0.866025403784439,-0.5,0.));
#29385=DIRECTION('ref_axis',(-0.5,0.866025403784439,0.));
#29386=DIRECTION('center_axis',(-0.866025403784439,-0.5,0.));
#29387=DIRECTION('ref_axis',(-0.5,0.866025403784439,0.));
#29388=DIRECTION('center_axis',(-0.866025403784439,-0.5,0.));
#29389=DIRECTION('ref_axis',(-0.5,0.866025403784439,0.));
#29390=DIRECTION('center_axis',(0.866025403784439,0.5,0.));
#29391=DIRECTION('ref_axis',(0.5,-0.866025403784439,0.));
#29392=DIRECTION('center_axis',(-0.866025403784439,0.5,0.));
#29393=DIRECTION('ref_axis',(0.5,0.866025403784439,0.));
#29394=DIRECTION('center_axis',(-0.866025403784439,0.5,0.));
#29395=DIRECTION('ref_axis',(0.5,0.866025403784439,0.));
#29396=DIRECTION('center_axis',(-0.866025403784439,-0.5,0.));
#29397=DIRECTION('ref_axis',(-0.5,0.866025403784439,0.));
#29398=DIRECTION('center_axis',(-0.866025403784439,0.5,0.));
#29399=DIRECTION('ref_axis',(0.5,0.866025403784439,0.));
#29400=DIRECTION('center_axis',(-0.866025403784439,0.5,0.));
#29401=DIRECTION('ref_axis',(0.5,0.866025403784439,0.));
#29402=DIRECTION('center_axis',(0.,1.,0.));
#29403=DIRECTION('ref_axis',(1.,0.,0.));
#29404=DIRECTION('center_axis',(-0.866025403784439,-0.5,0.));
#29405=DIRECTION('ref_axis',(-0.5,0.866025403784439,0.));
#29406=DIRECTION('center_axis',(-0.866025403784439,0.5,0.));
#29407=DIRECTION('ref_axis',(0.5,0.866025403784439,0.));
#29408=DIRECTION('center_axis',(0.,1.,0.));
#29409=DIRECTION('ref_axis',(1.,0.,0.));
#29410=DIRECTION('center_axis',(-0.866025403784439,-0.5,0.));
#29411=DIRECTION('ref_axis',(-0.5,0.866025403784439,0.));
#29412=DIRECTION('center_axis',(-0.866025403784439,-0.5,0.));
#29413=DIRECTION('ref_axis',(-0.5,0.866025403784439,0.));
#29414=DIRECTION('center_axis',(-0.866025403784439,-0.5,0.));
#29415=DIRECTION('ref_axis',(-0.5,0.866025403784439,0.));
#29416=DIRECTION('center_axis',(-0.866025403784439,0.5,0.));
#29417=DIRECTION('ref_axis',(0.5,0.866025403784439,0.));
#29418=DIRECTION('center_axis',(0.,0.,1.));
#29419=DIRECTION('ref_axis',(1.,0.,0.));
#29420=DIRECTION('',(0.,0.,-1.));
#29421=DIRECTION('center_axis',(0.,0.,1.));
#29422=DIRECTION('ref_axis',(1.,0.,0.));
#29423=DIRECTION('center_axis',(0.,0.,-1.));
#29424=DIRECTION('ref_axis',(-1.,0.,0.));
#29425=DIRECTION('center_axis',(0.,0.,1.));
#29426=DIRECTION('ref_axis',(1.,0.,0.));
#29427=DIRECTION('center_axis',(0.,0.,1.));
#29428=DIRECTION('ref_axis',(1.,0.,0.));
#29429=DIRECTION('',(0.,0.,-1.));
#29430=DIRECTION('center_axis',(0.,0.,1.));
#29431=DIRECTION('ref_axis',(1.,0.,0.));
#29432=DIRECTION('',(0.,0.,-1.));
#29433=DIRECTION('axis',(0.,0.,1.));
#29434=DIRECTION('refdir',(1.,0.,0.));
#29435=DIRECTION('center_axis',(0.,0.,-1.));
#29436=DIRECTION('ref_axis',(-1.,0.,0.));
#29437=DIRECTION('center_axis',(0.,0.,-1.));
#29438=DIRECTION('ref_axis',(-1.,0.,0.));
#29439=DIRECTION('',(0.707106781186555,8.65956056235503E-17,-0.70710678118654));
#29440=DIRECTION('center_axis',(0.,0.,1.));
#29441=DIRECTION('ref_axis',(-1.,0.,0.));
#29442=DIRECTION('center_axis',(0.,0.,1.));
#29443=DIRECTION('ref_axis',(-1.,0.,0.));
#29444=DIRECTION('center_axis',(0.,0.,1.));
#29445=DIRECTION('ref_axis',(1.,0.,0.));
#29446=DIRECTION('',(0.,0.,-1.));
#29447=DIRECTION('center_axis',(0.,0.,-1.));
#29448=DIRECTION('ref_axis',(-1.,0.,0.));
#29449=DIRECTION('center_axis',(0.,0.,-1.));
#29450=DIRECTION('ref_axis',(-1.,0.,0.));
#29451=DIRECTION('center_axis',(0.,0.,1.));
#29452=DIRECTION('ref_axis',(1.,0.,0.));
#29453=DIRECTION('center_axis',(0.,0.,1.));
#29454=DIRECTION('ref_axis',(1.,0.,0.));
#29455=DIRECTION('center_axis',(0.,0.,1.));
#29456=DIRECTION('ref_axis',(-1.,0.,0.));
#29457=DIRECTION('',(-0.707106781186555,-8.65956056235503E-17,-0.70710678118654));
#29458=DIRECTION('center_axis',(0.,0.,1.));
#29459=DIRECTION('ref_axis',(-1.,0.,0.));
#29460=DIRECTION('center_axis',(0.,0.,-1.));
#29461=DIRECTION('ref_axis',(-1.,0.,0.));
#29462=DIRECTION('center_axis',(0.,0.,1.));
#29463=DIRECTION('ref_axis',(1.,0.,0.));
#29464=DIRECTION('center_axis',(0.,1.81500578188617E-15,1.));
#29465=DIRECTION('ref_axis',(-1.,2.94181504497177E-17,0.));
#29466=DIRECTION('center_axis',(0.,0.,-1.));
#29467=DIRECTION('ref_axis',(-1.,6.12323399573677E-17,0.));
#29468=DIRECTION('',(0.923879532511288,5.54251204061075E-16,0.382683432365087));
#29469=DIRECTION('center_axis',(0.,0.,1.));
#29470=DIRECTION('ref_axis',(-1.,0.,0.));
#29471=DIRECTION('center_axis',(0.,0.,1.));
#29472=DIRECTION('ref_axis',(-1.,0.,0.));
#29473=DIRECTION('center_axis',(0.,0.,1.));
#29474=DIRECTION('ref_axis',(-1.,6.12323399573677E-17,0.));
#29475=DIRECTION('',(0.707106781186543,-8.65956056235487E-17,0.707106781186552));
#29476=DIRECTION('center_axis',(0.,0.,1.));
#29477=DIRECTION('ref_axis',(1.,0.,0.));
#29478=DIRECTION('center_axis',(0.,0.,-1.));
#29479=DIRECTION('ref_axis',(-1.,1.22464679914735E-16,0.));
#29480=DIRECTION('center_axis',(0.,-7.42744751489879E-16,1.));
#29481=DIRECTION('ref_axis',(-1.,3.11479911548302E-17,0.));
#29482=DIRECTION('',(-0.382683432365058,6.51261289894839E-16,-0.9238795325113));
#29483=DIRECTION('center_axis',(0.,0.,-1.));
#29484=DIRECTION('ref_axis',(-1.,0.,0.));
#29485=DIRECTION('center_axis',(0.,0.,-1.));
#29486=DIRECTION('ref_axis',(-1.,0.,0.));
#29487=DIRECTION('center_axis',(0.,0.,1.));
#29488=DIRECTION('ref_axis',(1.,0.,0.));
#29489=DIRECTION('',(0.,0.,-1.));
#29490=DIRECTION('center_axis',(0.,0.,1.));
#29491=DIRECTION('ref_axis',(-1.,0.,0.));
#29492=DIRECTION('center_axis',(0.,0.,1.));
#29493=DIRECTION('ref_axis',(-1.,0.,0.));
#29494=DIRECTION('center_axis',(0.,-7.42744751489906E-16,-1.));
#29495=DIRECTION('ref_axis',(-1.,3.11479911548302E-17,0.));
#29496=DIRECTION('center_axis',(0.,0.,-1.));
#29497=DIRECTION('ref_axis',(-1.,6.12323399573677E-17,0.));
#29498=DIRECTION('',(-0.382683432365092,7.44991698001377E-16,0.923879532511286));
#29499=DIRECTION('center_axis',(0.,0.,-1.));
#29500=DIRECTION('ref_axis',(-1.,0.,0.));
#29501=DIRECTION('center_axis',(0.,0.,1.));
#29502=DIRECTION('ref_axis',(-1.,6.12323399573677E-17,0.));
#29503=DIRECTION('',(-0.707106781186543,8.65956056235487E-17,0.707106781186552));
#29504=DIRECTION('center_axis',(0.,1.81500578188617E-15,-1.));
#29505=DIRECTION('ref_axis',(-1.,2.94181504497177E-17,0.));
#29506=DIRECTION('',(0.923879532511285,7.80536426518631E-16,-0.382683432365095));
#29507=DIRECTION('center_axis',(0.,0.,-1.));
#29508=DIRECTION('ref_axis',(-1.,0.,0.));
#29509=DIRECTION('center_axis',(0.,0.,-1.));
#29510=DIRECTION('ref_axis',(-1.,0.,0.));
#29511=DIRECTION('center_axis',(0.,0.,1.));
#29512=DIRECTION('ref_axis',(-1.,0.,0.));
#29513=DIRECTION('center_axis',(0.,0.,1.));
#29514=DIRECTION('ref_axis',(-1.,0.,0.));
#29515=DIRECTION('center_axis',(0.,0.,-1.));
#29516=DIRECTION('ref_axis',(-1.,0.,0.));
#29517=DIRECTION('center_axis',(0.,0.,-1.));
#29518=DIRECTION('ref_axis',(-1.,0.,0.));
#29519=DIRECTION('',(-0.707106781186555,-8.65956056235503E-17,-0.70710678118654));
#29520=DIRECTION('center_axis',(0.,0.,1.));
#29521=DIRECTION('ref_axis',(1.,0.,0.));
#29522=DIRECTION('',(0.,0.,-1.));
#29523=DIRECTION('center_axis',(0.,0.,1.));
#29524=DIRECTION('ref_axis',(1.,0.,0.));
#29525=DIRECTION('center_axis',(1.22464679914735E-16,-1.,0.));
#29526=DIRECTION('ref_axis',(-1.,-1.22464679914735E-16,0.));
#29527=DIRECTION('center_axis',(0.,0.,1.));
#29528=DIRECTION('ref_axis',(-1.,1.22464679914735E-16,0.));
#29529=DIRECTION('center_axis',(0.,0.,1.));
#29530=DIRECTION('ref_axis',(1.,0.,0.));
#29531=DIRECTION('',(0.,0.,-1.));
#29532=DIRECTION('center_axis',(0.,0.,-1.));
#29533=DIRECTION('ref_axis',(-1.,1.22464679914735E-16,0.));
#29534=DIRECTION('center_axis',(0.,0.,1.));
#29535=DIRECTION('ref_axis',(1.,0.,0.));
#29536=DIRECTION('center_axis',(1.22464679914735E-16,-1.,0.));
#29537=DIRECTION('ref_axis',(-1.,-1.22464679914735E-16,0.));
#29538=DIRECTION('center_axis',(0.,0.,1.));
#29539=DIRECTION('ref_axis',(-1.,0.,0.));
#29540=DIRECTION('center_axis',(0.,0.,1.));
#29541=DIRECTION('ref_axis',(1.,0.,0.));
#29542=DIRECTION('',(0.600000000000001,7.34788079488414E-17,-0.799999999999999));
#29543=DIRECTION('center_axis',(0.,0.,1.));
#29544=DIRECTION('ref_axis',(1.,0.,0.));
#29545=DIRECTION('center_axis',(0.,0.,1.));
#29546=DIRECTION('ref_axis',(1.,0.,0.));
#29547=DIRECTION('',(0.,0.,-1.));
#29548=DIRECTION('axis',(0.,0.,1.));
#29549=DIRECTION('refdir',(1.,0.,0.));
#29550=DIRECTION('center_axis',(0.,0.,-1.));
#29551=DIRECTION('ref_axis',(-1.,0.,0.));
#29552=DIRECTION('center_axis',(0.,0.,-1.));
#29553=DIRECTION('ref_axis',(-1.,0.,0.));
#29554=DIRECTION('',(-0.707106781186555,8.65956056235503E-17,0.70710678118654));
#29555=DIRECTION('center_axis',(0.,0.,1.));
#29556=DIRECTION('ref_axis',(-1.,0.,0.));
#29557=DIRECTION('center_axis',(0.,0.,1.));
#29558=DIRECTION('ref_axis',(-1.,0.,0.));
#29559=DIRECTION('center_axis',(0.,0.,-1.));
#29560=DIRECTION('ref_axis',(-1.,0.,0.));
#29561=DIRECTION('center_axis',(0.,0.,1.));
#29562=DIRECTION('ref_axis',(-1.,0.,0.));
#29563=DIRECTION('center_axis',(0.,0.,1.));
#29564=DIRECTION('ref_axis',(1.,0.,0.));
#29565=DIRECTION('center_axis',(0.,0.,1.));
#29566=DIRECTION('ref_axis',(1.,0.,0.));
#29567=DIRECTION('center_axis',(0.,0.,1.));
#29568=DIRECTION('ref_axis',(1.,0.,0.));
#29569=DIRECTION('center_axis',(0.,0.,1.));
#29570=DIRECTION('ref_axis',(1.,0.,0.));
#29571=DIRECTION('',(0.,0.,-1.));
#29572=DIRECTION('center_axis',(0.,4.39101262113477E-15,1.));
#29573=DIRECTION('ref_axis',(-1.,-3.11403559978336E-17,0.));
#29574=DIRECTION('center_axis',(0.,0.,-1.));
#29575=DIRECTION('ref_axis',(-1.,-6.12323399573677E-17,0.));
#29576=DIRECTION('',(-0.923879532511284,-1.8222803301846E-15,-0.382683432365097));
#29577=DIRECTION('center_axis',(0.,0.,1.));
#29578=DIRECTION('ref_axis',(-1.,0.,0.));
#29579=DIRECTION('center_axis',(0.,0.,1.));
#29580=DIRECTION('ref_axis',(-1.,-6.12323399573677E-17,0.));
#29581=DIRECTION('',(-0.707106781186543,-8.65956056235487E-17,-0.707106781186552));
#29582=DIRECTION('center_axis',(0.,-1.82787223937844E-15,1.));
#29583=DIRECTION('ref_axis',(-1.,-3.04052209636688E-17,0.));
#29584=DIRECTION('',(0.382683432365093,-1.72396337974038E-15,0.923879532511285));
#29585=DIRECTION('center_axis',(0.,0.,-1.));
#29586=DIRECTION('ref_axis',(-1.,0.,0.));
#29587=DIRECTION('center_axis',(0.,0.,-1.));
#29588=DIRECTION('ref_axis',(-1.,0.,0.));
#29589=DIRECTION('center_axis',(0.,0.,1.));
#29590=DIRECTION('ref_axis',(1.,0.,0.));
#29591=DIRECTION('center_axis',(0.,0.,1.));
#29592=DIRECTION('ref_axis',(-1.,0.,0.));
#29593=DIRECTION('center_axis',(0.,0.,1.));
#29594=DIRECTION('ref_axis',(-1.,0.,0.));
#29595=DIRECTION('',(0.,0.,-1.));
#29596=DIRECTION('center_axis',(0.,-1.82787223937844E-15,-1.));
#29597=DIRECTION('ref_axis',(-1.,-3.04052209636688E-17,0.));
#29598=DIRECTION('center_axis',(0.,0.,-1.));
#29599=DIRECTION('ref_axis',(-1.,-6.12323399573677E-17,0.));
#29600=DIRECTION('',(0.382683432365093,-1.63023297163385E-15,-0.923879532511285));
#29601=DIRECTION('center_axis',(0.,0.,-1.));
#29602=DIRECTION('ref_axis',(-1.,0.,0.));
#29603=DIRECTION('center_axis',(0.,0.,1.));
#29604=DIRECTION('ref_axis',(-1.,-6.12323399573677E-17,0.));
#29605=DIRECTION('',(0.707106781186543,8.65956056235487E-17,-0.707106781186552));
#29606=DIRECTION('center_axis',(0.,0.,-1.));
#29607=DIRECTION('ref_axis',(-1.,0.,0.));
#29608=DIRECTION('center_axis',(0.,0.,-1.));
#29609=DIRECTION('ref_axis',(-1.,0.,0.));
#29610=DIRECTION('',(-0.707106781186555,8.65956056235503E-17,0.70710678118654));
#29611=DIRECTION('center_axis',(0.,0.,1.));
#29612=DIRECTION('ref_axis',(-1.,0.,0.));
#29613=DIRECTION('center_axis',(0.,0.,1.));
#29614=DIRECTION('ref_axis',(-1.,0.,0.));
#29615=DIRECTION('center_axis',(0.,0.,1.));
#29616=DIRECTION('ref_axis',(1.,0.,0.));
#29617=DIRECTION('center_axis',(0.,0.,-1.));
#29618=DIRECTION('ref_axis',(-1.,0.,0.));
#29619=DIRECTION('center_axis',(0.,0.,-1.));
#29620=DIRECTION('ref_axis',(-1.,0.,0.));
#29621=DIRECTION('',(0.,0.,-1.));
#29622=DIRECTION('center_axis',(0.,0.,-1.));
#29623=DIRECTION('ref_axis',(-1.,0.,0.));
#29624=DIRECTION('center_axis',(0.,4.39101262113477E-15,-1.));
#29625=DIRECTION('ref_axis',(-1.,-3.11403559978336E-17,0.));
#29626=DIRECTION('',(-0.923879532511284,-1.59599510772706E-15,0.382683432365097));
#29627=DIRECTION('center_axis',(0.,0.,-1.));
#29628=DIRECTION('ref_axis',(-1.,0.,0.));
#29629=DIRECTION('center_axis',(0.,0.,-1.));
#29630=DIRECTION('ref_axis',(-1.,0.,0.));
#29631=DIRECTION('center_axis',(0.,0.,-1.));
#29632=DIRECTION('ref_axis',(-1.,0.,0.));
#29633=DIRECTION('center_axis',(0.,0.,1.));
#29634=DIRECTION('ref_axis',(-1.,0.,0.));
#29635=DIRECTION('center_axis',(0.,0.,1.));
#29636=DIRECTION('ref_axis',(-1.,0.,0.));
#29637=DIRECTION('',(-0.707106781186555,-8.65956056235503E-17,-0.70710678118654));
#29638=DIRECTION('center_axis',(0.,0.,-1.));
#29639=DIRECTION('ref_axis',(-1.,0.,0.));
#29640=DIRECTION('center_axis',(0.,0.,-1.));
#29641=DIRECTION('ref_axis',(-1.,0.,0.));
#29642=DIRECTION('center_axis',(0.,0.,1.));
#29643=DIRECTION('ref_axis',(-1.,0.,0.));
#29644=DIRECTION('center_axis',(0.,0.,1.));
#29645=DIRECTION('ref_axis',(1.,0.,0.));
#29646=DIRECTION('center_axis',(0.,0.,1.));
#29647=DIRECTION('ref_axis',(1.,0.,0.));
#29648=DIRECTION('',(0.,0.,1.));
#29649=DIRECTION('center_axis',(0.,0.,1.));
#29650=DIRECTION('ref_axis',(-1.,0.,0.));
#29651=DIRECTION('center_axis',(0.,0.,1.));
#29652=DIRECTION('ref_axis',(-1.,0.,0.));
#29653=DIRECTION('',(-0.707106781186555,-8.65956056235503E-17,-0.70710678118654));
#29654=DIRECTION('center_axis',(0.,0.,-1.));
#29655=DIRECTION('ref_axis',(-1.,0.,0.));
#29656=DIRECTION('center_axis',(0.,0.,-1.));
#29657=DIRECTION('ref_axis',(-1.,0.,0.));
#29658=DIRECTION('center_axis',(0.,0.,1.));
#29659=DIRECTION('ref_axis',(-1.,0.,0.));
#29660=DIRECTION('center_axis',(0.,0.,1.));
#29661=DIRECTION('ref_axis',(1.,0.,0.));
#29662=DIRECTION('center_axis',(0.,0.,1.));
#29663=DIRECTION('ref_axis',(1.,0.,0.));
#29664=DIRECTION('',(0.,0.,1.));
#29665=DIRECTION('center_axis',(0.,0.,-1.));
#29666=DIRECTION('ref_axis',(1.,0.,0.));
#29667=DIRECTION('',(0.316227766016841,3.87267321454042E-17,0.948683298050513));
#29668=DIRECTION('center_axis',(0.,0.,1.));
#29669=DIRECTION('ref_axis',(1.,0.,0.));
#29670=DIRECTION('center_axis',(0.,0.,1.));
#29671=DIRECTION('ref_axis',(1.,0.,0.));
#29672=DIRECTION('',(0.,0.,1.));
#29673=DIRECTION('center_axis',(0.,0.,1.));
#29674=DIRECTION('ref_axis',(1.,0.,0.));
#29675=DIRECTION('center_axis',(0.,0.,1.));
#29676=DIRECTION('ref_axis',(1.,0.,0.));
#29677=DIRECTION('',(-0.707106781186542,-8.65956056235487E-17,0.707106781186553));
#29678=DIRECTION('center_axis',(0.,0.,1.));
#29679=DIRECTION('ref_axis',(1.,0.,0.));
#29680=DIRECTION('center_axis',(0.,0.,-1.));
#29681=DIRECTION('ref_axis',(-1.,0.,0.));
#29682=DIRECTION('center_axis',(0.,0.,-1.));
#29683=DIRECTION('ref_axis',(1.,0.,0.));
#29684=DIRECTION('',(0.316227766016841,3.87267321454042E-17,0.948683298050513));
#29685=DIRECTION('center_axis',(0.,0.,1.));
#29686=DIRECTION('ref_axis',(1.,0.,0.));
#29687=DIRECTION('center_axis',(0.,0.,1.));
#29688=DIRECTION('ref_axis',(1.,0.,0.));
#29689=DIRECTION('',(0.,0.,1.));
#29690=DIRECTION('center_axis',(0.,0.,1.));
#29691=DIRECTION('ref_axis',(1.,0.,0.));
#29692=DIRECTION('center_axis',(0.,0.,1.));
#29693=DIRECTION('ref_axis',(1.,0.,0.));
#29694=DIRECTION('',(-0.707106781186542,-8.65956056235487E-17,0.707106781186553));
#29695=DIRECTION('center_axis',(0.,0.,1.));
#29696=DIRECTION('ref_axis',(1.,0.,0.));
#29697=DIRECTION('center_axis',(0.,0.,-1.));
#29698=DIRECTION('ref_axis',(-1.,0.,0.));
#29699=DIRECTION('center_axis',(0.,0.,1.));
#29700=DIRECTION('ref_axis',(-1.,0.,0.));
#29701=DIRECTION('',(0.707106781186555,-8.65956056235503E-17,0.70710678118654));
#29702=DIRECTION('center_axis',(0.,0.,1.));
#29703=DIRECTION('ref_axis',(-1.,0.,0.));
#29704=DIRECTION('center_axis',(0.,0.,1.));
#29705=DIRECTION('ref_axis',(1.,0.,0.));
#29706=DIRECTION('axis',(0.,0.,1.));
#29707=DIRECTION('refdir',(1.,0.,0.));
#29708=DIRECTION('center_axis',(0.,0.,1.));
#29709=DIRECTION('ref_axis',(1.,0.,0.));
#29710=DIRECTION('center_axis',(0.,0.,1.));
#29711=DIRECTION('ref_axis',(1.,0.,0.));
#29712=DIRECTION('',(0.,0.,1.));
#29713=DIRECTION('center_axis',(0.,0.,-1.));
#29714=DIRECTION('ref_axis',(1.,0.,0.));
#29715=DIRECTION('center_axis',(0.,0.,1.));
#29716=DIRECTION('ref_axis',(1.,0.,0.));
#29717=DIRECTION('center_axis',(0.,0.,1.));
#29718=DIRECTION('ref_axis',(1.,0.,0.));
#29719=DIRECTION('',(0.,0.,1.));
#29720=DIRECTION('center_axis',(0.,0.,-1.));
#29721=DIRECTION('ref_axis',(1.,0.,0.));
#29722=DIRECTION('center_axis',(0.,0.,1.));
#29723=DIRECTION('ref_axis',(1.,0.,0.));
#29724=DIRECTION('center_axis',(0.,0.,1.));
#29725=DIRECTION('ref_axis',(1.,0.,0.));
#29726=DIRECTION('',(0.,0.,1.));
#29727=DIRECTION('center_axis',(0.,0.,1.));
#29728=DIRECTION('ref_axis',(1.,0.,0.));
#29729=DIRECTION('center_axis',(0.,0.,1.));
#29730=DIRECTION('ref_axis',(1.,0.,0.));
#29731=DIRECTION('',(-0.707106781186548,-8.65956056235493E-17,0.707106781186548));
#29732=DIRECTION('center_axis',(0.,0.,-1.));
#29733=DIRECTION('ref_axis',(1.,0.,0.));
#29734=DIRECTION('center_axis',(0.,0.,1.));
#29735=DIRECTION('ref_axis',(1.,0.,0.));
#29736=DIRECTION('center_axis',(0.,0.,1.));
#29737=DIRECTION('ref_axis',(1.,0.,0.));
#29738=DIRECTION('',(0.,0.,1.));
#29739=DIRECTION('center_axis',(0.,0.,-1.));
#29740=DIRECTION('ref_axis',(1.,0.,0.));
#29741=DIRECTION('center_axis',(0.,0.,1.));
#29742=DIRECTION('ref_axis',(1.,0.,0.));
#29743=DIRECTION('center_axis',(0.,0.,1.));
#29744=DIRECTION('ref_axis',(1.,0.,0.));
#29745=DIRECTION('',(0.,0.,1.));
#29746=DIRECTION('center_axis',(0.,0.,-1.));
#29747=DIRECTION('ref_axis',(1.,0.,0.));
#29748=DIRECTION('center_axis',(0.,0.,1.));
#29749=DIRECTION('ref_axis',(1.,0.,0.));
#29750=DIRECTION('center_axis',(0.,0.,1.));
#29751=DIRECTION('ref_axis',(1.,0.,0.));
#29752=DIRECTION('',(0.,0.,1.));
#29753=DIRECTION('center_axis',(0.,0.,-1.));
#29754=DIRECTION('ref_axis',(1.,0.,0.));
#29755=DIRECTION('center_axis',(0.,0.,1.));
#29756=DIRECTION('ref_axis',(1.,0.,0.));
#29757=DIRECTION('center_axis',(0.,0.,1.));
#29758=DIRECTION('ref_axis',(1.,0.,0.));
#29759=DIRECTION('',(0.,0.,1.));
#29760=DIRECTION('center_axis',(0.,0.,-1.));
#29761=DIRECTION('ref_axis',(1.,0.,0.));
#29762=DIRECTION('center_axis',(0.,0.,1.));
#29763=DIRECTION('ref_axis',(1.,0.,0.));
#29764=DIRECTION('center_axis',(0.,0.,1.));
#29765=DIRECTION('ref_axis',(1.,0.,0.));
#29766=DIRECTION('',(0.,0.,1.));
#29767=DIRECTION('center_axis',(0.,0.,-1.));
#29768=DIRECTION('ref_axis',(1.,0.,0.));
#29769=DIRECTION('center_axis',(0.,0.,1.));
#29770=DIRECTION('ref_axis',(1.,0.,0.));
#29771=DIRECTION('center_axis',(0.,0.,1.));
#29772=DIRECTION('ref_axis',(1.,0.,0.));
#29773=DIRECTION('',(0.,0.,1.));
#29774=DIRECTION('center_axis',(0.,0.,-1.));
#29775=DIRECTION('ref_axis',(1.,0.,0.));
#29776=DIRECTION('center_axis',(0.,0.,-1.));
#29777=DIRECTION('ref_axis',(-1.,0.,0.));
#29778=DIRECTION('center_axis',(0.,0.,-1.));
#29779=DIRECTION('ref_axis',(-1.,0.,0.));
#29780=DIRECTION('',(-0.707106781186555,8.65956056235503E-17,0.70710678118654));
#29781=DIRECTION('center_axis',(0.,0.,1.));
#29782=DIRECTION('ref_axis',(-1.,0.,0.));
#29783=DIRECTION('center_axis',(0.,0.,1.));
#29784=DIRECTION('ref_axis',(-1.,0.,0.));
#29785=DIRECTION('center_axis',(0.,0.,1.));
#29786=DIRECTION('ref_axis',(1.,0.,0.));
#29787=DIRECTION('center_axis',(0.,0.,-1.));
#29788=DIRECTION('ref_axis',(-1.,0.,0.));
#29789=DIRECTION('center_axis',(0.,0.,-1.));
#29790=DIRECTION('ref_axis',(-1.,0.,0.));
#29791=DIRECTION('',(0.,0.,-1.));
#29792=DIRECTION('center_axis',(0.,0.,-1.));
#29793=DIRECTION('ref_axis',(-1.,0.,0.));
#29794=DIRECTION('center_axis',(0.,0.,1.));
#29795=DIRECTION('ref_axis',(-1.,0.,0.));
#29796=DIRECTION('center_axis',(0.,0.,1.));
#29797=DIRECTION('ref_axis',(-1.,0.,0.));
#29798=DIRECTION('',(0.707106781186555,-8.65956056235503E-17,0.70710678118654));
#29799=DIRECTION('center_axis',(0.,0.,1.));
#29800=DIRECTION('ref_axis',(-1.,0.,0.));
#29801=DIRECTION('center_axis',(0.,0.,1.));
#29802=DIRECTION('ref_axis',(1.,0.,0.));
#29803=DIRECTION('center_axis',(0.,0.,-1.));
#29804=DIRECTION('ref_axis',(-1.,0.,0.));
#29805=DIRECTION('center_axis',(0.,0.,-1.));
#29806=DIRECTION('ref_axis',(-1.,0.,0.));
#29807=DIRECTION('',(0.707106781186553,8.659560562355E-17,-0.707106781186542));
#29808=DIRECTION('center_axis',(0.,0.,1.));
#29809=DIRECTION('ref_axis',(-1.,0.,0.));
#29810=DIRECTION('center_axis',(0.,0.,1.));
#29811=DIRECTION('ref_axis',(-1.,0.,0.));
#29812=DIRECTION('center_axis',(0.,0.,1.));
#29813=DIRECTION('ref_axis',(1.,0.,0.));
#29814=DIRECTION('',(0.,0.,-1.));
#29815=DIRECTION('center_axis',(0.,0.,-1.));
#29816=DIRECTION('ref_axis',(-1.,0.,0.));
#29817=DIRECTION('center_axis',(0.,0.,-1.));
#29818=DIRECTION('ref_axis',(-1.,0.,0.));
#29819=DIRECTION('center_axis',(0.,0.,1.));
#29820=DIRECTION('ref_axis',(-1.,0.,0.));
#29821=DIRECTION('',(-0.707106781186553,-8.659560562355E-17,-0.707106781186542));
#29822=DIRECTION('axis',(0.,0.,1.));
#29823=DIRECTION('refdir',(1.,0.,0.));
#29824=DIRECTION('center_axis',(0.,0.,1.));
#29825=DIRECTION('ref_axis',(1.,0.,0.));
#29826=DIRECTION('',(-0.857167300702112,-1.04972719113862E-16,0.515038074910054));
#29827=DIRECTION('center_axis',(0.,0.,1.));
#29828=DIRECTION('ref_axis',(1.,0.,0.));
#29829=DIRECTION('center_axis',(0.,0.,1.));
#29830=DIRECTION('ref_axis',(1.,0.,0.));
#29831=DIRECTION('',(0.,0.,1.));
#29832=DIRECTION('center_axis',(0.,0.,-1.));
#29833=DIRECTION('ref_axis',(1.,0.,0.));
#29834=DIRECTION('center_axis',(0.,0.,1.));
#29835=DIRECTION('ref_axis',(1.,0.,0.));
#29836=DIRECTION('',(-0.857167300702112,-1.04972719113862E-16,0.515038074910054));
#29837=DIRECTION('center_axis',(0.,0.,1.));
#29838=DIRECTION('ref_axis',(1.,0.,0.));
#29839=DIRECTION('center_axis',(0.,0.,1.));
#29840=DIRECTION('ref_axis',(1.,0.,0.));
#29841=DIRECTION('',(0.,0.,1.));
#29842=DIRECTION('center_axis',(0.,0.,-1.));
#29843=DIRECTION('ref_axis',(1.,0.,0.));
#29844=DIRECTION('center_axis',(0.,0.,-1.));
#29845=DIRECTION('ref_axis',(1.,0.,0.));
#29846=DIRECTION('center_axis',(0.,0.,-1.));
#29847=DIRECTION('ref_axis',(1.,0.,0.));
#29848=DIRECTION('',(0.,0.,1.));
#29849=DIRECTION('center_axis',(0.,0.,1.));
#29850=DIRECTION('ref_axis',(1.,0.,0.));
#29851=DIRECTION('center_axis',(0.,0.,1.));
#29852=DIRECTION('ref_axis',(1.,0.,0.));
#29853=DIRECTION('center_axis',(0.,0.,-1.));
#29854=DIRECTION('ref_axis',(-1.,0.,0.));
#29855=DIRECTION('center_axis',(0.,0.,1.));
#29856=DIRECTION('ref_axis',(1.,0.,0.));
#29857=DIRECTION('center_axis',(0.,0.,1.));
#29858=DIRECTION('ref_axis',(1.,0.,0.));
#29859=DIRECTION('center_axis',(0.,0.,1.));
#29860=DIRECTION('ref_axis',(1.,0.,0.));
#29861=DIRECTION('',(0.707106781186548,8.65956056235493E-17,-0.707106781186548));
#29862=DIRECTION('center_axis',(0.,0.,1.));
#29863=DIRECTION('ref_axis',(1.,0.,0.));
#29864=DIRECTION('center_axis',(0.,0.,1.));
#29865=DIRECTION('ref_axis',(1.,0.,0.));
#29866=DIRECTION('',(0.,0.,-1.));
#29867=DIRECTION('center_axis',(0.,0.,1.));
#29868=DIRECTION('ref_axis',(1.,0.,0.));
#29869=DIRECTION('center_axis',(0.,0.,1.));
#29870=DIRECTION('ref_axis',(1.,0.,0.));
#29871=DIRECTION('',(0.,0.,1.));
#29872=DIRECTION('center_axis',(0.,0.,1.));
#29873=DIRECTION('ref_axis',(1.,0.,0.));
#29874=DIRECTION('center_axis',(0.,0.,-1.));
#29875=DIRECTION('ref_axis',(-1.,0.,0.));
#29876=DIRECTION('center_axis',(0.,0.,-1.));
#29877=DIRECTION('ref_axis',(1.,0.,0.));
#29878=DIRECTION('center_axis',(0.,0.,1.));
#29879=DIRECTION('ref_axis',(1.,0.,0.));
#29880=DIRECTION('center_axis',(0.,0.,1.));
#29881=DIRECTION('ref_axis',(1.,0.,0.));
#29882=DIRECTION('center_axis',(0.,0.,1.));
#29883=DIRECTION('ref_axis',(1.,0.,0.));
#29884=DIRECTION('center_axis',(0.,0.,1.));
#29885=DIRECTION('ref_axis',(1.,0.,0.));
#29886=DIRECTION('',(0.,0.,-1.));
#29887=DIRECTION('center_axis',(0.,0.,-1.));
#29888=DIRECTION('ref_axis',(-1.,0.,0.));
#29889=DIRECTION('center_axis',(0.,0.,1.));
#29890=DIRECTION('ref_axis',(1.,0.,0.));
#29891=DIRECTION('center_axis',(0.,0.,1.));
#29892=DIRECTION('ref_axis',(1.,0.,0.));
#29893=DIRECTION('center_axis',(0.,0.,1.));
#29894=DIRECTION('ref_axis',(1.,0.,0.));
#29895=DIRECTION('',(0.707106781186551,8.65956056235498E-17,-0.707106781186544));
#29896=DIRECTION('center_axis',(0.,0.,1.));
#29897=DIRECTION('ref_axis',(1.,0.,0.));
#29898=DIRECTION('',(0.,0.,-1.));
#29899=DIRECTION('center_axis',(0.,0.,-1.));
#29900=DIRECTION('ref_axis',(1.,0.,0.));
#29901=DIRECTION('center_axis',(0.,0.,1.));
#29902=DIRECTION('ref_axis',(1.,0.,0.));
#29903=DIRECTION('',(-0.707106781186548,-8.65956056235494E-17,-0.707106781186547));
#29904=DIRECTION('center_axis',(0.,0.,1.));
#29905=DIRECTION('ref_axis',(1.,0.,0.));
#29906=DIRECTION('center_axis',(0.,0.,1.));
#29907=DIRECTION('ref_axis',(1.,0.,0.));
#29908=DIRECTION('center_axis',(0.,0.,1.));
#29909=DIRECTION('ref_axis',(1.,0.,0.));
#29910=DIRECTION('center_axis',(0.,0.,1.));
#29911=DIRECTION('ref_axis',(1.,0.,0.));
#29912=DIRECTION('',(0.,0.,-1.));
#29913=DIRECTION('center_axis',(0.,0.,1.));
#29914=DIRECTION('ref_axis',(1.,0.,0.));
#29915=DIRECTION('center_axis',(0.,0.,1.));
#29916=DIRECTION('ref_axis',(1.,0.,0.));
#29917=DIRECTION('center_axis',(0.,0.,1.));
#29918=DIRECTION('ref_axis',(1.,0.,0.));
#29919=DIRECTION('center_axis',(0.,0.,1.));
#29920=DIRECTION('ref_axis',(1.,0.,0.));
#29921=DIRECTION('',(0.,0.,-1.));
#29922=DIRECTION('center_axis',(0.,0.,-1.));
#29923=DIRECTION('ref_axis',(1.,0.,0.));
#29924=DIRECTION('center_axis',(0.,0.,1.));
#29925=DIRECTION('ref_axis',(1.,0.,0.));
#29926=DIRECTION('',(-0.707106781186549,-8.65956056235496E-17,-0.707106781186546));
#29927=DIRECTION('center_axis',(0.,0.,1.));
#29928=DIRECTION('ref_axis',(1.,0.,0.));
#29929=DIRECTION('axis',(0.,0.,1.));
#29930=DIRECTION('refdir',(1.,0.,0.));
#29931=DIRECTION('center_axis',(0.,0.,-1.));
#29932=DIRECTION('ref_axis',(-1.,0.,0.));
#29933=DIRECTION('center_axis',(0.,0.,-1.));
#29934=DIRECTION('ref_axis',(-1.,0.,0.));
#29935=DIRECTION('',(0.707106781186555,8.65956056235503E-17,-0.70710678118654));
#29936=DIRECTION('center_axis',(0.,0.,1.));
#29937=DIRECTION('ref_axis',(-1.,0.,0.));
#29938=DIRECTION('center_axis',(0.,0.,1.));
#29939=DIRECTION('ref_axis',(-1.,0.,0.));
#29940=DIRECTION('center_axis',(0.,0.,1.));
#29941=DIRECTION('ref_axis',(1.,0.,0.));
#29942=DIRECTION('center_axis',(0.,0.,1.));
#29943=DIRECTION('ref_axis',(-1.,0.,0.));
#29944=DIRECTION('center_axis',(0.,0.,1.));
#29945=DIRECTION('ref_axis',(1.,0.,0.));
#29946=DIRECTION('',(0.,0.,-1.));
#29947=DIRECTION('center_axis',(0.,0.,1.));
#29948=DIRECTION('ref_axis',(1.,0.,0.));
#29949=DIRECTION('center_axis',(0.,0.,1.));
#29950=DIRECTION('ref_axis',(-1.,0.,0.));
#29951=DIRECTION('center_axis',(0.,0.,-1.));
#29952=DIRECTION('ref_axis',(-1.,0.,0.));
#29953=DIRECTION('center_axis',(0.,0.,-1.));
#29954=DIRECTION('ref_axis',(-1.,0.,0.));
#29955=DIRECTION('',(0.707106781186555,-8.65956056235502E-17,0.70710678118654));
#29956=DIRECTION('center_axis',(0.,0.,1.));
#29957=DIRECTION('ref_axis',(1.,0.,0.));
#29958=DIRECTION('',(0.,0.,-1.));
#29959=DIRECTION('center_axis',(0.,0.,1.));
#29960=DIRECTION('ref_axis',(-1.,0.,0.));
#29961=DIRECTION('',(0.,0.,1.));
#29962=DIRECTION('',(0.,0.,-1.));
#29963=DIRECTION('center_axis',(0.,0.,1.));
#29964=DIRECTION('ref_axis',(-1.,0.,0.));
#29965=DIRECTION('center_axis',(0.,0.,-1.));
#29966=DIRECTION('ref_axis',(-1.,0.,0.));
#29967=DIRECTION('center_axis',(0.,0.,-1.));
#29968=DIRECTION('ref_axis',(-1.,0.,0.));
#29969=DIRECTION('',(-0.707106781186555,8.65956056235503E-17,0.70710678118654));
#29970=DIRECTION('center_axis',(0.,0.,-1.));
#29971=DIRECTION('ref_axis',(-1.,0.,0.));
#29972=DIRECTION('center_axis',(0.,0.,1.));
#29973=DIRECTION('ref_axis',(-1.,0.,0.));
#29974=DIRECTION('',(-0.592241372047889,-0.805760607894698,-4.99896642157306E-14));
#29975=DIRECTION('center_axis',(0.,0.,1.));
#29976=DIRECTION('ref_axis',(-1.,-7.64599154681893E-13,0.));
#29977=DIRECTION('center_axis',(0.,0.,-1.));
#29978=DIRECTION('ref_axis',(-1.,0.,0.));
#29979=DIRECTION('center_axis',(0.,0.,1.));
#29980=DIRECTION('ref_axis',(1.,0.,0.));
#29981=DIRECTION('center_axis',(0.,0.,1.));
#29982=DIRECTION('ref_axis',(-1.,0.,0.));
#29983=DIRECTION('',(-0.707106781186555,-8.65956056235503E-17,-0.70710678118654));
#29984=DIRECTION('center_axis',(1.,0.,0.));
#29985=DIRECTION('ref_axis',(0.,1.,0.));
#29986=DIRECTION('center_axis',(1.,0.,0.));
#29987=DIRECTION('ref_axis',(0.,0.,-1.));
#29988=DIRECTION('center_axis',(1.,0.,0.));
#29989=DIRECTION('ref_axis',(0.,0.,-1.));
#29990=DIRECTION('',(1.,0.,0.));
#29991=DIRECTION('center_axis',(1.,0.,0.));
#29992=DIRECTION('ref_axis',(0.,0.,-1.));
#29993=DIRECTION('center_axis',(0.,0.,-1.));
#29994=DIRECTION('ref_axis',(1.,0.,0.));
#29995=DIRECTION('center_axis',(0.,0.,-1.));
#29996=DIRECTION('ref_axis',(1.,0.,0.));
#29997=DIRECTION('',(0.707106781186555,-8.65956056235503E-17,0.70710678118654));
#29998=DIRECTION('center_axis',(0.,0.,1.));
#29999=DIRECTION('ref_axis',(1.,0.,0.));
#30000=DIRECTION('center_axis',(0.,0.,1.));
#30001=DIRECTION('ref_axis',(1.,0.,0.));
#30002=DIRECTION('',(0.,0.,1.));
#30003=DIRECTION('center_axis',(0.,0.,-1.));
#30004=DIRECTION('ref_axis',(1.,0.,0.));
#30005=DIRECTION('center_axis',(0.,0.,-1.));
#30006=DIRECTION('ref_axis',(-1.,0.,0.));
#30007=DIRECTION('center_axis',(0.,0.,1.));
#30008=DIRECTION('ref_axis',(-1.,0.,0.));
#30009=DIRECTION('center_axis',(0.,0.,-1.));
#30010=DIRECTION('ref_axis',(1.,0.,0.));
#30011=DIRECTION('center_axis',(0.,0.,-1.));
#30012=DIRECTION('ref_axis',(1.,0.,0.));
#30013=DIRECTION('center_axis',(0.,0.,1.));
#30014=DIRECTION('ref_axis',(1.,0.,0.));
#30015=DIRECTION('center_axis',(0.,0.,1.));
#30016=DIRECTION('ref_axis',(1.,0.,0.));
#30017=DIRECTION('',(0.707106781186555,8.65956056235503E-17,-0.70710678118654));
#30018=DIRECTION('center_axis',(0.,0.,1.));
#30019=DIRECTION('ref_axis',(1.,0.,0.));
#30020=DIRECTION('center_axis',(0.,0.,-1.));
#30021=DIRECTION('ref_axis',(-1.,0.,0.));
#30022=DIRECTION('center_axis',(0.,0.,1.));
#30023=DIRECTION('ref_axis',(1.,0.,0.));
#30024=DIRECTION('center_axis',(0.,0.,1.));
#30025=DIRECTION('ref_axis',(1.,0.,0.));
#30026=DIRECTION('center_axis',(0.,0.,-1.));
#30027=DIRECTION('ref_axis',(1.,0.,0.));
#30028=DIRECTION('',(0.707106781186555,-8.65956056235502E-17,0.70710678118654));
#30029=DIRECTION('center_axis',(0.,0.,1.));
#30030=DIRECTION('ref_axis',(1.,0.,0.));
#30031=DIRECTION('center_axis',(0.,0.,1.));
#30032=DIRECTION('ref_axis',(1.,0.,0.));
#30033=DIRECTION('',(0.,0.,1.));
#30034=DIRECTION('center_axis',(0.,0.,-1.));
#30035=DIRECTION('ref_axis',(1.,0.,0.));
#30036=DIRECTION('center_axis',(0.,0.,1.));
#30037=DIRECTION('ref_axis',(1.,0.,0.));
#30038=DIRECTION('',(0.707106781186555,8.65956056235502E-17,-0.70710678118654));
#30039=DIRECTION('center_axis',(0.,0.,-1.));
#30040=DIRECTION('ref_axis',(1.,0.,0.));
#30041=DIRECTION('',(0.707106781186555,-8.65956056235502E-17,0.70710678118654));
#30042=DIRECTION('center_axis',(0.,0.,1.));
#30043=DIRECTION('ref_axis',(1.,0.,0.));
#30044=DIRECTION('center_axis',(0.,0.,1.));
#30045=DIRECTION('ref_axis',(1.,0.,0.));
#30046=DIRECTION('',(0.,0.,1.));
#30047=DIRECTION('center_axis',(0.,0.,-1.));
#30048=DIRECTION('ref_axis',(1.,0.,0.));
#30049=DIRECTION('center_axis',(0.,0.,1.));
#30050=DIRECTION('ref_axis',(1.,0.,0.));
#30051=DIRECTION('',(0.707106781186555,8.65956056235502E-17,-0.70710678118654));
#30052=DIRECTION('center_axis',(-1.,0.,0.));
#30053=DIRECTION('ref_axis',(0.,0.,1.));
#30054=DIRECTION('center_axis',(-1.,0.,0.));
#30055=DIRECTION('ref_axis',(0.,0.,1.));
#30056=DIRECTION('center_axis',(0.,0.,-1.));
#30057=DIRECTION('ref_axis',(-1.,0.,0.));
#30058=DIRECTION('',(0.707106781186555,8.65956056235503E-17,-0.70710678118654));
#30059=DIRECTION('center_axis',(0.,0.,1.));
#30060=DIRECTION('ref_axis',(-1.,0.,0.));
#30061=DIRECTION('center_axis',(0.,0.,1.));
#30062=DIRECTION('ref_axis',(-1.,0.,0.));
#30063=DIRECTION('center_axis',(0.,0.,1.));
#30064=DIRECTION('ref_axis',(1.,0.,0.));
#30065=DIRECTION('',(0.,0.,-1.));
#30066=DIRECTION('center_axis',(0.,0.,-1.));
#30067=DIRECTION('ref_axis',(-1.,0.,0.));
#30068=DIRECTION('center_axis',(0.,0.,-1.));
#30069=DIRECTION('ref_axis',(-1.,0.,0.));
#30070=DIRECTION('center_axis',(0.,0.,1.));
#30071=DIRECTION('ref_axis',(-1.,0.,0.));
#30072=DIRECTION('',(-0.707106781186555,-8.65956056235503E-17,-0.70710678118654));
#30073=DIRECTION('axis',(0.,0.,1.));
#30074=DIRECTION('refdir',(1.,0.,0.));
#30075=DIRECTION('center_axis',(0.,0.,-1.));
#30076=DIRECTION('ref_axis',(-1.,0.,0.));
#30077=DIRECTION('center_axis',(0.,0.,-1.));
#30078=DIRECTION('ref_axis',(-1.,0.,0.));
#30079=DIRECTION('',(-0.707106781186555,8.65956056235503E-17,0.70710678118654));
#30080=DIRECTION('center_axis',(0.,0.,1.));
#30081=DIRECTION('ref_axis',(-1.,0.,0.));
#30082=DIRECTION('center_axis',(0.,0.,1.));
#30083=DIRECTION('ref_axis',(-1.,0.,0.));
#30084=DIRECTION('center_axis',(0.,0.,1.));
#30085=DIRECTION('ref_axis',(1.,0.,0.));
#30086=DIRECTION('center_axis',(0.,0.,-1.));
#30087=DIRECTION('ref_axis',(-1.,0.,0.));
#30088=DIRECTION('center_axis',(0.,0.,-1.));
#30089=DIRECTION('ref_axis',(-1.,0.,0.));
#30090=DIRECTION('',(0.,0.,-1.));
#30091=DIRECTION('center_axis',(0.,0.,-1.));
#30092=DIRECTION('ref_axis',(-1.,0.,0.));
#30093=DIRECTION('center_axis',(0.,0.,-1.));
#30094=DIRECTION('ref_axis',(1.,0.,0.));
#30095=DIRECTION('center_axis',(0.,0.,1.));
#30096=DIRECTION('ref_axis',(-1.,0.,0.));
#30097=DIRECTION('center_axis',(0.,0.,-1.));
#30098=DIRECTION('ref_axis',(1.,0.,0.));
#30099=DIRECTION('center_axis',(0.,0.,-1.));
#30100=DIRECTION('ref_axis',(1.,0.,0.));
#30101=DIRECTION('center_axis',(0.,0.,1.));
#30102=DIRECTION('ref_axis',(-1.,0.,0.));
#30103=DIRECTION('center_axis',(0.,0.,-1.));
#30104=DIRECTION('ref_axis',(1.,0.,0.));
#30105=DIRECTION('center_axis',(0.,0.,-1.));
#30106=DIRECTION('ref_axis',(1.,0.,0.));
#30107=DIRECTION('center_axis',(0.,0.,1.));
#30108=DIRECTION('ref_axis',(-1.,0.,0.));
#30109=DIRECTION('center_axis',(0.,0.,-1.));
#30110=DIRECTION('ref_axis',(1.,0.,0.));
#30111=DIRECTION('center_axis',(0.,0.,1.));
#30112=DIRECTION('ref_axis',(-1.,0.,0.));
#30113=DIRECTION('',(0.707106781186555,-8.65956056235503E-17,0.70710678118654));
#30114=DIRECTION('center_axis',(0.,0.,1.));
#30115=DIRECTION('ref_axis',(-1.,0.,0.));
#30116=DIRECTION('center_axis',(0.,0.,1.));
#30117=DIRECTION('ref_axis',(1.,0.,0.));
#30118=DIRECTION('center_axis',(0.,0.,-1.));
#30119=DIRECTION('ref_axis',(-1.,0.,0.));
#30120=DIRECTION('center_axis',(0.,0.,1.));
#30121=DIRECTION('ref_axis',(1.,0.,0.));
#30122=DIRECTION('center_axis',(0.,0.,1.));
#30123=DIRECTION('ref_axis',(1.,0.,0.));
#30124=DIRECTION('center_axis',(0.,0.,1.));
#30125=DIRECTION('ref_axis',(1.,0.,0.));
#30126=DIRECTION('center_axis',(0.,0.,1.));
#30127=DIRECTION('ref_axis',(-1.,0.,0.));
#30128=DIRECTION('center_axis',(0.,0.,-1.));
#30129=DIRECTION('ref_axis',(-1.,0.,0.));
#30130=DIRECTION('center_axis',(0.,0.,-1.));
#30131=DIRECTION('ref_axis',(-1.,0.,0.));
#30132=DIRECTION('',(-0.707106781186555,-8.65956056235503E-17,-0.70710678118654));
#30133=DIRECTION('center_axis',(0.,0.,1.));
#30134=DIRECTION('ref_axis',(1.,0.,0.));
#30135=DIRECTION('center_axis',(0.,0.,1.));
#30136=DIRECTION('ref_axis',(-1.,0.,0.));
#30137=DIRECTION('center_axis',(0.,0.,1.));
#30138=DIRECTION('ref_axis',(-1.,0.,0.));
#30139=DIRECTION('',(0.,0.,-1.));
#30140=DIRECTION('center_axis',(0.,0.,-1.));
#30141=DIRECTION('ref_axis',(1.,0.,0.));
#30142=DIRECTION('',(0.707106781186555,-8.65956056235503E-17,0.70710678118654));
#30143=DIRECTION('center_axis',(0.,0.,1.));
#30144=DIRECTION('ref_axis',(1.,0.,0.));
#30145=DIRECTION('center_axis',(0.,0.,1.));
#30146=DIRECTION('ref_axis',(1.,0.,0.));
#30147=DIRECTION('',(0.,0.,1.));
#30148=DIRECTION('center_axis',(0.,0.,-1.));
#30149=DIRECTION('ref_axis',(1.,0.,0.));
#30150=DIRECTION('center_axis',(0.,0.,1.));
#30151=DIRECTION('ref_axis',(1.,0.,0.));
#30152=DIRECTION('',(0.707106781186555,8.65956056235503E-17,-0.70710678118654));
#30153=DIRECTION('center_axis',(0.,0.,-1.));
#30154=DIRECTION('ref_axis',(1.,0.,0.));
#30155=DIRECTION('',(0.707106781186555,-8.65956056235503E-17,0.70710678118654));
#30156=DIRECTION('center_axis',(0.,0.,1.));
#30157=DIRECTION('ref_axis',(1.,0.,0.));
#30158=DIRECTION('center_axis',(0.,0.,1.));
#30159=DIRECTION('ref_axis',(1.,0.,0.));
#30160=DIRECTION('',(0.,0.,1.));
#30161=DIRECTION('center_axis',(0.,0.,-1.));
#30162=DIRECTION('ref_axis',(1.,0.,0.));
#30163=DIRECTION('center_axis',(0.,0.,1.));
#30164=DIRECTION('ref_axis',(1.,0.,0.));
#30165=DIRECTION('',(0.707106781186555,8.65956056235503E-17,-0.70710678118654));
#30166=DIRECTION('center_axis',(0.,0.,-1.));
#30167=DIRECTION('ref_axis',(1.,0.,0.));
#30168=DIRECTION('',(0.707106781186555,-8.65956056235503E-17,0.70710678118654));
#30169=DIRECTION('center_axis',(0.,0.,1.));
#30170=DIRECTION('ref_axis',(1.,0.,0.));
#30171=DIRECTION('center_axis',(0.,0.,1.));
#30172=DIRECTION('ref_axis',(1.,0.,0.));
#30173=DIRECTION('',(0.,0.,1.));
#30174=DIRECTION('center_axis',(0.,0.,-1.));
#30175=DIRECTION('ref_axis',(1.,0.,0.));
#30176=DIRECTION('center_axis',(0.,0.,1.));
#30177=DIRECTION('ref_axis',(1.,0.,0.));
#30178=DIRECTION('',(0.707106781186555,8.65956056235503E-17,-0.70710678118654));
#30179=DIRECTION('center_axis',(0.,0.,-1.));
#30180=DIRECTION('ref_axis',(-1.,0.,0.));
#30181=DIRECTION('',(0.707106781186555,8.65956056235503E-17,-0.70710678118654));
#30182=DIRECTION('axis',(0.,0.,1.));
#30183=DIRECTION('refdir',(1.,0.,0.));
#30184=DIRECTION('center_axis',(0.,1.,0.));
#30185=DIRECTION('ref_axis',(-1.,0.,0.));
#30186=DIRECTION('',(0.,0.,-1.));
#30187=DIRECTION('',(1.,0.,0.));
#30188=DIRECTION('',(0.,0.,1.));
#30189=DIRECTION('',(-1.,0.,0.));
#30190=DIRECTION('center_axis',(0.,-1.,0.));
#30191=DIRECTION('ref_axis',(1.,0.,0.));
#30192=DIRECTION('',(0.,0.,1.));
#30193=DIRECTION('',(1.,0.,0.));
#30194=DIRECTION('',(0.,0.,1.));
#30195=DIRECTION('',(-1.,0.,0.));
#30196=DIRECTION('center_axis',(-1.,0.,0.));
#30197=DIRECTION('ref_axis',(0.,-1.,0.));
#30198=DIRECTION('',(0.,-1.,0.));
#30199=DIRECTION('',(0.,1.,0.));
#30200=DIRECTION('center_axis',(0.,0.,-1.));
#30201=DIRECTION('ref_axis',(-1.,0.,0.));
#30202=DIRECTION('center_axis',(0.,0.,1.));
#30203=DIRECTION('ref_axis',(1.,0.,0.));
#30204=DIRECTION('center_axis',(0.,0.,1.));
#30205=DIRECTION('ref_axis',(-1.,0.,0.));
#30206=DIRECTION('center_axis',(0.,0.,1.));
#30207=DIRECTION('ref_axis',(-1.,0.,0.));
#30208=DIRECTION('center_axis',(0.,0.,1.));
#30209=DIRECTION('ref_axis',(1.,0.,0.));
#30210=DIRECTION('',(1.,0.,0.));
#30211=DIRECTION('center_axis',(0.,0.,1.));
#30212=DIRECTION('ref_axis',(1.,2.06553120860494E-16,0.));
#30213=DIRECTION('',(-0.866025403784439,-0.5,0.));
#30214=DIRECTION('center_axis',(0.,0.,-1.));
#30215=DIRECTION('ref_axis',(1.,8.07434927000111E-16,0.));
#30216=DIRECTION('',(0.5,0.866025403784439,0.));
#30217=DIRECTION('center_axis',(0.,0.,1.));
#30218=DIRECTION('ref_axis',(0.5,0.866025403784439,0.));
#30219=DIRECTION('',(-2.77555756156289E-16,-1.,0.));
#30220=DIRECTION('center_axis',(0.,0.,-1.));
#30221=DIRECTION('ref_axis',(0.499999999999999,0.866025403784439,0.));
#30222=DIRECTION('',(-0.5,0.866025403784439,0.));
#30223=DIRECTION('center_axis',(0.,0.,1.));
#30224=DIRECTION('ref_axis',(-0.5,0.866025403784439,0.));
#30225=DIRECTION('',(0.866025403784438,-0.5,0.));
#30226=DIRECTION('center_axis',(0.,0.,-1.));
#30227=DIRECTION('ref_axis',(-0.500000000000001,0.866025403784438,0.));
#30228=DIRECTION('',(-1.,1.66533453693773E-16,0.));
#30229=DIRECTION('center_axis',(0.,0.,1.));
#30230=DIRECTION('ref_axis',(-1.,-5.16382802151235E-17,0.));
#30231=DIRECTION('',(0.866025403784439,0.5,0.));
#30232=DIRECTION('center_axis',(0.,0.,-1.));
#30233=DIRECTION('ref_axis',(-1.,-6.5604087818759E-16,0.));
#30234=DIRECTION('',(-0.5,-0.866025403784438,0.));
#30235=DIRECTION('center_axis',(0.,0.,1.));
#30236=DIRECTION('ref_axis',(-0.5,-0.866025403784438,0.));
#30237=DIRECTION('',(6.66133814775094E-16,1.,0.));
#30238=DIRECTION('center_axis',(0.,0.,-1.));
#30239=DIRECTION('ref_axis',(-0.5,-0.866025403784439,0.));
#30240=DIRECTION('',(0.499999999999999,-0.866025403784439,0.));
#30241=DIRECTION('center_axis',(0.,0.,1.));
#30242=DIRECTION('ref_axis',(0.5,-0.866025403784439,0.));
#30243=DIRECTION('',(-0.866025403784438,0.500000000000001,0.));
#30244=DIRECTION('center_axis',(0.,0.,-1.));
#30245=DIRECTION('ref_axis',(0.5,-0.866025403784439,0.));
#30246=DIRECTION('center_axis',(0.,0.,1.));
#30247=DIRECTION('ref_axis',(-1.,0.,0.));
#30248=DIRECTION('center_axis',(0.,0.,1.));
#30249=DIRECTION('ref_axis',(-1.,1.22464679914735E-16,0.));
#30250=DIRECTION('center_axis',(0.,0.,1.));
#30251=DIRECTION('ref_axis',(1.,0.,0.));
#30252=DIRECTION('center_axis',(0.,0.,-1.));
#30253=DIRECTION('ref_axis',(-1.,0.,0.));
#30254=DIRECTION('center_axis',(0.,0.,-1.));
#30255=DIRECTION('ref_axis',(-1.,0.,0.));
#30256=DIRECTION('',(0.,0.,-1.));
#30257=DIRECTION('center_axis',(0.,0.,-1.));
#30258=DIRECTION('ref_axis',(-1.,0.,0.));
#30259=DIRECTION('center_axis',(0.,0.,-1.));
#30260=DIRECTION('ref_axis',(-1.,0.,0.));
#30261=DIRECTION('',(0.,0.,-1.));
#30262=DIRECTION('center_axis',(0.,0.,-1.));
#30263=DIRECTION('ref_axis',(-1.,0.,0.));
#30264=DIRECTION('center_axis',(0.,0.,-1.));
#30265=DIRECTION('ref_axis',(-1.,0.,0.));
#30266=DIRECTION('',(0.,0.,-1.));
#30267=DIRECTION('center_axis',(-0.866025403784439,-0.499999999999999,0.));
#30268=DIRECTION('ref_axis',(0.499999999999999,-0.866025403784439,0.));
#30269=DIRECTION('',(0.,0.,1.));
#30270=DIRECTION('',(-0.499999999999999,0.866025403784439,0.));
#30271=DIRECTION('',(0.,0.,1.));
#30272=DIRECTION('center_axis',(0.,0.,1.));
#30273=DIRECTION('ref_axis',(0.5,-0.866025403784439,0.));
#30274=DIRECTION('',(0.,0.,1.));
#30275=DIRECTION('center_axis',(0.,0.,1.));
#30276=DIRECTION('ref_axis',(0.5,-0.866025403784439,0.));
#30277=DIRECTION('center_axis',(0.500000000000001,0.866025403784438,0.));
#30278=DIRECTION('ref_axis',(-0.866025403784438,0.500000000000001,0.));
#30279=DIRECTION('',(0.,0.,1.));
#30280=DIRECTION('',(0.866025403784438,-0.500000000000001,0.));
#30281=DIRECTION('center_axis',(0.,0.,1.));
#30282=DIRECTION('ref_axis',(0.5,-0.866025403784439,0.));
#30283=DIRECTION('center_axis',(0.,0.,-1.));
#30284=DIRECTION('ref_axis',(0.5,-0.866025403784439,0.));
#30285=DIRECTION('center_axis',(-0.866025403784438,0.5,0.));
#30286=DIRECTION('ref_axis',(-0.5,-0.866025403784438,0.));
#30287=DIRECTION('',(0.,0.,1.));
#30288=DIRECTION('',(0.5,0.866025403784438,0.));
#30289=DIRECTION('',(0.,0.,1.));
#30290=DIRECTION('center_axis',(0.,0.,1.));
#30291=DIRECTION('ref_axis',(-0.5,-0.866025403784439,0.));
#30292=DIRECTION('',(0.,0.,1.));
#30293=DIRECTION('center_axis',(0.,0.,1.));
#30294=DIRECTION('ref_axis',(-0.5,-0.866025403784439,0.));
#30295=DIRECTION('center_axis',(1.,-6.66133814775094E-16,0.));
#30296=DIRECTION('ref_axis',(6.66133814775094E-16,1.,0.));
#30297=DIRECTION('',(0.,0.,1.));
#30298=DIRECTION('',(-6.66133814775094E-16,-1.,0.));
#30299=DIRECTION('center_axis',(0.,0.,1.));
#30300=DIRECTION('ref_axis',(-0.5,-0.866025403784438,0.));
#30301=DIRECTION('center_axis',(0.,0.,-1.));
#30302=DIRECTION('ref_axis',(-0.5,-0.866025403784438,0.));
#30303=DIRECTION('center_axis',(1.66533453693773E-16,1.,0.));
#30304=DIRECTION('ref_axis',(-1.,1.66533453693773E-16,0.));
#30305=DIRECTION('',(0.,0.,1.));
#30306=DIRECTION('',(1.,-1.66533453693773E-16,0.));
#30307=DIRECTION('',(0.,0.,1.));
#30308=DIRECTION('center_axis',(0.,0.,1.));
#30309=DIRECTION('ref_axis',(-1.,-6.5604087818759E-16,0.));
#30310=DIRECTION('',(0.,0.,1.));
#30311=DIRECTION('center_axis',(0.,0.,1.));
#30312=DIRECTION('ref_axis',(-1.,-6.5604087818759E-16,0.));
#30313=DIRECTION('center_axis',(0.5,-0.866025403784439,0.));
#30314=DIRECTION('ref_axis',(0.866025403784439,0.5,0.));
#30315=DIRECTION('',(0.,0.,1.));
#30316=DIRECTION('',(-0.866025403784439,-0.5,0.));
#30317=DIRECTION('center_axis',(0.,0.,1.));
#30318=DIRECTION('ref_axis',(-1.,-5.16382802151235E-17,0.));
#30319=DIRECTION('center_axis',(0.,0.,-1.));
#30320=DIRECTION('ref_axis',(-1.,-5.16382802151235E-17,0.));
#30321=DIRECTION('center_axis',(0.866025403784439,0.5,0.));
#30322=DIRECTION('ref_axis',(-0.5,0.866025403784439,0.));
#30323=DIRECTION('',(0.,0.,1.));
#30324=DIRECTION('',(0.5,-0.866025403784439,0.));
#30325=DIRECTION('',(0.,0.,1.));
#30326=DIRECTION('center_axis',(0.,0.,1.));
#30327=DIRECTION('ref_axis',(-0.500000000000001,0.866025403784438,0.));
#30328=DIRECTION('',(0.,0.,1.));
#30329=DIRECTION('center_axis',(0.,0.,1.));
#30330=DIRECTION('ref_axis',(-0.500000000000001,0.866025403784438,0.));
#30331=DIRECTION('center_axis',(-0.5,-0.866025403784438,0.));
#30332=DIRECTION('ref_axis',(0.866025403784438,-0.5,0.));
#30333=DIRECTION('',(0.,0.,1.));
#30334=DIRECTION('',(-0.866025403784438,0.5,0.));
#30335=DIRECTION('center_axis',(0.,0.,1.));
#30336=DIRECTION('ref_axis',(-0.5,0.866025403784439,0.));
#30337=DIRECTION('center_axis',(0.,0.,-1.));
#30338=DIRECTION('ref_axis',(-0.5,0.866025403784439,0.));
#30339=DIRECTION('center_axis',(0.866025403784439,-0.5,0.));
#30340=DIRECTION('ref_axis',(0.5,0.866025403784439,0.));
#30341=DIRECTION('',(0.,0.,1.));
#30342=DIRECTION('',(-0.5,-0.866025403784439,0.));
#30343=DIRECTION('',(0.,0.,1.));
#30344=DIRECTION('center_axis',(0.,0.,1.));
#30345=DIRECTION('ref_axis',(0.499999999999999,0.866025403784439,0.));
#30346=DIRECTION('',(0.,0.,1.));
#30347=DIRECTION('center_axis',(0.,0.,1.));
#30348=DIRECTION('ref_axis',(0.499999999999999,0.866025403784439,0.));
#30349=DIRECTION('center_axis',(-1.,2.77555756156289E-16,0.));
#30350=DIRECTION('ref_axis',(-2.77555756156289E-16,-1.,0.));
#30351=DIRECTION('',(0.,0.,1.));
#30352=DIRECTION('',(2.77555756156289E-16,1.,0.));
#30353=DIRECTION('center_axis',(0.,0.,1.));
#30354=DIRECTION('ref_axis',(0.5,0.866025403784439,0.));
#30355=DIRECTION('center_axis',(0.,0.,-1.));
#30356=DIRECTION('ref_axis',(0.5,0.866025403784439,0.));
#30357=DIRECTION('center_axis',(0.,-1.,0.));
#30358=DIRECTION('ref_axis',(1.,0.,0.));
#30359=DIRECTION('',(0.,0.,1.));
#30360=DIRECTION('',(-1.,0.,0.));
#30361=DIRECTION('',(0.,0.,1.));
#30362=DIRECTION('center_axis',(0.,0.,1.));
#30363=DIRECTION('ref_axis',(1.,8.07434927000111E-16,0.));
#30364=DIRECTION('',(0.,0.,1.));
#30365=DIRECTION('center_axis',(0.,0.,1.));
#30366=DIRECTION('ref_axis',(1.,8.07434927000111E-16,0.));
#30367=DIRECTION('center_axis',(-0.5,0.866025403784439,0.));
#30368=DIRECTION('ref_axis',(-0.866025403784439,-0.5,0.));
#30369=DIRECTION('',(0.,0.,1.));
#30370=DIRECTION('',(0.866025403784439,0.5,0.));
#30371=DIRECTION('center_axis',(0.,0.,1.));
#30372=DIRECTION('ref_axis',(1.,2.06553120860494E-16,0.));
#30373=DIRECTION('center_axis',(0.,0.,-1.));
#30374=DIRECTION('ref_axis',(1.,2.06553120860494E-16,0.));
#30375=DIRECTION('center_axis',(0.,0.,1.));
#30376=DIRECTION('ref_axis',(1.,0.,0.));
#30377=DIRECTION('center_axis',(0.,0.,1.));
#30378=DIRECTION('ref_axis',(1.,0.,0.));
#30379=DIRECTION('',(0.,0.,-1.));
#30380=DIRECTION('center_axis',(0.,0.,1.));
#30381=DIRECTION('ref_axis',(1.,0.,0.));
#30382=DIRECTION('axis',(0.,0.,1.));
#30383=DIRECTION('refdir',(1.,0.,0.));
#30384=DIRECTION('center_axis',(-0.707106781186544,0.,-0.707106781186551));
#30385=DIRECTION('ref_axis',(-0.707106781186551,0.,0.707106781186544));
#30386=DIRECTION('',(-0.707106781186551,0.,0.707106781186544));
#30387=DIRECTION('',(0.,1.,0.));
#30388=DIRECTION('',(0.707106781186551,0.,-0.707106781186544));
#30389=DIRECTION('',(0.,-1.,0.));
#30390=DIRECTION('center_axis',(-1.,0.,0.));
#30391=DIRECTION('ref_axis',(0.,-1.,0.));
#30392=DIRECTION('',(0.,0.,1.));
#30393=DIRECTION('',(0.,-1.,0.));
#30394=DIRECTION('',(0.,0.,1.));
#30395=DIRECTION('center_axis',(0.,-1.,0.));
#30396=DIRECTION('ref_axis',(1.,0.,0.));
#30397=DIRECTION('',(1.,0.,0.));
#30398=DIRECTION('',(-0.707106781186548,0.,0.707106781186548));
#30399=DIRECTION('',(0.,0.,1.));
#30400=DIRECTION('',(0.707106781186548,0.,0.707106781186547));
#30401=DIRECTION('',(1.,0.,0.));
#30402=DIRECTION('',(0.707106781186548,0.,0.707106781186548));
#30403=DIRECTION('',(0.,0.,1.));
#30404=DIRECTION('',(-0.707106781186547,0.,0.707106781186548));
#30405=DIRECTION('',(1.,0.,0.));
#30406=DIRECTION('',(-0.707106781186548,0.,0.707106781186547));
#30407=DIRECTION('',(0.,0.,-1.));
#30408=DIRECTION('',(0.707106781186548,0.,0.707106781186547));
#30409=DIRECTION('',(-1.,0.,0.));
#30410=DIRECTION('',(0.707106781186548,0.,0.707106781186547));
#30411=DIRECTION('center_axis',(-0.707106781186548,0.,0.707106781186548));
#30412=DIRECTION('ref_axis',(0.707106781186548,0.,0.707106781186548));
#30413=DIRECTION('',(0.,1.,0.));
#30414=DIRECTION('',(-0.707106781186548,0.,-0.707106781186548));
#30415=DIRECTION('',(0.,-1.,0.));
#30416=DIRECTION('center_axis',(-1.,0.,0.));
#30417=DIRECTION('ref_axis',(0.,-1.,0.));
#30418=DIRECTION('',(0.,0.,1.));
#30419=DIRECTION('',(0.,1.,0.));
#30420=DIRECTION('center_axis',(0.,1.,0.));
#30421=DIRECTION('ref_axis',(-1.,0.,0.));
#30422=DIRECTION('',(-0.707106781186548,0.,-0.707106781186547));
#30423=DIRECTION('',(1.,0.,0.));
#30424=DIRECTION('',(-0.707106781186548,0.,-0.707106781186547));
#30425=DIRECTION('',(0.,0.,1.));
#30426=DIRECTION('',(0.707106781186548,0.,-0.707106781186547));
#30427=DIRECTION('',(-1.,0.,0.));
#30428=DIRECTION('',(0.707106781186547,0.,-0.707106781186548));
#30429=DIRECTION('',(-1.,0.,0.));
#30430=DIRECTION('',(-0.707106781186548,0.,-0.707106781186547));
#30431=DIRECTION('',(0.,0.,1.));
#30432=DIRECTION('',(0.707106781186548,0.,-0.707106781186548));
#30433=DIRECTION('',(-1.,0.,0.));
#30434=DIRECTION('center_axis',(-0.707106781186547,0.,0.707106781186548));
#30435=DIRECTION('ref_axis',(0.707106781186548,0.,0.707106781186547));
#30436=DIRECTION('',(0.,1.,0.));
#30437=DIRECTION('center_axis',(0.,0.,1.));
#30438=DIRECTION('ref_axis',(1.,0.,0.));
#30439=DIRECTION('',(0.,-1.,0.));
#30440=DIRECTION('',(1.,0.,0.));
#30441=DIRECTION('',(0.,-1.,0.));
#30442=DIRECTION('',(-1.,0.,0.));
#30443=DIRECTION('',(0.,1.,0.));
#30444=DIRECTION('center_axis',(-0.707106781186547,0.,0.707106781186548));
#30445=DIRECTION('ref_axis',(0.707106781186548,0.,0.707106781186547));
#30446=DIRECTION('',(0.,1.,0.));
#30447=DIRECTION('center_axis',(1.,0.,0.));
#30448=DIRECTION('ref_axis',(0.,1.,0.));
#30449=DIRECTION('',(0.,-1.,0.));
#30450=DIRECTION('center_axis',(-0.707106781186548,0.,-0.707106781186547));
#30451=DIRECTION('ref_axis',(-0.707106781186547,0.,0.707106781186548));
#30452=DIRECTION('',(0.,-1.,0.));
#30453=DIRECTION('center_axis',(0.,0.,1.));
#30454=DIRECTION('ref_axis',(1.,0.,0.));
#30455=DIRECTION('',(0.,1.,0.));
#30456=DIRECTION('',(-1.,0.,0.));
#30457=DIRECTION('',(0.,-1.,0.));
#30458=DIRECTION('',(1.,0.,0.));
#30459=DIRECTION('',(0.,1.,0.));
#30460=DIRECTION('center_axis',(-0.707106781186547,0.,-0.707106781186548));
#30461=DIRECTION('ref_axis',(-0.707106781186548,0.,0.707106781186547));
#30462=DIRECTION('center_axis',(-0.707106781186547,0.,0.707106781186548));
#30463=DIRECTION('ref_axis',(0.707106781186548,0.,0.707106781186547));
#30464=DIRECTION('',(0.,1.,0.));
#30465=DIRECTION('',(0.,-1.,0.));
#30466=DIRECTION('center_axis',(-1.,0.,0.));
#30467=DIRECTION('ref_axis',(0.,-1.,0.));
#30468=DIRECTION('',(0.,-1.,0.));
#30469=DIRECTION('',(0.,0.,1.));
#30470=DIRECTION('',(0.,-1.,0.));
#30471=DIRECTION('',(0.,0.,1.));
#30472=DIRECTION('center_axis',(1.,0.,0.));
#30473=DIRECTION('ref_axis',(0.,-1.,0.));
#30474=DIRECTION('center_axis',(1.,0.,0.));
#30475=DIRECTION('ref_axis',(0.,-1.,0.));
#30476=DIRECTION('',(0.,-1.,0.));
#30477=DIRECTION('center_axis',(-0.707106781186548,0.,-0.707106781186548));
#30478=DIRECTION('ref_axis',(-0.707106781186548,0.,0.707106781186548));
#30479=DIRECTION('',(0.,1.,0.));
#30480=DIRECTION('center_axis',(0.,0.,1.));
#30481=DIRECTION('ref_axis',(1.,0.,0.));
#30482=DIRECTION('center_axis',(-1.,0.,0.));
#30483=DIRECTION('ref_axis',(0.,-1.,0.));
#30484=DIRECTION('center_axis',(-1.,0.,0.));
#30485=DIRECTION('ref_axis',(0.,-1.,0.));
#30486=DIRECTION('',(-1.,0.,0.));
#30487=DIRECTION('center_axis',(-1.,0.,0.));
#30488=DIRECTION('ref_axis',(0.,-1.,0.));
#30489=DIRECTION('center_axis',(-1.,0.,0.));
#30490=DIRECTION('ref_axis',(0.,-1.,0.));
#30491=DIRECTION('',(-1.,0.,0.));
#30492=DIRECTION('center_axis',(0.,1.,0.));
#30493=DIRECTION('ref_axis',(-1.,0.,0.));
#30494=DIRECTION('',(-1.,0.,0.));
#30495=DIRECTION('',(-1.,0.,0.));
#30496=DIRECTION('',(0.,0.,1.));
#30497=DIRECTION('center_axis',(1.,0.,0.));
#30498=DIRECTION('ref_axis',(0.,1.,0.));
#30499=DIRECTION('',(0.,1.,0.));
#30500=DIRECTION('',(0.,1.,0.));
#30501=DIRECTION('',(0.,0.,1.));
#30502=DIRECTION('center_axis',(0.,-1.,0.));
#30503=DIRECTION('ref_axis',(1.,0.,0.));
#30504=DIRECTION('',(1.,0.,0.));
#30505=DIRECTION('',(1.,0.,0.));
#30506=DIRECTION('center_axis',(0.,0.,1.));
#30507=DIRECTION('ref_axis',(1.,0.,0.));
#30508=DIRECTION('center_axis',(0.,0.,1.));
#30509=DIRECTION('ref_axis',(1.,0.,0.));
#30510=DIRECTION('center_axis',(0.,1.,0.));
#30511=DIRECTION('ref_axis',(-1.,0.,0.));
#30512=DIRECTION('',(-1.,0.,0.));
#30513=DIRECTION('',(0.,0.,1.));
#30514=DIRECTION('',(0.,0.,1.));
#30515=DIRECTION('center_axis',(1.,0.,0.));
#30516=DIRECTION('ref_axis',(0.,1.,0.));
#30517=DIRECTION('',(0.,1.,0.));
#30518=DIRECTION('',(0.,0.,1.));
#30519=DIRECTION('center_axis',(0.,-1.,0.));
#30520=DIRECTION('ref_axis',(1.,0.,0.));
#30521=DIRECTION('',(1.,0.,0.));
#30522=DIRECTION('',(0.,0.,1.));
#30523=DIRECTION('center_axis',(-1.,0.,0.));
#30524=DIRECTION('ref_axis',(0.,-1.,0.));
#30525=DIRECTION('',(0.,-1.,0.));
#30526=DIRECTION('center_axis',(0.,0.,1.));
#30527=DIRECTION('ref_axis',(1.,0.,0.));
#30528=DIRECTION('center_axis',(0.,1.,0.));
#30529=DIRECTION('ref_axis',(-1.,0.,0.));
#30530=DIRECTION('',(0.,0.,1.));
#30531=DIRECTION('',(-1.,0.,0.));
#30532=DIRECTION('',(0.,0.,1.));
#30533=DIRECTION('center_axis',(1.,0.,0.));
#30534=DIRECTION('ref_axis',(0.,1.,0.));
#30535=DIRECTION('',(0.,0.,1.));
#30536=DIRECTION('',(0.,1.,0.));
#30537=DIRECTION('center_axis',(0.,-1.,0.));
#30538=DIRECTION('ref_axis',(1.,0.,0.));
#30539=DIRECTION('',(0.,0.,1.));
#30540=DIRECTION('',(1.,0.,0.));
#30541=DIRECTION('center_axis',(-1.,0.,0.));
#30542=DIRECTION('ref_axis',(0.,-1.,0.));
#30543=DIRECTION('',(0.,-1.,0.));
#30544=DIRECTION('center_axis',(0.,0.,1.));
#30545=DIRECTION('ref_axis',(1.,0.,0.));
#30546=DIRECTION('center_axis',(0.,0.,1.));
#30547=DIRECTION('ref_axis',(1.,0.,0.));
#30548=DIRECTION('axis',(0.,0.,1.));
#30549=DIRECTION('refdir',(1.,0.,0.));
#30550=DIRECTION('center_axis',(0.,0.,1.));
#30551=DIRECTION('ref_axis',(0.707106781186546,-0.707106781186549,0.));
#30552=DIRECTION('center_axis',(0.,0.,-1.));
#30553=DIRECTION('ref_axis',(0.707106781186546,-0.707106781186549,0.));
#30554=DIRECTION('',(0.,0.,-1.));
#30555=DIRECTION('center_axis',(0.,0.,1.));
#30556=DIRECTION('ref_axis',(0.707106781186546,-0.707106781186549,0.));
#30557=DIRECTION('',(0.,0.,1.));
#30558=DIRECTION('center_axis',(0.,0.,1.));
#30559=DIRECTION('ref_axis',(1.,0.,0.));
#30560=DIRECTION('',(0.,1.,0.));
#30561=DIRECTION('center_axis',(0.,0.,-1.));
#30562=DIRECTION('ref_axis',(0.707106781186548,0.707106781186547,0.));
#30563=DIRECTION('',(-1.,0.,0.));
#30564=DIRECTION('',(0.,1.,0.));
#30565=DIRECTION('center_axis',(0.,0.,-1.));
#30566=DIRECTION('ref_axis',(0.,1.,0.));
#30567=DIRECTION('',(1.,0.,0.));
#30568=DIRECTION('center_axis',(0.,0.,-1.));
#30569=DIRECTION('ref_axis',(-3.0626842058625E-15,-1.,0.));
#30570=DIRECTION('',(-1.,0.,0.));
#30571=DIRECTION('center_axis',(0.,0.,-1.));
#30572=DIRECTION('ref_axis',(0.,1.,0.));
#30573=DIRECTION('',(0.,1.,0.));
#30574=DIRECTION('',(1.,0.,0.));
#30575=DIRECTION('center_axis',(1.,0.,0.));
#30576=DIRECTION('ref_axis',(0.,1.,0.));
#30577=DIRECTION('',(0.,1.,0.));
#30578=DIRECTION('',(0.,0.,-1.));
#30579=DIRECTION('center_axis',(0.,0.,1.));
#30580=DIRECTION('ref_axis',(0.707106781186548,0.707106781186547,0.));
#30581=DIRECTION('center_axis',(0.,0.,1.));
#30582=DIRECTION('ref_axis',(0.707106781186548,0.707106781186547,0.));
#30583=DIRECTION('',(0.,0.,1.));
#30584=DIRECTION('center_axis',(-1.,0.,0.));
#30585=DIRECTION('ref_axis',(0.,-1.,0.));
#30586=DIRECTION('center_axis',(-1.,0.,0.));
#30587=DIRECTION('ref_axis',(0.,-1.,0.));
#30588=DIRECTION('',(-1.,0.,0.));
#30589=DIRECTION('center_axis',(1.,0.,0.));
#30590=DIRECTION('ref_axis',(0.,-1.,0.));
#30591=DIRECTION('center_axis',(-1.,0.,0.));
#30592=DIRECTION('ref_axis',(0.,-1.,0.));
#30593=DIRECTION('center_axis',(-1.,0.,0.));
#30594=DIRECTION('ref_axis',(0.,-1.,0.));
#30595=DIRECTION('',(-1.,0.,0.));
#30596=DIRECTION('center_axis',(1.,0.,0.));
#30597=DIRECTION('ref_axis',(0.,-1.,0.));
#30598=DIRECTION('center_axis',(0.,-1.,0.));
#30599=DIRECTION('ref_axis',(-1.,0.,0.));
#30600=DIRECTION('',(0.,0.,-1.));
#30601=DIRECTION('',(1.,0.,0.));
#30602=DIRECTION('',(0.,0.,-1.));
#30603=DIRECTION('center_axis',(0.,0.,-1.));
#30604=DIRECTION('ref_axis',(-3.0626842058625E-15,-1.,0.));
#30605=DIRECTION('',(0.,0.,-1.));
#30606=DIRECTION('center_axis',(0.,0.,1.));
#30607=DIRECTION('ref_axis',(-3.0626842058625E-15,-1.,0.));
#30608=DIRECTION('center_axis',(0.,1.,0.));
#30609=DIRECTION('ref_axis',(1.,0.,0.));
#30610=DIRECTION('',(0.,0.,-1.));
#30611=DIRECTION('',(-1.,0.,0.));
#30612=DIRECTION('center_axis',(0.,0.,-1.));
#30613=DIRECTION('ref_axis',(0.,1.,0.));
#30614=DIRECTION('center_axis',(0.,0.,1.));
#30615=DIRECTION('ref_axis',(0.,1.,0.));
#30616=DIRECTION('center_axis',(0.,0.,1.));
#30617=DIRECTION('ref_axis',(0.,1.,0.));
#30618=DIRECTION('center_axis',(0.,0.,1.));
#30619=DIRECTION('ref_axis',(1.,0.,0.));
#30620=DIRECTION('',(0.,1.,0.));
#30621=DIRECTION('center_axis',(0.,1.,0.));
#30622=DIRECTION('ref_axis',(-0.707106781186551,0.,-0.707106781186544));
#30623=DIRECTION('center_axis',(0.,-1.,0.));
#30624=DIRECTION('ref_axis',(-0.707106781186551,0.,-0.707106781186544));
#30625=DIRECTION('center_axis',(0.,1.,0.));
#30626=DIRECTION('ref_axis',(-0.707106781186551,0.,-0.707106781186544));
#30627=DIRECTION('',(0.,-1.,0.));
#30628=DIRECTION('center_axis',(0.,1.,0.));
#30629=DIRECTION('ref_axis',(-1.,0.,0.));
#30630=DIRECTION('',(-1.,0.,0.));
#30631=DIRECTION('',(0.,0.,-1.));
#30632=DIRECTION('center_axis',(0.,-1.,0.));
#30633=DIRECTION('ref_axis',(1.,0.,0.));
#30634=DIRECTION('',(0.,0.,1.));
#30635=DIRECTION('',(1.,0.,0.));
#30636=DIRECTION('center_axis',(0.,1.,0.));
#30637=DIRECTION('ref_axis',(-1.,0.,0.));
#30638=DIRECTION('',(-1.,0.,0.));
#30639=DIRECTION('',(0.,0.,1.));
#30640=DIRECTION('',(-1.,0.,0.));
#30641=DIRECTION('',(0.,0.,1.));
#30642=DIRECTION('center_axis',(1.,0.,0.));
#30643=DIRECTION('ref_axis',(0.,1.,0.));
#30644=DIRECTION('',(0.,1.,0.));
#30645=DIRECTION('',(0.,1.,0.));
#30646=DIRECTION('',(0.,0.,1.));
#30647=DIRECTION('',(0.,1.,0.));
#30648=DIRECTION('center_axis',(0.,-1.,0.));
#30649=DIRECTION('ref_axis',(1.,0.,0.));
#30650=DIRECTION('',(1.,0.,0.));
#30651=DIRECTION('',(1.,0.,0.));
#30652=DIRECTION('',(0.,0.,1.));
#30653=DIRECTION('center_axis',(-1.,0.,0.));
#30654=DIRECTION('ref_axis',(0.,-1.,0.));
#30655=DIRECTION('',(0.,-1.,0.));
#30656=DIRECTION('',(0.,-1.,0.));
#30657=DIRECTION('center_axis',(0.,0.,1.));
#30658=DIRECTION('ref_axis',(1.,0.,0.));
#30659=DIRECTION('center_axis',(0.,0.,1.));
#30660=DIRECTION('ref_axis',(1.,0.,0.));
#30661=DIRECTION('axis',(0.,0.,1.));
#30662=DIRECTION('refdir',(1.,0.,0.));
#30663=DIRECTION('center_axis',(0.,1.,0.));
#30664=DIRECTION('ref_axis',(-1.,0.,0.));
#30665=DIRECTION('',(1.,0.,0.));
#30666=DIRECTION('',(0.,0.,1.));
#30667=DIRECTION('',(-1.,0.,0.));
#30668=DIRECTION('',(0.,0.,1.));
#30669=DIRECTION('center_axis',(1.,0.,0.));
#30670=DIRECTION('ref_axis',(0.,1.,0.));
#30671=DIRECTION('',(0.,-1.,0.));
#30672=DIRECTION('',(0.,1.,0.));
#30673=DIRECTION('',(0.,0.,1.));
#30674=DIRECTION('center_axis',(0.,-1.,0.));
#30675=DIRECTION('ref_axis',(1.,0.,0.));
#30676=DIRECTION('',(-1.,0.,0.));
#30677=DIRECTION('',(1.,0.,0.));
#30678=DIRECTION('',(0.,0.,1.));
#30679=DIRECTION('center_axis',(-1.,0.,0.));
#30680=DIRECTION('ref_axis',(0.,-1.,0.));
#30681=DIRECTION('',(0.,1.,0.));
#30682=DIRECTION('',(0.,-1.,0.));
#30683=DIRECTION('center_axis',(0.,0.,1.));
#30684=DIRECTION('ref_axis',(1.,0.,0.));
#30685=DIRECTION('center_axis',(0.,1.,0.));
#30686=DIRECTION('ref_axis',(-1.,0.,0.));
#30687=DIRECTION('',(1.,0.,0.));
#30688=DIRECTION('',(0.,0.,1.));
#30689=DIRECTION('',(-1.,0.,0.));
#30690=DIRECTION('',(0.,0.,1.));
#30691=DIRECTION('center_axis',(1.,0.,0.));
#30692=DIRECTION('ref_axis',(0.,1.,0.));
#30693=DIRECTION('',(0.,-1.,0.));
#30694=DIRECTION('',(0.,1.,0.));
#30695=DIRECTION('',(0.,0.,1.));
#30696=DIRECTION('center_axis',(0.,-1.,0.));
#30697=DIRECTION('ref_axis',(1.,0.,0.));
#30698=DIRECTION('',(-1.,0.,0.));
#30699=DIRECTION('',(1.,0.,0.));
#30700=DIRECTION('',(0.,0.,1.));
#30701=DIRECTION('center_axis',(-1.,0.,0.));
#30702=DIRECTION('ref_axis',(0.,-1.,0.));
#30703=DIRECTION('',(0.,1.,0.));
#30704=DIRECTION('',(0.,-1.,0.));
#30705=DIRECTION('center_axis',(0.,0.,1.));
#30706=DIRECTION('ref_axis',(1.,0.,0.));
#30707=DIRECTION('center_axis',(0.,0.,1.));
#30708=DIRECTION('ref_axis',(1.,0.,0.));
#30709=DIRECTION('center_axis',(0.,0.,1.));
#30710=DIRECTION('ref_axis',(1.,0.,0.));
#30711=DIRECTION('',(0.,0.,-1.));
#30712=DIRECTION('center_axis',(0.,0.,-1.));
#30713=DIRECTION('ref_axis',(1.,0.,0.));
#30714=DIRECTION('center_axis',(0.,0.,1.));
#30715=DIRECTION('ref_axis',(1.,0.,0.));
#30716=DIRECTION('center_axis',(0.,1.,0.));
#30717=DIRECTION('ref_axis',(-1.,0.,0.));
#30718=DIRECTION('',(1.,0.,0.));
#30719=DIRECTION('',(0.,0.,1.));
#30720=DIRECTION('',(-1.,0.,0.));
#30721=DIRECTION('',(0.,0.,1.));
#30722=DIRECTION('center_axis',(1.,0.,0.));
#30723=DIRECTION('ref_axis',(0.,1.,0.));
#30724=DIRECTION('',(0.,-1.,0.));
#30725=DIRECTION('',(0.,1.,0.));
#30726=DIRECTION('',(0.,0.,1.));
#30727=DIRECTION('center_axis',(0.,-1.,0.));
#30728=DIRECTION('ref_axis',(1.,0.,0.));
#30729=DIRECTION('',(-1.,0.,0.));
#30730=DIRECTION('',(1.,0.,0.));
#30731=DIRECTION('',(0.,0.,1.));
#30732=DIRECTION('center_axis',(-1.,0.,0.));
#30733=DIRECTION('ref_axis',(0.,-1.,0.));
#30734=DIRECTION('',(0.,1.,0.));
#30735=DIRECTION('',(0.,-1.,0.));
#30736=DIRECTION('center_axis',(0.,0.,1.));
#30737=DIRECTION('ref_axis',(1.,0.,0.));
#30738=DIRECTION('center_axis',(0.,1.,0.));
#30739=DIRECTION('ref_axis',(-1.,0.,0.));
#30740=DIRECTION('',(1.,0.,0.));
#30741=DIRECTION('',(0.,0.,1.));
#30742=DIRECTION('',(-1.,0.,0.));
#30743=DIRECTION('',(0.,0.,1.));
#30744=DIRECTION('center_axis',(1.,0.,0.));
#30745=DIRECTION('ref_axis',(0.,1.,0.));
#30746=DIRECTION('',(0.,-1.,0.));
#30747=DIRECTION('',(0.,1.,0.));
#30748=DIRECTION('',(0.,0.,1.));
#30749=DIRECTION('center_axis',(0.,-1.,0.));
#30750=DIRECTION('ref_axis',(1.,0.,0.));
#30751=DIRECTION('',(-1.,0.,0.));
#30752=DIRECTION('',(1.,0.,0.));
#30753=DIRECTION('',(0.,0.,1.));
#30754=DIRECTION('center_axis',(-1.,0.,0.));
#30755=DIRECTION('ref_axis',(0.,-1.,0.));
#30756=DIRECTION('',(0.,1.,0.));
#30757=DIRECTION('',(0.,-1.,0.));
#30758=DIRECTION('center_axis',(0.,0.,1.));
#30759=DIRECTION('ref_axis',(1.,0.,0.));
#30760=DIRECTION('center_axis',(0.,1.,0.));
#30761=DIRECTION('ref_axis',(-1.,0.,0.));
#30762=DIRECTION('',(1.,0.,0.));
#30763=DIRECTION('',(0.,0.,1.));
#30764=DIRECTION('',(-1.,0.,0.));
#30765=DIRECTION('',(0.,0.,1.));
#30766=DIRECTION('center_axis',(1.,0.,0.));
#30767=DIRECTION('ref_axis',(0.,1.,0.));
#30768=DIRECTION('',(0.,-1.,0.));
#30769=DIRECTION('',(0.,1.,0.));
#30770=DIRECTION('',(0.,0.,1.));
#30771=DIRECTION('center_axis',(0.,-1.,0.));
#30772=DIRECTION('ref_axis',(1.,0.,0.));
#30773=DIRECTION('',(-1.,0.,0.));
#30774=DIRECTION('',(1.,0.,0.));
#30775=DIRECTION('',(0.,0.,1.));
#30776=DIRECTION('center_axis',(-1.,0.,0.));
#30777=DIRECTION('ref_axis',(0.,-1.,0.));
#30778=DIRECTION('',(0.,1.,0.));
#30779=DIRECTION('',(0.,-1.,0.));
#30780=DIRECTION('center_axis',(0.,0.,1.));
#30781=DIRECTION('ref_axis',(1.,0.,0.));
#30782=DIRECTION('center_axis',(0.,1.,0.));
#30783=DIRECTION('ref_axis',(-1.,0.,0.));
#30784=DIRECTION('',(1.,0.,0.));
#30785=DIRECTION('',(0.,0.,1.));
#30786=DIRECTION('',(-1.,0.,0.));
#30787=DIRECTION('',(0.,0.,1.));
#30788=DIRECTION('center_axis',(1.,0.,0.));
#30789=DIRECTION('ref_axis',(0.,1.,0.));
#30790=DIRECTION('',(0.,-1.,0.));
#30791=DIRECTION('',(0.,1.,0.));
#30792=DIRECTION('',(0.,0.,1.));
#30793=DIRECTION('center_axis',(0.,-1.,0.));
#30794=DIRECTION('ref_axis',(1.,0.,0.));
#30795=DIRECTION('',(-1.,0.,0.));
#30796=DIRECTION('',(1.,0.,0.));
#30797=DIRECTION('',(0.,0.,1.));
#30798=DIRECTION('center_axis',(-1.,0.,0.));
#30799=DIRECTION('ref_axis',(0.,-1.,0.));
#30800=DIRECTION('',(0.,1.,0.));
#30801=DIRECTION('',(0.,-1.,0.));
#30802=DIRECTION('center_axis',(0.,0.,1.));
#30803=DIRECTION('ref_axis',(1.,0.,0.));
#30804=DIRECTION('center_axis',(0.,0.,1.));
#30805=DIRECTION('ref_axis',(1.,0.,0.));
#30806=DIRECTION('center_axis',(0.,0.,1.));
#30807=DIRECTION('ref_axis',(1.,0.,0.));
#30808=DIRECTION('',(0.,0.,1.));
#30809=DIRECTION('center_axis',(0.,0.,-1.));
#30810=DIRECTION('ref_axis',(1.,0.,0.));
#30811=DIRECTION('center_axis',(0.,0.,1.));
#30812=DIRECTION('ref_axis',(1.,0.,0.));
#30813=DIRECTION('center_axis',(0.,0.,1.));
#30814=DIRECTION('ref_axis',(1.,0.,0.));
#30815=DIRECTION('',(0.,0.,1.));
#30816=DIRECTION('center_axis',(0.,0.,-1.));
#30817=DIRECTION('ref_axis',(1.,0.,0.));
#30818=DIRECTION('center_axis',(0.,0.,1.));
#30819=DIRECTION('ref_axis',(1.,0.,0.));
#30820=DIRECTION('center_axis',(0.,0.,1.));
#30821=DIRECTION('ref_axis',(1.,0.,0.));
#30822=DIRECTION('',(0.,0.,1.));
#30823=DIRECTION('center_axis',(0.,0.,-1.));
#30824=DIRECTION('ref_axis',(1.,0.,0.));
#30825=DIRECTION('center_axis',(0.,0.,1.));
#30826=DIRECTION('ref_axis',(1.,0.,0.));
#30827=DIRECTION('center_axis',(0.,0.,1.));
#30828=DIRECTION('ref_axis',(1.,0.,0.));
#30829=DIRECTION('',(0.,0.,-1.));
#30830=DIRECTION('center_axis',(0.,0.,1.));
#30831=DIRECTION('ref_axis',(1.,0.,0.));
#30832=DIRECTION('center_axis',(0.,0.,-1.));
#30833=DIRECTION('ref_axis',(-1.,0.,0.));
#30834=DIRECTION('center_axis',(0.,0.,1.));
#30835=DIRECTION('ref_axis',(1.,0.,0.));
#30836=DIRECTION('center_axis',(0.,0.,1.));
#30837=DIRECTION('ref_axis',(1.,0.,0.));
#30838=DIRECTION('center_axis',(0.,0.,1.));
#30839=DIRECTION('ref_axis',(1.,0.,0.));
#30840=DIRECTION('',(0.,0.,-1.));
#30841=DIRECTION('center_axis',(0.,0.,1.));
#30842=DIRECTION('ref_axis',(1.,0.,0.));
#30843=DIRECTION('axis',(0.,0.,1.));
#30844=DIRECTION('refdir',(1.,0.,0.));
#30845=DIRECTION('center_axis',(0.,0.,1.));
#30846=DIRECTION('ref_axis',(1.,0.,0.));
#30847=DIRECTION('',(0.,0.,-1.));
#30848=DIRECTION('',(0.,0.,-1.));
#30849=DIRECTION('center_axis',(0.,0.,1.));
#30850=DIRECTION('ref_axis',(1.,0.,0.));
#30851=DIRECTION('center_axis',(0.,0.,-1.));
#30852=DIRECTION('ref_axis',(1.,0.,0.));
#30853=DIRECTION('center_axis',(0.,0.,1.));
#30854=DIRECTION('ref_axis',(1.,0.,0.));
#30855=DIRECTION('',(0.,0.,-1.));
#30856=DIRECTION('center_axis',(0.,0.,1.));
#30857=DIRECTION('ref_axis',(1.,0.,0.));
#30858=DIRECTION('',(0.,0.,-1.));
#30859=DIRECTION('center_axis',(0.,0.,1.));
#30860=DIRECTION('ref_axis',(1.,7.2918327227141E-15,9.38957226509774E-17));
#30861=DIRECTION('',(0.,0.,1.));
#30862=DIRECTION('center_axis',(0.,0.,1.));
#30863=DIRECTION('ref_axis',(1.,7.2918327227141E-15,9.38957226509774E-17));
#30864=DIRECTION('center_axis',(0.,0.,1.));
#30865=DIRECTION('ref_axis',(1.,7.2918327227141E-15,9.38957226509774E-17));
#30866=DIRECTION('',(0.,0.,1.));
#30867=DIRECTION('center_axis',(0.,0.,1.));
#30868=DIRECTION('ref_axis',(1.,7.2918327227141E-15,9.38957226509774E-17));
#30869=DIRECTION('',(0.,0.,1.));
#30870=DIRECTION('center_axis',(0.,0.,1.));
#30871=DIRECTION('ref_axis',(1.,7.2918327227141E-15,9.38957226509774E-17));
#30872=DIRECTION('',(0.,0.,1.));
#30873=DIRECTION('center_axis',(0.,0.,1.));
#30874=DIRECTION('ref_axis',(1.,0.,0.));
#30875=DIRECTION('center_axis',(0.,0.,-1.));
#30876=DIRECTION('ref_axis',(1.,0.,0.));
#30877=DIRECTION('center_axis',(0.,0.,-1.));
#30878=DIRECTION('ref_axis',(1.,0.,0.));
#30879=DIRECTION('center_axis',(0.,0.,1.));
#30880=DIRECTION('ref_axis',(1.,0.,0.));
#30881=DIRECTION('center_axis',(0.,0.,-1.));
#30882=DIRECTION('ref_axis',(1.,7.2918327227141E-15,9.38957226509774E-17));
#30883=DIRECTION('center_axis',(0.,0.,1.));
#30884=DIRECTION('ref_axis',(0.222268344484715,0.974985529656735,9.38957226509774E-17));
#30885=DIRECTION('center_axis',(0.,0.,1.));
#30886=DIRECTION('ref_axis',(0.890895128280542,-0.454209060242083,0.));
#30887=DIRECTION('center_axis',(0.,0.,-1.));
#30888=DIRECTION('ref_axis',(1.,0.,0.));
#30889=DIRECTION('center_axis',(0.,0.,1.));
#30890=DIRECTION('ref_axis',(1.,0.,0.));
#30891=DIRECTION('',(-0.838805152831226,-1.02724004552307E-16,0.544431736385548));
#30892=DIRECTION('center_axis',(0.,0.,-1.));
#30893=DIRECTION('ref_axis',(1.,0.,0.));
#30894=DIRECTION('center_axis',(0.5,0.866025403784439,0.));
#30895=DIRECTION('ref_axis',(0.866025403784439,-0.5,0.));
#30896=DIRECTION('',(0.866025403784439,-0.5,0.));
#30897=DIRECTION('',(0.,0.,-1.));
#30898=DIRECTION('',(0.866025403784439,-0.5,0.));
#30899=DIRECTION('',(0.,0.,-1.));
#30900=DIRECTION('center_axis',(-0.5,0.866025403784439,0.));
#30901=DIRECTION('ref_axis',(0.866025403784439,0.5,0.));
#30902=DIRECTION('',(0.866025403784439,0.5,0.));
#30903=DIRECTION('',(0.,0.,-1.));
#30904=DIRECTION('',(0.866025403784439,0.5,0.));
#30905=DIRECTION('center_axis',(-1.,-1.33539075443303E-16,0.));
#30906=DIRECTION('ref_axis',(-1.33539075443303E-16,1.,0.));
#30907=DIRECTION('',(-1.33539075443303E-16,1.,0.));
#30908=DIRECTION('',(0.,0.,-1.));
#30909=DIRECTION('',(-1.33539075443303E-16,1.,0.));
#30910=DIRECTION('center_axis',(-0.5,-0.866025403784439,0.));
#30911=DIRECTION('ref_axis',(-0.866025403784439,0.5,0.));
#30912=DIRECTION('',(-0.866025403784439,0.5,0.));
#30913=DIRECTION('',(0.,0.,-1.));
#30914=DIRECTION('',(-0.866025403784439,0.5,0.));
#30915=DIRECTION('center_axis',(0.5,-0.866025403784439,0.));
#30916=DIRECTION('ref_axis',(-0.866025403784439,-0.5,0.));
#30917=DIRECTION('',(-0.866025403784439,-0.5,0.));
#30918=DIRECTION('',(0.,0.,-1.));
#30919=DIRECTION('',(-0.866025403784439,-0.5,0.));
#30920=DIRECTION('center_axis',(1.,-2.67078150886606E-16,0.));
#30921=DIRECTION('ref_axis',(-2.67078150886606E-16,-1.,0.));
#30922=DIRECTION('',(-2.67078150886606E-16,-1.,0.));
#30923=DIRECTION('',(-2.67078150886606E-16,-1.,0.));
#30924=DIRECTION('center_axis',(0.,0.,-1.));
#30925=DIRECTION('ref_axis',(-1.,0.,0.));
#30926=DIRECTION('center_axis',(0.,0.,-1.));
#30927=DIRECTION('ref_axis',(-1.,0.,0.));
#30928=DIRECTION('center_axis',(0.,0.,1.));
#30929=DIRECTION('ref_axis',(1.,0.,0.));
#30930=DIRECTION('center_axis',(0.,0.,1.));
#30931=DIRECTION('ref_axis',(1.,0.,0.));
#30932=DIRECTION('',(0.768221279597376,9.4079973109581E-17,-0.64018439966448));
#30933=DIRECTION('center_axis',(0.,0.,-1.));
#30934=DIRECTION('ref_axis',(1.,0.,0.));
#30935=DIRECTION('center_axis',(0.,0.,1.));
#30936=DIRECTION('ref_axis',(1.,0.,0.));
#30937=DIRECTION('',(-0.707106781186547,-8.65956056235493E-17,-0.707106781186548));
#30938=DIRECTION('center_axis',(0.,0.,1.));
#30939=DIRECTION('ref_axis',(1.,0.,0.));
#30940=DIRECTION('axis',(0.,0.,1.));
#30941=DIRECTION('refdir',(1.,0.,0.));
#30942=DIRECTION('center_axis',(0.,0.,1.));
#30943=DIRECTION('ref_axis',(1.,0.,0.));
#30944=DIRECTION('',(0.,0.,-1.));
#30945=DIRECTION('center_axis',(0.,0.,-1.));
#30946=DIRECTION('ref_axis',(1.,0.,0.));
#30947=DIRECTION('',(0.,0.,-1.));
#30948=DIRECTION('center_axis',(0.,0.,1.));
#30949=DIRECTION('ref_axis',(1.,0.,0.));
#30950=DIRECTION('center_axis',(0.,0.,-1.));
#30951=DIRECTION('ref_axis',(1.,0.,0.));
#30952=DIRECTION('center_axis',(0.,0.,1.));
#30953=DIRECTION('ref_axis',(1.,0.,0.));
#30954=DIRECTION('',(0.,0.,-1.));
#30955=DIRECTION('center_axis',(0.,0.,1.));
#30956=DIRECTION('ref_axis',(1.,0.,0.));
#30957=DIRECTION('',(0.,0.,-1.));
#30958=DIRECTION('center_axis',(0.,0.,1.));
#30959=DIRECTION('ref_axis',(1.,0.,0.));
#30960=DIRECTION('',(0.,0.,-1.));
#30961=DIRECTION('center_axis',(0.,0.,1.));
#30962=DIRECTION('ref_axis',(1.,0.,0.));
#30963=DIRECTION('',(0.,0.,-1.));
#30964=DIRECTION('center_axis',(0.,0.,1.));
#30965=DIRECTION('ref_axis',(1.,0.,0.));
#30966=DIRECTION('',(0.,0.,-1.));
#30967=DIRECTION('center_axis',(0.,0.,1.));
#30968=DIRECTION('ref_axis',(1.,0.,0.));
#30969=DIRECTION('',(0.,0.,-1.));
#30970=DIRECTION('center_axis',(0.,0.,1.));
#30971=DIRECTION('ref_axis',(1.,0.,0.));
#30972=DIRECTION('',(0.,0.,-1.));
#30973=DIRECTION('center_axis',(0.,0.,1.));
#30974=DIRECTION('ref_axis',(0.918748963007942,-0.394842174763325,0.));
#30975=DIRECTION('',(0.,0.,1.));
#30976=DIRECTION('center_axis',(0.,0.,1.));
#30977=DIRECTION('ref_axis',(1.,3.85997805270075E-14,0.));
#30978=DIRECTION('center_axis',(0.,0.,1.));
#30979=DIRECTION('ref_axis',(1.,3.85997805270075E-14,0.));
#30980=DIRECTION('',(0.,0.,1.));
#30981=DIRECTION('center_axis',(0.,0.,1.));
#30982=DIRECTION('ref_axis',(1.,3.85997805270075E-14,0.));
#30983=DIRECTION('',(0.,0.,1.));
#30984=DIRECTION('center_axis',(0.,0.,1.));
#30985=DIRECTION('ref_axis',(1.,3.85997805270075E-14,0.));
#30986=DIRECTION('',(0.,0.,1.));
#30987=DIRECTION('center_axis',(0.,0.,1.));
#30988=DIRECTION('ref_axis',(1.,3.85997805270075E-14,0.));
#30989=DIRECTION('',(0.,0.,1.));
#30990=DIRECTION('center_axis',(0.,0.,1.));
#30991=DIRECTION('ref_axis',(1.,3.85997805270075E-14,0.));
#30992=DIRECTION('',(0.,0.,1.));
#30993=DIRECTION('center_axis',(0.,0.,1.));
#30994=DIRECTION('ref_axis',(1.,3.85997805270075E-14,0.));
#30995=DIRECTION('',(0.,0.,1.));
#30996=DIRECTION('center_axis',(0.,0.,1.));
#30997=DIRECTION('ref_axis',(1.,3.85997805270075E-14,0.));
#30998=DIRECTION('',(0.,0.,1.));
#30999=DIRECTION('center_axis',(0.,0.,1.));
#31000=DIRECTION('ref_axis',(1.,0.,0.));
#31001=DIRECTION('center_axis',(0.,0.,-1.));
#31002=DIRECTION('ref_axis',(1.,3.85997805270075E-14,0.));
#31003=DIRECTION('center_axis',(0.,0.,1.));
#31004=DIRECTION('ref_axis',(-0.518977820445148,0.854787705741024,0.));
#31005=DIRECTION('center_axis',(0.,0.,1.));
#31006=DIRECTION('ref_axis',(1.,0.,0.));
#31007=DIRECTION('center_axis',(0.,0.,-1.));
#31008=DIRECTION('ref_axis',(1.,0.,0.));
#31009=DIRECTION('center_axis',(0.,0.,1.));
#31010=DIRECTION('ref_axis',(1.,0.,0.));
#31011=DIRECTION('',(-0.857167300702112,-1.04972719113862E-16,0.515038074910054));
#31012=DIRECTION('center_axis',(0.,0.,1.));
#31013=DIRECTION('ref_axis',(1.,0.,0.));
#31014=DIRECTION('center_axis',(0.,0.,1.));
#31015=DIRECTION('ref_axis',(1.,0.,0.));
#31016=DIRECTION('',(0.,0.,1.));
#31017=DIRECTION('center_axis',(0.,0.,1.));
#31018=DIRECTION('ref_axis',(1.,0.,0.));
#31019=DIRECTION('center_axis',(0.,0.,1.));
#31020=DIRECTION('ref_axis',(1.,0.,0.));
#31021=DIRECTION('',(-0.707106781186547,-8.65956056235493E-17,0.707106781186548));
#31022=DIRECTION('center_axis',(0.,0.,-1.));
#31023=DIRECTION('ref_axis',(1.,0.,0.));
#31024=DIRECTION('center_axis',(0.,0.,1.));
#31025=DIRECTION('ref_axis',(1.,0.,0.));
#31026=DIRECTION('center_axis',(0.,0.,-1.));
#31027=DIRECTION('ref_axis',(1.,0.,0.));
#31028=DIRECTION('center_axis',(0.,0.,1.));
#31029=DIRECTION('ref_axis',(1.,0.,0.));
#31030=DIRECTION('center_axis',(0.,0.,-1.));
#31031=DIRECTION('ref_axis',(1.,0.,0.));
#31032=DIRECTION('center_axis',(0.,0.,1.));
#31033=DIRECTION('ref_axis',(-1.,-1.22464679914735E-16,0.));
#31034=DIRECTION('center_axis',(0.,0.,-1.));
#31035=DIRECTION('ref_axis',(1.,0.,0.));
#31036=DIRECTION('center_axis',(0.,0.,1.));
#31037=DIRECTION('ref_axis',(1.,0.,0.));
#31038=DIRECTION('center_axis',(0.,0.,-1.));
#31039=DIRECTION('ref_axis',(1.,0.,0.));
#31040=DIRECTION('center_axis',(0.,0.,1.));
#31041=DIRECTION('ref_axis',(1.,0.,0.));
#31042=DIRECTION('center_axis',(0.,0.,-1.));
#31043=DIRECTION('ref_axis',(1.,0.,0.));
#31044=DIRECTION('center_axis',(0.,0.,1.));
#31045=DIRECTION('ref_axis',(1.,0.,0.));
#31046=DIRECTION('center_axis',(0.,0.,-1.));
#31047=DIRECTION('ref_axis',(1.,0.,0.));
#31048=DIRECTION('center_axis',(-1.92296268638356E-16,-1.,0.));
#31049=DIRECTION('ref_axis',(1.,-1.92296268638356E-16,0.));
#31050=DIRECTION('',(0.,0.,1.));
#31051=DIRECTION('',(1.,-1.92296268638356E-16,0.));
#31052=DIRECTION('',(0.,0.,1.));
#31053=DIRECTION('',(1.,-1.92296268638356E-16,0.));
#31054=DIRECTION('center_axis',(-0.866025403784439,-0.5,0.));
#31055=DIRECTION('ref_axis',(0.5,-0.866025403784439,0.));
#31056=DIRECTION('',(0.5,-0.866025403784439,0.));
#31057=DIRECTION('',(0.,0.,1.));
#31058=DIRECTION('',(0.5,-0.866025403784439,0.));
#31059=DIRECTION('center_axis',(-0.866025403784438,0.5,0.));
#31060=DIRECTION('ref_axis',(-0.5,-0.866025403784438,0.));
#31061=DIRECTION('',(-0.5,-0.866025403784438,0.));
#31062=DIRECTION('',(0.,0.,1.));
#31063=DIRECTION('',(-0.5,-0.866025403784438,0.));
#31064=DIRECTION('center_axis',(0.,0.,1.));
#31065=DIRECTION('ref_axis',(1.,0.,0.));
#31066=DIRECTION('',(0.5,0.866025403784439,0.));
#31067=DIRECTION('',(-1.,1.92296268638356E-16,0.));
#31068=DIRECTION('',(-0.5,0.866025403784439,0.));
#31069=DIRECTION('center_axis',(1.92296268638356E-16,1.,0.));
#31070=DIRECTION('ref_axis',(-1.,1.92296268638356E-16,0.));
#31071=DIRECTION('',(-1.,1.92296268638356E-16,0.));
#31072=DIRECTION('',(0.,0.,1.));
#31073=DIRECTION('center_axis',(0.,0.,-1.));
#31074=DIRECTION('ref_axis',(1.,0.,0.));
#31075=DIRECTION('center_axis',(0.,0.,1.));
#31076=DIRECTION('ref_axis',(1.,0.,0.));
#31077=DIRECTION('center_axis',(0.,0.,-1.));
#31078=DIRECTION('ref_axis',(1.,0.,0.));
#31079=DIRECTION('center_axis',(0.,0.,1.));
#31080=DIRECTION('ref_axis',(1.,0.,0.));
#31081=DIRECTION('center_axis',(0.,0.,-1.));
#31082=DIRECTION('ref_axis',(1.,0.,0.));
#31083=DIRECTION('center_axis',(0.,0.,1.));
#31084=DIRECTION('ref_axis',(1.,0.,0.));
#31085=DIRECTION('center_axis',(0.,0.,-1.));
#31086=DIRECTION('ref_axis',(-1.,-1.01064309961486E-15,0.));
#31087=DIRECTION('center_axis',(0.,0.,1.));
#31088=DIRECTION('ref_axis',(1.,0.,0.));
#31089=DIRECTION('center_axis',(0.,0.,-1.));
#31090=DIRECTION('ref_axis',(1.,0.,0.));
#31091=DIRECTION('center_axis',(0.,0.,1.));
#31092=DIRECTION('ref_axis',(1.,0.,0.));
#31093=DIRECTION('center_axis',(0.,0.,-1.));
#31094=DIRECTION('ref_axis',(1.,0.,0.));
#31095=DIRECTION('center_axis',(0.,0.,1.));
#31096=DIRECTION('ref_axis',(1.,0.,0.));
#31097=DIRECTION('center_axis',(0.866025403784439,-0.5,0.));
#31098=DIRECTION('ref_axis',(0.5,0.866025403784439,0.));
#31099=DIRECTION('',(0.,0.,1.));
#31100=DIRECTION('',(0.5,0.866025403784439,0.));
#31101=DIRECTION('center_axis',(0.,0.,-1.));
#31102=DIRECTION('ref_axis',(-1.,0.,0.));
#31103=DIRECTION('center_axis',(0.,0.,1.));
#31104=DIRECTION('ref_axis',(1.,0.,0.));
#31105=DIRECTION('center_axis',(0.,0.,1.));
#31106=DIRECTION('ref_axis',(1.,0.,0.));
#31107=DIRECTION('',(0.707106781186547,8.65956056235493E-17,-0.707106781186548));
#31108=DIRECTION('center_axis',(0.866025403784439,0.5,0.));
#31109=DIRECTION('ref_axis',(-0.5,0.866025403784439,0.));
#31110=DIRECTION('',(-0.5,0.866025403784439,0.));
#31111=DIRECTION('center_axis',(0.,0.,1.));
#31112=DIRECTION('ref_axis',(1.,0.,0.));
#31113=DIRECTION('axis',(0.,0.,1.));
#31114=DIRECTION('refdir',(1.,0.,0.));
#31115=DIRECTION('center_axis',(0.,0.,1.));
#31116=DIRECTION('ref_axis',(1.,0.,0.));
#31117=DIRECTION('',(0.,0.,-1.));
#31118=DIRECTION('center_axis',(0.,0.,-1.));
#31119=DIRECTION('ref_axis',(1.,0.,0.));
#31120=DIRECTION('',(0.,0.,-1.));
#31121=DIRECTION('center_axis',(0.,0.,1.));
#31122=DIRECTION('ref_axis',(1.,0.,0.));
#31123=DIRECTION('center_axis',(0.,0.,-1.));
#31124=DIRECTION('ref_axis',(1.,0.,0.));
#31125=DIRECTION('center_axis',(0.,0.,1.));
#31126=DIRECTION('ref_axis',(1.,0.,0.));
#31127=DIRECTION('',(0.,0.,-1.));
#31128=DIRECTION('center_axis',(0.,0.,1.));
#31129=DIRECTION('ref_axis',(1.,0.,0.));
#31130=DIRECTION('',(0.,0.,-1.));
#31131=DIRECTION('center_axis',(0.,0.,1.));
#31132=DIRECTION('ref_axis',(1.,0.,0.));
#31133=DIRECTION('',(0.,0.,-1.));
#31134=DIRECTION('center_axis',(0.,0.,1.));
#31135=DIRECTION('ref_axis',(1.,0.,0.));
#31136=DIRECTION('',(0.,0.,-1.));
#31137=DIRECTION('center_axis',(0.,0.,1.));
#31138=DIRECTION('ref_axis',(1.,0.,0.));
#31139=DIRECTION('',(0.,0.,-1.));
#31140=DIRECTION('center_axis',(0.,0.,1.));
#31141=DIRECTION('ref_axis',(1.,0.,0.));
#31142=DIRECTION('',(0.,0.,-1.));
#31143=DIRECTION('center_axis',(0.,0.,1.));
#31144=DIRECTION('ref_axis',(1.,0.,0.));
#31145=DIRECTION('',(0.,0.,-1.));
#31146=DIRECTION('center_axis',(0.,0.,1.));
#31147=DIRECTION('ref_axis',(1.,0.,0.));
#31148=DIRECTION('',(0.,0.,-1.));
#31149=DIRECTION('center_axis',(0.,0.,1.));
#31150=DIRECTION('ref_axis',(1.,0.,0.));
#31151=DIRECTION('',(0.,0.,-1.));
#31152=DIRECTION('center_axis',(0.,0.,1.));
#31153=DIRECTION('ref_axis',(1.,0.,0.));
#31154=DIRECTION('',(0.,0.,-1.));
#31155=DIRECTION('center_axis',(0.,0.,1.));
#31156=DIRECTION('ref_axis',(1.,0.,0.));
#31157=DIRECTION('',(0.,0.,-1.));
#31158=DIRECTION('center_axis',(0.,0.,1.));
#31159=DIRECTION('ref_axis',(1.,0.,0.));
#31160=DIRECTION('',(0.,0.,-1.));
#31161=DIRECTION('center_axis',(0.,0.,1.));
#31162=DIRECTION('ref_axis',(1.,0.,0.));
#31163=DIRECTION('',(0.,0.,-1.));
#31164=DIRECTION('center_axis',(0.,0.,1.));
#31165=DIRECTION('ref_axis',(1.,0.,0.));
#31166=DIRECTION('',(0.,0.,-1.));
#31167=DIRECTION('center_axis',(0.,0.,1.));
#31168=DIRECTION('ref_axis',(1.,0.,0.));
#31169=DIRECTION('',(0.,0.,-1.));
#31170=DIRECTION('center_axis',(0.,0.,1.));
#31171=DIRECTION('ref_axis',(1.,0.,0.));
#31172=DIRECTION('',(0.,0.,-1.));
#31173=DIRECTION('center_axis',(0.,0.,1.));
#31174=DIRECTION('ref_axis',(1.,0.,0.));
#31175=DIRECTION('',(0.,0.,-1.));
#31176=DIRECTION('center_axis',(0.,0.,1.));
#31177=DIRECTION('ref_axis',(1.,0.,0.));
#31178=DIRECTION('',(0.,0.,-1.));
#31179=DIRECTION('center_axis',(0.,0.,1.));
#31180=DIRECTION('ref_axis',(1.,0.,0.));
#31181=DIRECTION('',(0.,0.,-1.));
#31182=DIRECTION('center_axis',(0.,0.,1.));
#31183=DIRECTION('ref_axis',(1.,0.,0.));
#31184=DIRECTION('',(0.,0.,-1.));
#31185=DIRECTION('center_axis',(0.,0.,1.));
#31186=DIRECTION('ref_axis',(1.,0.,0.));
#31187=DIRECTION('',(0.,0.,-1.));
#31188=DIRECTION('center_axis',(0.,0.,1.));
#31189=DIRECTION('ref_axis',(1.,0.,0.));
#31190=DIRECTION('',(0.,0.,-1.));
#31191=DIRECTION('center_axis',(0.,0.,1.));
#31192=DIRECTION('ref_axis',(1.,0.,0.));
#31193=DIRECTION('',(0.,0.,-1.));
#31194=DIRECTION('center_axis',(0.,0.,1.));
#31195=DIRECTION('ref_axis',(1.,0.,0.));
#31196=DIRECTION('',(0.,0.,-1.));
#31197=DIRECTION('center_axis',(0.,0.,1.));
#31198=DIRECTION('ref_axis',(1.,0.,0.));
#31199=DIRECTION('',(0.,0.,-1.));
#31200=DIRECTION('center_axis',(0.,0.,1.));
#31201=DIRECTION('ref_axis',(1.,0.,0.));
#31202=DIRECTION('',(0.,0.,-1.));
#31203=DIRECTION('center_axis',(0.,0.,1.));
#31204=DIRECTION('ref_axis',(1.,0.,0.));
#31205=DIRECTION('',(0.,0.,-1.));
#31206=DIRECTION('center_axis',(0.,0.,1.));
#31207=DIRECTION('ref_axis',(-0.00388812637901143,-0.999992441208063,0.));
#31208=DIRECTION('',(0.,0.,1.));
#31209=DIRECTION('center_axis',(0.,0.,1.));
#31210=DIRECTION('ref_axis',(1.,-1.57698425990146E-13,0.));
#31211=DIRECTION('center_axis',(0.,0.,1.));
#31212=DIRECTION('ref_axis',(1.,-1.57698425990146E-13,0.));
#31213=DIRECTION('',(0.,0.,1.));
#31214=DIRECTION('center_axis',(0.,0.,1.));
#31215=DIRECTION('ref_axis',(1.,-1.57698425990146E-13,0.));
#31216=DIRECTION('',(0.,0.,1.));
#31217=DIRECTION('center_axis',(0.,0.,1.));
#31218=DIRECTION('ref_axis',(1.,-1.57698425990146E-13,0.));
#31219=DIRECTION('',(0.,0.,1.));
#31220=DIRECTION('center_axis',(0.,0.,1.));
#31221=DIRECTION('ref_axis',(1.,-1.57698425990146E-13,0.));
#31222=DIRECTION('',(0.,0.,1.));
#31223=DIRECTION('center_axis',(0.,0.,1.));
#31224=DIRECTION('ref_axis',(1.,-1.57698425990146E-13,0.));
#31225=DIRECTION('',(0.,0.,1.));
#31226=DIRECTION('center_axis',(0.,0.,1.));
#31227=DIRECTION('ref_axis',(1.,-1.57698425990146E-13,0.));
#31228=DIRECTION('',(0.,0.,1.));
#31229=DIRECTION('center_axis',(0.,0.,1.));
#31230=DIRECTION('ref_axis',(1.,-1.57698425990146E-13,0.));
#31231=DIRECTION('',(0.,0.,1.));
#31232=DIRECTION('center_axis',(0.,0.,1.));
#31233=DIRECTION('ref_axis',(1.,-1.57698425990146E-13,0.));
#31234=DIRECTION('',(0.,0.,1.));
#31235=DIRECTION('center_axis',(0.,0.,1.));
#31236=DIRECTION('ref_axis',(1.,-1.57698425990146E-13,0.));
#31237=DIRECTION('',(0.,0.,1.));
#31238=DIRECTION('center_axis',(0.,0.,1.));
#31239=DIRECTION('ref_axis',(1.,-1.57698425990146E-13,0.));
#31240=DIRECTION('',(0.,0.,1.));
#31241=DIRECTION('center_axis',(0.,0.,1.));
#31242=DIRECTION('ref_axis',(1.,-1.57698425990146E-13,0.));
#31243=DIRECTION('',(0.,0.,1.));
#31244=DIRECTION('center_axis',(0.,0.,1.));
#31245=DIRECTION('ref_axis',(1.,-1.57698425990146E-13,0.));
#31246=DIRECTION('',(0.,0.,1.));
#31247=DIRECTION('center_axis',(0.,0.,1.));
#31248=DIRECTION('ref_axis',(1.,-1.57698425990146E-13,0.));
#31249=DIRECTION('',(0.,0.,1.));
#31250=DIRECTION('center_axis',(0.,0.,1.));
#31251=DIRECTION('ref_axis',(1.,-1.57698425990146E-13,0.));
#31252=DIRECTION('',(0.,0.,1.));
#31253=DIRECTION('center_axis',(0.,0.,1.));
#31254=DIRECTION('ref_axis',(1.,-1.57698425990146E-13,0.));
#31255=DIRECTION('',(0.,0.,1.));
#31256=DIRECTION('center_axis',(0.,0.,1.));
#31257=DIRECTION('ref_axis',(1.,-1.57698425990146E-13,0.));
#31258=DIRECTION('',(0.,0.,1.));
#31259=DIRECTION('center_axis',(0.,0.,1.));
#31260=DIRECTION('ref_axis',(1.,-1.57698425990146E-13,0.));
#31261=DIRECTION('',(0.,0.,1.));
#31262=DIRECTION('center_axis',(0.,0.,1.));
#31263=DIRECTION('ref_axis',(1.,-1.57698425990146E-13,0.));
#31264=DIRECTION('',(0.,0.,1.));
#31265=DIRECTION('center_axis',(0.,0.,1.));
#31266=DIRECTION('ref_axis',(1.,-1.57698425990146E-13,0.));
#31267=DIRECTION('',(0.,0.,1.));
#31268=DIRECTION('center_axis',(0.,0.,1.));
#31269=DIRECTION('ref_axis',(1.,-1.57698425990146E-13,0.));
#31270=DIRECTION('',(0.,0.,1.));
#31271=DIRECTION('center_axis',(0.,0.,1.));
#31272=DIRECTION('ref_axis',(1.,-1.57698425990146E-13,0.));
#31273=DIRECTION('',(0.,0.,1.));
#31274=DIRECTION('center_axis',(0.,0.,1.));
#31275=DIRECTION('ref_axis',(1.,-1.57698425990146E-13,0.));
#31276=DIRECTION('',(0.,0.,1.));
#31277=DIRECTION('center_axis',(0.,0.,1.));
#31278=DIRECTION('ref_axis',(1.,-1.57698425990146E-13,0.));
#31279=DIRECTION('',(0.,0.,1.));
#31280=DIRECTION('center_axis',(0.,0.,1.));
#31281=DIRECTION('ref_axis',(1.,-1.57698425990146E-13,0.));
#31282=DIRECTION('',(0.,0.,1.));
#31283=DIRECTION('center_axis',(0.,0.,1.));
#31284=DIRECTION('ref_axis',(1.,-1.57698425990146E-13,0.));
#31285=DIRECTION('',(0.,0.,1.));
#31286=DIRECTION('center_axis',(0.,0.,1.));
#31287=DIRECTION('ref_axis',(1.,-1.57698425990146E-13,0.));
#31288=DIRECTION('',(0.,0.,1.));
#31289=DIRECTION('center_axis',(0.,0.,1.));
#31290=DIRECTION('ref_axis',(1.,-1.57698425990146E-13,0.));
#31291=DIRECTION('',(0.,0.,1.));
#31292=DIRECTION('center_axis',(0.,0.,1.));
#31293=DIRECTION('ref_axis',(1.,-1.57698425990146E-13,0.));
#31294=DIRECTION('',(0.,0.,1.));
#31295=DIRECTION('center_axis',(0.,0.,-1.));
#31296=DIRECTION('ref_axis',(1.,-1.57698425990146E-13,0.));
#31297=DIRECTION('center_axis',(0.,0.,1.));
#31298=DIRECTION('ref_axis',(1.,0.,0.));
#31299=DIRECTION('center_axis',(0.,0.,1.));
#31300=DIRECTION('ref_axis',(1.,0.,0.));
#31301=DIRECTION('center_axis',(0.,0.,1.));
#31302=DIRECTION('ref_axis',(1.,0.,0.));
#31303=DIRECTION('center_axis',(0.,0.,1.));
#31304=DIRECTION('ref_axis',(1.,0.,0.));
#31305=DIRECTION('center_axis',(0.,0.,-1.));
#31306=DIRECTION('ref_axis',(1.,-1.57698425990146E-13,0.));
#31307=DIRECTION('center_axis',(0.,0.,1.));
#31308=DIRECTION('ref_axis',(-0.952281269972968,0.30522185842215,0.));
#31309=DIRECTION('center_axis',(0.,0.,1.));
#31310=DIRECTION('ref_axis',(0.984807753012208,-0.17364817766693,0.));
#31311=DIRECTION('center_axis',(0.,0.,-1.));
#31312=DIRECTION('ref_axis',(1.,0.,0.));
#31313=DIRECTION('',(-0.996089805327885,-0.0883464754353932,0.));
#31314=DIRECTION('',(0.905801965515954,-0.423701309022563,0.));
#31315=DIRECTION('center_axis',(-0.423701309022563,-0.905801965515954,0.));
#31316=DIRECTION('ref_axis',(0.905801965515954,-0.423701309022563,0.));
#31317=DIRECTION('',(0.,0.,1.));
#31318=DIRECTION('',(0.,0.,1.));
#31319=DIRECTION('center_axis',(-0.0883464754353932,0.996089805327885,0.));
#31320=DIRECTION('ref_axis',(-0.996089805327885,-0.0883464754353932,0.));
#31321=DIRECTION('',(0.,0.,-1.));
#31322=DIRECTION('center_axis',(0.,0.,1.));
#31323=DIRECTION('ref_axis',(0.939692620785908,-0.342020143325669,0.));
#31324=DIRECTION('center_axis',(0.,0.,-1.));
#31325=DIRECTION('ref_axis',(1.,0.,0.));
#31326=DIRECTION('',(-0.996298167445974,0.0859648855277176,0.));
#31327=DIRECTION('',(0.818465838146947,-0.574555194725812,0.));
#31328=DIRECTION('center_axis',(-0.574555194725812,-0.818465838146947,0.));
#31329=DIRECTION('ref_axis',(0.818465838146947,-0.574555194725812,0.));
#31330=DIRECTION('',(0.,0.,1.));
#31331=DIRECTION('',(0.,0.,1.));
#31332=DIRECTION('center_axis',(0.0859648855277176,0.996298167445974,0.));
#31333=DIRECTION('ref_axis',(-0.996298167445974,0.0859648855277176,0.));
#31334=DIRECTION('',(0.,0.,-1.));
#31335=DIRECTION('center_axis',(0.,0.,1.));
#31336=DIRECTION('ref_axis',(0.866025403784438,-0.5,0.));
#31337=DIRECTION('center_axis',(0.,0.,-1.));
#31338=DIRECTION('ref_axis',(1.,0.,0.));
#31339=DIRECTION('',(-0.966234513897416,0.257664246944399,0.));
#31340=DIRECTION('',(0.706261040449543,-0.707951511576272,0.));
#31341=DIRECTION('center_axis',(-0.707951511576272,-0.706261040449543,0.));
#31342=DIRECTION('ref_axis',(0.706261040449543,-0.707951511576272,0.));
#31343=DIRECTION('',(0.,0.,1.));
#31344=DIRECTION('',(0.,0.,1.));
#31345=DIRECTION('center_axis',(0.257664246944399,0.966234513897416,0.));
#31346=DIRECTION('ref_axis',(-0.966234513897416,0.257664246944399,0.));
#31347=DIRECTION('',(0.,0.,-1.));
#31348=DIRECTION('center_axis',(0.,0.,1.));
#31349=DIRECTION('ref_axis',(0.766044443118978,-0.64278760968654,0.));
#31350=DIRECTION('center_axis',(0.,0.,-1.));
#31351=DIRECTION('ref_axis',(1.,0.,0.));
#31352=DIRECTION('',(-0.906812313582341,0.421534610602074,0.));
#31353=DIRECTION('',(0.572596858423411,-0.819837079988238,0.));
#31354=DIRECTION('center_axis',(-0.819837079988238,-0.572596858423411,0.));
#31355=DIRECTION('ref_axis',(0.572596858423411,-0.819837079988238,0.));
#31356=DIRECTION('',(0.,0.,1.));
#31357=DIRECTION('',(0.,0.,1.));
#31358=DIRECTION('center_axis',(0.421534610602074,0.906812313582341,0.));
#31359=DIRECTION('ref_axis',(-0.906812313582341,0.421534610602074,0.));
#31360=DIRECTION('',(0.,0.,-1.));
#31361=DIRECTION('center_axis',(0.,0.,1.));
#31362=DIRECTION('ref_axis',(0.642787609686539,-0.766044443118978,0.));
#31363=DIRECTION('center_axis',(0.,0.,-1.));
#31364=DIRECTION('ref_axis',(1.,0.,0.));
#31365=DIRECTION('',(-0.819837079988238,0.572596858423411,0.));
#31366=DIRECTION('',(0.421534610602074,-0.906812313582341,0.));
#31367=DIRECTION('center_axis',(-0.906812313582341,-0.421534610602074,0.));
#31368=DIRECTION('ref_axis',(0.421534610602074,-0.906812313582341,0.));
#31369=DIRECTION('',(0.,0.,1.));
#31370=DIRECTION('',(0.,0.,1.));
#31371=DIRECTION('center_axis',(0.572596858423411,0.819837079988238,0.));
#31372=DIRECTION('ref_axis',(-0.819837079988238,0.572596858423411,0.));
#31373=DIRECTION('',(0.,0.,-1.));
#31374=DIRECTION('center_axis',(0.,0.,1.));
#31375=DIRECTION('ref_axis',(0.5,-0.866025403784438,0.));
#31376=DIRECTION('center_axis',(0.,0.,-1.));
#31377=DIRECTION('ref_axis',(1.,0.,0.));
#31378=DIRECTION('',(-0.707951511576272,0.706261040449544,0.));
#31379=DIRECTION('',(0.257664246944398,-0.966234513897416,0.));
#31380=DIRECTION('center_axis',(-0.966234513897416,-0.257664246944398,0.));
#31381=DIRECTION('ref_axis',(0.257664246944398,-0.966234513897416,0.));
#31382=DIRECTION('',(0.,0.,1.));
#31383=DIRECTION('',(0.,0.,1.));
#31384=DIRECTION('center_axis',(0.706261040449544,0.707951511576272,0.));
#31385=DIRECTION('ref_axis',(-0.707951511576272,0.706261040449544,0.));
#31386=DIRECTION('',(0.,0.,-1.));
#31387=DIRECTION('center_axis',(0.,0.,1.));
#31388=DIRECTION('ref_axis',(0.342020143325668,-0.939692620785909,0.));
#31389=DIRECTION('center_axis',(0.,0.,-1.));
#31390=DIRECTION('ref_axis',(1.,0.,0.));
#31391=DIRECTION('',(-0.57455519472581,0.818465838146948,0.));
#31392=DIRECTION('',(0.0859648855277162,-0.996298167445974,0.));
#31393=DIRECTION('center_axis',(-0.996298167445974,-0.0859648855277162,
0.));
#31394=DIRECTION('ref_axis',(0.0859648855277162,-0.996298167445974,0.));
#31395=DIRECTION('',(0.,0.,1.));
#31396=DIRECTION('',(0.,0.,1.));
#31397=DIRECTION('center_axis',(0.818465838146948,0.57455519472581,0.));
#31398=DIRECTION('ref_axis',(-0.57455519472581,0.818465838146948,0.));
#31399=DIRECTION('',(0.,0.,-1.));
#31400=DIRECTION('center_axis',(0.,0.,1.));
#31401=DIRECTION('ref_axis',(0.17364817766693,-0.984807753012208,0.));
#31402=DIRECTION('center_axis',(0.,0.,-1.));
#31403=DIRECTION('ref_axis',(1.,0.,0.));
#31404=DIRECTION('',(-0.423701309022563,0.905801965515955,0.));
#31405=DIRECTION('',(-0.0883464754353936,-0.996089805327885,0.));
#31406=DIRECTION('center_axis',(-0.996089805327885,0.0883464754353937,0.));
#31407=DIRECTION('ref_axis',(-0.0883464754353937,-0.996089805327885,0.));
#31408=DIRECTION('',(0.,0.,1.));
#31409=DIRECTION('',(0.,0.,1.));
#31410=DIRECTION('center_axis',(0.905801965515955,0.423701309022563,0.));
#31411=DIRECTION('ref_axis',(-0.423701309022563,0.905801965515955,0.));
#31412=DIRECTION('',(0.,0.,-1.));
#31413=DIRECTION('center_axis',(0.,0.,1.));
#31414=DIRECTION('ref_axis',(-1.94289029309402E-16,-1.,0.));
#31415=DIRECTION('center_axis',(0.,0.,-1.));
#31416=DIRECTION('ref_axis',(1.,0.,0.));
#31417=DIRECTION('',(-0.259973473447872,0.96561575852067,0.));
#31418=DIRECTION('',(-0.259973473447873,-0.96561575852067,0.));
#31419=DIRECTION('center_axis',(-0.96561575852067,0.259973473447873,0.));
#31420=DIRECTION('ref_axis',(-0.259973473447873,-0.96561575852067,0.));
#31421=DIRECTION('',(0.,0.,1.));
#31422=DIRECTION('',(0.,0.,1.));
#31423=DIRECTION('center_axis',(0.96561575852067,0.259973473447872,0.));
#31424=DIRECTION('ref_axis',(-0.259973473447872,0.96561575852067,0.));
#31425=DIRECTION('',(0.,0.,-1.));
#31426=DIRECTION('center_axis',(0.,0.,1.));
#31427=DIRECTION('ref_axis',(-0.17364817766693,-0.984807753012208,0.));
#31428=DIRECTION('center_axis',(0.,0.,-1.));
#31429=DIRECTION('ref_axis',(1.,0.,0.));
#31430=DIRECTION('',(-0.0883464754353933,0.996089805327885,0.));
#31431=DIRECTION('',(-0.423701309022563,-0.905801965515955,0.));
#31432=DIRECTION('center_axis',(-0.905801965515955,0.423701309022563,0.));
#31433=DIRECTION('ref_axis',(-0.423701309022563,-0.905801965515955,0.));
#31434=DIRECTION('',(0.,0.,1.));
#31435=DIRECTION('',(0.,0.,1.));
#31436=DIRECTION('center_axis',(0.996089805327885,0.0883464754353932,0.));
#31437=DIRECTION('ref_axis',(-0.0883464754353932,0.996089805327885,0.));
#31438=DIRECTION('',(0.,0.,-1.));
#31439=DIRECTION('center_axis',(0.,0.,1.));
#31440=DIRECTION('ref_axis',(-0.342020143325669,-0.939692620785908,0.));
#31441=DIRECTION('center_axis',(0.,0.,-1.));
#31442=DIRECTION('ref_axis',(1.,0.,0.));
#31443=DIRECTION('',(0.0859648855277175,0.996298167445974,0.));
#31444=DIRECTION('',(-0.574555194725811,-0.818465838146947,0.));
#31445=DIRECTION('center_axis',(-0.818465838146947,0.574555194725811,0.));
#31446=DIRECTION('ref_axis',(-0.574555194725811,-0.818465838146947,0.));
#31447=DIRECTION('',(0.,0.,1.));
#31448=DIRECTION('',(0.,0.,1.));
#31449=DIRECTION('center_axis',(0.996298167445974,-0.0859648855277175,0.));
#31450=DIRECTION('ref_axis',(0.0859648855277175,0.996298167445974,0.));
#31451=DIRECTION('',(0.,0.,-1.));
#31452=DIRECTION('center_axis',(0.,0.,1.));
#31453=DIRECTION('ref_axis',(-0.5,-0.866025403784438,0.));
#31454=DIRECTION('center_axis',(0.,0.,-1.));
#31455=DIRECTION('ref_axis',(1.,0.,0.));
#31456=DIRECTION('',(0.257664246944399,0.966234513897416,0.));
#31457=DIRECTION('',(-0.707951511576272,-0.706261040449543,0.));
#31458=DIRECTION('center_axis',(-0.706261040449543,0.707951511576272,0.));
#31459=DIRECTION('ref_axis',(-0.707951511576272,-0.706261040449543,0.));
#31460=DIRECTION('',(0.,0.,1.));
#31461=DIRECTION('',(0.,0.,1.));
#31462=DIRECTION('center_axis',(0.966234513897416,-0.257664246944399,0.));
#31463=DIRECTION('ref_axis',(0.257664246944399,0.966234513897416,0.));
#31464=DIRECTION('',(0.,0.,-1.));
#31465=DIRECTION('center_axis',(0.,0.,1.));
#31466=DIRECTION('ref_axis',(-0.642787609686539,-0.766044443118978,0.));
#31467=DIRECTION('center_axis',(0.,0.,-1.));
#31468=DIRECTION('ref_axis',(1.,0.,0.));
#31469=DIRECTION('',(0.421534610602074,0.906812313582341,0.));
#31470=DIRECTION('',(-0.819837079988238,-0.572596858423411,0.));
#31471=DIRECTION('center_axis',(-0.572596858423411,0.819837079988238,0.));
#31472=DIRECTION('ref_axis',(-0.819837079988238,-0.572596858423411,0.));
#31473=DIRECTION('',(0.,0.,1.));
#31474=DIRECTION('',(0.,0.,1.));
#31475=DIRECTION('center_axis',(0.906812313582341,-0.421534610602074,0.));
#31476=DIRECTION('ref_axis',(0.421534610602074,0.906812313582341,0.));
#31477=DIRECTION('',(0.,0.,-1.));
#31478=DIRECTION('center_axis',(0.,0.,1.));
#31479=DIRECTION('ref_axis',(-0.766044443118978,-0.642787609686539,0.));
#31480=DIRECTION('center_axis',(0.,0.,-1.));
#31481=DIRECTION('ref_axis',(1.,0.,0.));
#31482=DIRECTION('',(0.572596858423411,0.819837079988238,0.));
#31483=DIRECTION('',(-0.906812313582341,-0.421534610602074,0.));
#31484=DIRECTION('center_axis',(-0.421534610602074,0.906812313582341,0.));
#31485=DIRECTION('ref_axis',(-0.906812313582341,-0.421534610602074,0.));
#31486=DIRECTION('',(0.,0.,1.));
#31487=DIRECTION('',(0.,0.,1.));
#31488=DIRECTION('center_axis',(0.819837079988238,-0.572596858423411,0.));
#31489=DIRECTION('ref_axis',(0.572596858423411,0.819837079988238,0.));
#31490=DIRECTION('',(0.,0.,-1.));
#31491=DIRECTION('center_axis',(0.,0.,1.));
#31492=DIRECTION('ref_axis',(-0.866025403784439,-0.5,0.));
#31493=DIRECTION('center_axis',(0.,0.,-1.));
#31494=DIRECTION('ref_axis',(1.,0.,0.));
#31495=DIRECTION('',(0.706261040449544,0.707951511576271,0.));
#31496=DIRECTION('',(-0.966234513897416,-0.257664246944398,0.));
#31497=DIRECTION('center_axis',(-0.257664246944398,0.966234513897416,0.));
#31498=DIRECTION('ref_axis',(-0.966234513897416,-0.257664246944398,0.));
#31499=DIRECTION('',(0.,0.,1.));
#31500=DIRECTION('',(0.,0.,1.));
#31501=DIRECTION('center_axis',(0.707951511576271,-0.706261040449544,0.));
#31502=DIRECTION('ref_axis',(0.706261040449544,0.707951511576271,0.));
#31503=DIRECTION('',(0.,0.,-1.));
#31504=DIRECTION('center_axis',(0.,0.,1.));
#31505=DIRECTION('ref_axis',(-0.939692620785909,-0.342020143325669,0.));
#31506=DIRECTION('center_axis',(0.,0.,-1.));
#31507=DIRECTION('ref_axis',(1.,0.,0.));
#31508=DIRECTION('',(0.818465838146948,0.574555194725811,0.));
#31509=DIRECTION('',(-0.996298167445974,-0.0859648855277167,0.));
#31510=DIRECTION('center_axis',(-0.0859648855277167,0.996298167445974,0.));
#31511=DIRECTION('ref_axis',(-0.996298167445974,-0.0859648855277167,0.));
#31512=DIRECTION('',(0.,0.,1.));
#31513=DIRECTION('',(0.,0.,1.));
#31514=DIRECTION('center_axis',(0.574555194725811,-0.818465838146948,0.));
#31515=DIRECTION('ref_axis',(0.818465838146948,0.574555194725811,0.));
#31516=DIRECTION('',(0.,0.,-1.));
#31517=DIRECTION('center_axis',(0.,0.,1.));
#31518=DIRECTION('ref_axis',(-0.984807753012208,-0.17364817766693,0.));
#31519=DIRECTION('center_axis',(0.,0.,-1.));
#31520=DIRECTION('ref_axis',(1.,0.,0.));
#31521=DIRECTION('',(0.905801965515955,0.423701309022563,0.));
#31522=DIRECTION('',(-0.996089805327885,0.0883464754353936,0.));
#31523=DIRECTION('center_axis',(0.0883464754353936,0.996089805327885,0.));
#31524=DIRECTION('ref_axis',(-0.996089805327885,0.0883464754353936,0.));
#31525=DIRECTION('',(0.,0.,1.));
#31526=DIRECTION('',(0.,0.,1.));
#31527=DIRECTION('center_axis',(0.423701309022563,-0.905801965515955,0.));
#31528=DIRECTION('ref_axis',(0.905801965515955,0.423701309022563,0.));
#31529=DIRECTION('',(0.,0.,-1.));
#31530=DIRECTION('center_axis',(0.,0.,1.));
#31531=DIRECTION('ref_axis',(-1.,1.11022302462516E-16,0.));
#31532=DIRECTION('center_axis',(0.,0.,-1.));
#31533=DIRECTION('ref_axis',(1.,0.,0.));
#31534=DIRECTION('',(0.96561575852067,0.259973473447872,0.));
#31535=DIRECTION('',(-0.96561575852067,0.259973473447873,0.));
#31536=DIRECTION('center_axis',(0.,0.,-1.));
#31537=DIRECTION('ref_axis',(1.,0.,0.));
#31538=DIRECTION('center_axis',(0.259973473447873,0.96561575852067,0.));
#31539=DIRECTION('ref_axis',(-0.96561575852067,0.259973473447873,0.));
#31540=DIRECTION('',(0.,0.,1.));
#31541=DIRECTION('',(0.,0.,1.));
#31542=DIRECTION('center_axis',(0.259973473447872,-0.96561575852067,0.));
#31543=DIRECTION('ref_axis',(0.96561575852067,0.259973473447872,0.));
#31544=DIRECTION('',(0.,0.,-1.));
#31545=DIRECTION('center_axis',(0.,0.,1.));
#31546=DIRECTION('ref_axis',(-0.984807753012208,0.173648177666931,0.));
#31547=DIRECTION('center_axis',(0.,0.,-1.));
#31548=DIRECTION('ref_axis',(1.,0.,0.));
#31549=DIRECTION('',(0.996089805327885,0.0883464754353928,0.));
#31550=DIRECTION('',(-0.905801965515954,0.423701309022564,0.));
#31551=DIRECTION('center_axis',(0.423701309022564,0.905801965515954,0.));
#31552=DIRECTION('ref_axis',(-0.905801965515954,0.423701309022564,0.));
#31553=DIRECTION('',(0.,0.,1.));
#31554=DIRECTION('',(0.,0.,1.));
#31555=DIRECTION('center_axis',(0.0883464754353928,-0.996089805327885,0.));
#31556=DIRECTION('ref_axis',(0.996089805327885,0.0883464754353928,0.));
#31557=DIRECTION('',(0.,0.,-1.));
#31558=DIRECTION('center_axis',(0.,0.,1.));
#31559=DIRECTION('ref_axis',(-0.939692620785908,0.342020143325669,0.));
#31560=DIRECTION('center_axis',(0.,0.,-1.));
#31561=DIRECTION('ref_axis',(1.,0.,0.));
#31562=DIRECTION('',(0.996298167445974,-0.085964885527717,0.));
#31563=DIRECTION('',(-0.818465838146948,0.574555194725811,0.));
#31564=DIRECTION('center_axis',(0.574555194725811,0.818465838146948,0.));
#31565=DIRECTION('ref_axis',(-0.818465838146948,0.574555194725811,0.));
#31566=DIRECTION('',(0.,0.,1.));
#31567=DIRECTION('',(0.,0.,1.));
#31568=DIRECTION('center_axis',(-0.085964885527717,-0.996298167445974,0.));
#31569=DIRECTION('ref_axis',(0.996298167445974,-0.085964885527717,0.));
#31570=DIRECTION('',(0.,0.,-1.));
#31571=DIRECTION('center_axis',(0.,0.,1.));
#31572=DIRECTION('ref_axis',(-0.866025403784439,0.5,0.));
#31573=DIRECTION('center_axis',(0.,0.,-1.));
#31574=DIRECTION('ref_axis',(1.,0.,0.));
#31575=DIRECTION('',(0.966234513897416,-0.257664246944398,0.));
#31576=DIRECTION('',(-0.706261040449544,0.707951511576272,0.));
#31577=DIRECTION('center_axis',(0.707951511576272,0.706261040449544,0.));
#31578=DIRECTION('ref_axis',(-0.706261040449544,0.707951511576272,0.));
#31579=DIRECTION('',(0.,0.,1.));
#31580=DIRECTION('',(0.,0.,1.));
#31581=DIRECTION('center_axis',(-0.257664246944398,-0.966234513897416,0.));
#31582=DIRECTION('ref_axis',(0.966234513897416,-0.257664246944398,0.));
#31583=DIRECTION('',(0.,0.,-1.));
#31584=DIRECTION('center_axis',(0.,0.,1.));
#31585=DIRECTION('ref_axis',(-0.766044443118978,0.642787609686539,0.));
#31586=DIRECTION('center_axis',(0.,0.,-1.));
#31587=DIRECTION('ref_axis',(1.,0.,0.));
#31588=DIRECTION('',(0.906812313582341,-0.421534610602074,0.));
#31589=DIRECTION('',(-0.572596858423411,0.819837079988238,0.));
#31590=DIRECTION('center_axis',(0.819837079988238,0.572596858423411,0.));
#31591=DIRECTION('ref_axis',(-0.572596858423411,0.819837079988238,0.));
#31592=DIRECTION('',(0.,0.,1.));
#31593=DIRECTION('',(0.,0.,1.));
#31594=DIRECTION('center_axis',(-0.421534610602074,-0.906812313582341,0.));
#31595=DIRECTION('ref_axis',(0.906812313582341,-0.421534610602074,0.));
#31596=DIRECTION('',(0.,0.,-1.));
#31597=DIRECTION('center_axis',(0.,0.,1.));
#31598=DIRECTION('ref_axis',(-0.642787609686539,0.766044443118978,0.));
#31599=DIRECTION('center_axis',(0.,0.,-1.));
#31600=DIRECTION('ref_axis',(1.,0.,0.));
#31601=DIRECTION('',(0.819837079988238,-0.572596858423411,0.));
#31602=DIRECTION('',(-0.421534610602074,0.906812313582341,0.));
#31603=DIRECTION('center_axis',(0.906812313582341,0.421534610602074,0.));
#31604=DIRECTION('ref_axis',(-0.421534610602074,0.906812313582341,0.));
#31605=DIRECTION('',(0.,0.,1.));
#31606=DIRECTION('',(0.,0.,1.));
#31607=DIRECTION('center_axis',(-0.572596858423411,-0.819837079988238,0.));
#31608=DIRECTION('ref_axis',(0.819837079988238,-0.572596858423411,0.));
#31609=DIRECTION('',(0.,0.,-1.));
#31610=DIRECTION('center_axis',(0.,0.,1.));
#31611=DIRECTION('ref_axis',(-0.5,0.866025403784439,0.));
#31612=DIRECTION('center_axis',(0.,0.,-1.));
#31613=DIRECTION('ref_axis',(1.,0.,0.));
#31614=DIRECTION('',(0.707951511576272,-0.706261040449544,0.));
#31615=DIRECTION('',(-0.257664246944398,0.966234513897416,0.));
#31616=DIRECTION('center_axis',(0.966234513897416,0.257664246944398,0.));
#31617=DIRECTION('ref_axis',(-0.257664246944398,0.966234513897416,0.));
#31618=DIRECTION('',(0.,0.,1.));
#31619=DIRECTION('',(0.,0.,1.));
#31620=DIRECTION('center_axis',(-0.706261040449544,-0.707951511576272,0.));
#31621=DIRECTION('ref_axis',(0.707951511576272,-0.706261040449544,0.));
#31622=DIRECTION('',(0.,0.,-1.));
#31623=DIRECTION('center_axis',(0.,0.,1.));
#31624=DIRECTION('ref_axis',(-0.342020143325669,0.939692620785909,0.));
#31625=DIRECTION('center_axis',(0.,0.,-1.));
#31626=DIRECTION('ref_axis',(1.,0.,0.));
#31627=DIRECTION('',(0.574555194725811,-0.818465838146948,0.));
#31628=DIRECTION('',(-0.0859648855277167,0.996298167445974,0.));
#31629=DIRECTION('center_axis',(0.996298167445974,0.0859648855277167,0.));
#31630=DIRECTION('ref_axis',(-0.0859648855277167,0.996298167445974,0.));
#31631=DIRECTION('',(0.,0.,1.));
#31632=DIRECTION('',(0.,0.,1.));
#31633=DIRECTION('center_axis',(-0.818465838146948,-0.574555194725811,0.));
#31634=DIRECTION('ref_axis',(0.574555194725811,-0.818465838146948,0.));
#31635=DIRECTION('',(0.,0.,-1.));
#31636=DIRECTION('center_axis',(0.,0.,1.));
#31637=DIRECTION('ref_axis',(-0.17364817766693,0.984807753012208,0.));
#31638=DIRECTION('center_axis',(0.,0.,-1.));
#31639=DIRECTION('ref_axis',(1.,0.,0.));
#31640=DIRECTION('',(0.423701309022563,-0.905801965515955,0.));
#31641=DIRECTION('',(0.0883464754353932,0.996089805327885,0.));
#31642=DIRECTION('center_axis',(0.996089805327885,-0.0883464754353932,0.));
#31643=DIRECTION('ref_axis',(0.0883464754353932,0.996089805327885,0.));
#31644=DIRECTION('',(0.,0.,1.));
#31645=DIRECTION('',(0.,0.,1.));
#31646=DIRECTION('center_axis',(-0.905801965515955,-0.423701309022563,0.));
#31647=DIRECTION('ref_axis',(0.423701309022563,-0.905801965515955,0.));
#31648=DIRECTION('',(0.,0.,-1.));
#31649=DIRECTION('center_axis',(0.,0.,1.));
#31650=DIRECTION('ref_axis',(5.55111512312578E-17,1.,0.));
#31651=DIRECTION('center_axis',(0.,0.,-1.));
#31652=DIRECTION('ref_axis',(1.,0.,0.));
#31653=DIRECTION('',(0.259973473447872,-0.96561575852067,0.));
#31654=DIRECTION('',(0.259973473447872,0.96561575852067,0.));
#31655=DIRECTION('center_axis',(0.96561575852067,-0.259973473447873,0.));
#31656=DIRECTION('ref_axis',(0.259973473447873,0.96561575852067,0.));
#31657=DIRECTION('',(0.,0.,1.));
#31658=DIRECTION('',(0.,0.,1.));
#31659=DIRECTION('center_axis',(-0.96561575852067,-0.259973473447872,0.));
#31660=DIRECTION('ref_axis',(0.259973473447872,-0.96561575852067,0.));
#31661=DIRECTION('',(0.,0.,-1.));
#31662=DIRECTION('center_axis',(0.,0.,1.));
#31663=DIRECTION('ref_axis',(0.17364817766693,0.984807753012208,0.));
#31664=DIRECTION('center_axis',(0.,0.,-1.));
#31665=DIRECTION('ref_axis',(1.,0.,0.));
#31666=DIRECTION('',(0.0883464754353931,-0.996089805327885,0.));
#31667=DIRECTION('',(0.423701309022563,0.905801965515954,0.));
#31668=DIRECTION('center_axis',(0.905801965515954,-0.423701309022563,0.));
#31669=DIRECTION('ref_axis',(0.423701309022563,0.905801965515954,0.));
#31670=DIRECTION('',(0.,0.,1.));
#31671=DIRECTION('',(0.,0.,1.));
#31672=DIRECTION('center_axis',(-0.996089805327885,-0.0883464754353932,
0.));
#31673=DIRECTION('ref_axis',(0.0883464754353932,-0.996089805327885,0.));
#31674=DIRECTION('',(0.,0.,-1.));
#31675=DIRECTION('center_axis',(0.,0.,1.));
#31676=DIRECTION('ref_axis',(0.342020143325669,0.939692620785908,0.));
#31677=DIRECTION('center_axis',(0.,0.,-1.));
#31678=DIRECTION('ref_axis',(1.,0.,0.));
#31679=DIRECTION('',(-0.085964885527717,-0.996298167445974,0.));
#31680=DIRECTION('',(0.574555194725811,0.818465838146948,0.));
#31681=DIRECTION('center_axis',(0.818465838146948,-0.574555194725811,0.));
#31682=DIRECTION('ref_axis',(0.574555194725811,0.818465838146948,0.));
#31683=DIRECTION('',(0.,0.,1.));
#31684=DIRECTION('',(0.,0.,1.));
#31685=DIRECTION('center_axis',(-0.996298167445974,0.085964885527717,0.));
#31686=DIRECTION('ref_axis',(-0.085964885527717,-0.996298167445974,0.));
#31687=DIRECTION('',(0.,0.,-1.));
#31688=DIRECTION('center_axis',(0.,0.,1.));
#31689=DIRECTION('ref_axis',(0.5,0.866025403784439,0.));
#31690=DIRECTION('center_axis',(0.,0.,-1.));
#31691=DIRECTION('ref_axis',(1.,0.,0.));
#31692=DIRECTION('',(-0.257664246944398,-0.966234513897416,0.));
#31693=DIRECTION('',(0.707951511576272,0.706261040449544,0.));
#31694=DIRECTION('center_axis',(0.706261040449544,-0.707951511576272,0.));
#31695=DIRECTION('ref_axis',(0.707951511576272,0.706261040449544,0.));
#31696=DIRECTION('',(0.,0.,1.));
#31697=DIRECTION('',(0.,0.,1.));
#31698=DIRECTION('center_axis',(-0.966234513897416,0.257664246944398,0.));
#31699=DIRECTION('ref_axis',(-0.257664246944398,-0.966234513897416,0.));
#31700=DIRECTION('',(0.,0.,-1.));
#31701=DIRECTION('center_axis',(0.,0.,1.));
#31702=DIRECTION('ref_axis',(0.642787609686539,0.766044443118978,0.));
#31703=DIRECTION('center_axis',(0.,0.,-1.));
#31704=DIRECTION('ref_axis',(1.,0.,0.));
#31705=DIRECTION('',(-0.421534610602074,-0.906812313582341,0.));
#31706=DIRECTION('',(0.819837079988238,0.572596858423411,0.));
#31707=DIRECTION('center_axis',(0.572596858423411,-0.819837079988238,0.));
#31708=DIRECTION('ref_axis',(0.819837079988238,0.572596858423411,0.));
#31709=DIRECTION('',(0.,0.,1.));
#31710=DIRECTION('',(0.,0.,1.));
#31711=DIRECTION('center_axis',(-0.906812313582341,0.421534610602074,0.));
#31712=DIRECTION('ref_axis',(-0.421534610602074,-0.906812313582341,0.));
#31713=DIRECTION('',(0.,0.,-1.));
#31714=DIRECTION('center_axis',(0.,0.,1.));
#31715=DIRECTION('ref_axis',(0.766044443118978,0.642787609686539,0.));
#31716=DIRECTION('center_axis',(0.,0.,-1.));
#31717=DIRECTION('ref_axis',(1.,0.,0.));
#31718=DIRECTION('',(-0.572596858423411,-0.819837079988238,0.));
#31719=DIRECTION('',(0.906812313582341,0.421534610602074,0.));
#31720=DIRECTION('center_axis',(0.421534610602074,-0.906812313582341,0.));
#31721=DIRECTION('ref_axis',(0.906812313582341,0.421534610602074,0.));
#31722=DIRECTION('',(0.,0.,1.));
#31723=DIRECTION('',(0.,0.,1.));
#31724=DIRECTION('center_axis',(-0.819837079988238,0.572596858423411,0.));
#31725=DIRECTION('ref_axis',(-0.572596858423411,-0.819837079988238,0.));
#31726=DIRECTION('',(0.,0.,-1.));
#31727=DIRECTION('center_axis',(0.,0.,1.));
#31728=DIRECTION('ref_axis',(0.866025403784439,0.5,0.));
#31729=DIRECTION('center_axis',(0.,0.,-1.));
#31730=DIRECTION('ref_axis',(1.,0.,0.));
#31731=DIRECTION('',(-0.706261040449544,-0.707951511576272,0.));
#31732=DIRECTION('',(0.966234513897416,0.257664246944398,0.));
#31733=DIRECTION('center_axis',(0.257664246944398,-0.966234513897416,0.));
#31734=DIRECTION('ref_axis',(0.966234513897416,0.257664246944398,0.));
#31735=DIRECTION('',(0.,0.,1.));
#31736=DIRECTION('',(0.,0.,1.));
#31737=DIRECTION('center_axis',(-0.707951511576272,0.706261040449544,0.));
#31738=DIRECTION('ref_axis',(-0.706261040449544,-0.707951511576272,0.));
#31739=DIRECTION('',(0.,0.,-1.));
#31740=DIRECTION('center_axis',(0.,0.,1.));
#31741=DIRECTION('ref_axis',(0.939692620785909,0.342020143325669,0.));
#31742=DIRECTION('center_axis',(0.,0.,-1.));
#31743=DIRECTION('ref_axis',(1.,0.,0.));
#31744=DIRECTION('',(-0.818465838146948,-0.574555194725811,0.));
#31745=DIRECTION('',(0.996298167445974,0.0859648855277167,0.));
#31746=DIRECTION('center_axis',(0.0859648855277167,-0.996298167445974,0.));
#31747=DIRECTION('ref_axis',(0.996298167445974,0.0859648855277167,0.));
#31748=DIRECTION('',(0.,0.,1.));
#31749=DIRECTION('',(0.,0.,1.));
#31750=DIRECTION('center_axis',(-0.574555194725811,0.818465838146948,0.));
#31751=DIRECTION('ref_axis',(-0.818465838146948,-0.574555194725811,0.));
#31752=DIRECTION('',(0.,0.,-1.));
#31753=DIRECTION('center_axis',(0.,0.,1.));
#31754=DIRECTION('ref_axis',(0.984807753012208,0.17364817766693,0.));
#31755=DIRECTION('center_axis',(0.,0.,-1.));
#31756=DIRECTION('ref_axis',(1.,0.,0.));
#31757=DIRECTION('',(-0.905801965515955,-0.423701309022563,0.));
#31758=DIRECTION('',(0.996089805327885,-0.0883464754353932,0.));
#31759=DIRECTION('center_axis',(-0.0883464754353933,-0.996089805327885,
0.));
#31760=DIRECTION('ref_axis',(0.996089805327885,-0.0883464754353933,0.));
#31761=DIRECTION('',(0.,0.,1.));
#31762=DIRECTION('',(0.,0.,1.));
#31763=DIRECTION('center_axis',(-0.423701309022563,0.905801965515955,0.));
#31764=DIRECTION('ref_axis',(-0.905801965515954,-0.423701309022563,0.));
#31765=DIRECTION('',(0.,0.,-1.));
#31766=DIRECTION('center_axis',(0.,0.,1.));
#31767=DIRECTION('ref_axis',(1.,0.,0.));
#31768=DIRECTION('center_axis',(0.,0.,1.));
#31769=DIRECTION('ref_axis',(1.,0.,0.));
#31770=DIRECTION('center_axis',(0.,0.,1.));
#31771=DIRECTION('ref_axis',(1.,0.,0.));
#31772=DIRECTION('center_axis',(0.,0.,1.));
#31773=DIRECTION('ref_axis',(1.,0.,0.));
#31774=DIRECTION('center_axis',(0.,0.,1.));
#31775=DIRECTION('ref_axis',(1.,0.,0.));
#31776=DIRECTION('center_axis',(0.,0.,1.));
#31777=DIRECTION('ref_axis',(1.,0.,0.));
#31778=DIRECTION('center_axis',(0.,0.,1.));
#31779=DIRECTION('ref_axis',(1.,0.,0.));
#31780=DIRECTION('center_axis',(0.,0.,1.));
#31781=DIRECTION('ref_axis',(1.,0.,0.));
#31782=DIRECTION('center_axis',(0.,0.,1.));
#31783=DIRECTION('ref_axis',(1.,0.,0.));
#31784=DIRECTION('center_axis',(0.,0.,1.));
#31785=DIRECTION('ref_axis',(1.,0.,0.));
#31786=DIRECTION('center_axis',(0.,0.,1.));
#31787=DIRECTION('ref_axis',(1.,0.,0.));
#31788=DIRECTION('center_axis',(0.,0.,1.));
#31789=DIRECTION('ref_axis',(1.,0.,0.));
#31790=DIRECTION('center_axis',(0.,0.,1.));
#31791=DIRECTION('ref_axis',(1.,0.,0.));
#31792=DIRECTION('center_axis',(0.,0.,1.));
#31793=DIRECTION('ref_axis',(1.,0.,0.));
#31794=DIRECTION('center_axis',(0.,0.,1.));
#31795=DIRECTION('ref_axis',(1.,0.,0.));
#31796=DIRECTION('center_axis',(0.,0.,1.));
#31797=DIRECTION('ref_axis',(1.,0.,0.));
#31798=DIRECTION('center_axis',(0.,0.,1.));
#31799=DIRECTION('ref_axis',(1.,0.,0.));
#31800=DIRECTION('center_axis',(0.,0.,1.));
#31801=DIRECTION('ref_axis',(1.,0.,0.));
#31802=DIRECTION('',(0.,0.,-1.));
#31803=DIRECTION('center_axis',(0.,0.,1.));
#31804=DIRECTION('ref_axis',(1.,0.,0.));
#31805=DIRECTION('center_axis',(0.,0.,1.));
#31806=DIRECTION('ref_axis',(1.,0.,0.));
#31807=DIRECTION('center_axis',(0.,0.,1.));
#31808=DIRECTION('ref_axis',(1.,0.,0.));
#31809=DIRECTION('center_axis',(0.,0.,1.));
#31810=DIRECTION('ref_axis',(1.,0.,0.));
#31811=DIRECTION('center_axis',(0.,0.,1.));
#31812=DIRECTION('ref_axis',(1.,0.,0.));
#31813=DIRECTION('center_axis',(0.,0.,1.));
#31814=DIRECTION('ref_axis',(1.,0.,0.));
#31815=DIRECTION('center_axis',(0.,0.,1.));
#31816=DIRECTION('ref_axis',(1.,0.,0.));
#31817=DIRECTION('center_axis',(0.,0.,1.));
#31818=DIRECTION('ref_axis',(1.,0.,0.));
#31819=DIRECTION('center_axis',(0.,0.,1.));
#31820=DIRECTION('ref_axis',(1.,0.,0.));
#31821=DIRECTION('center_axis',(0.,0.,1.));
#31822=DIRECTION('ref_axis',(1.,0.,0.));
#31823=DIRECTION('center_axis',(0.,0.,1.));
#31824=DIRECTION('ref_axis',(1.,0.,0.));
#31825=DIRECTION('center_axis',(0.,0.,1.));
#31826=DIRECTION('ref_axis',(1.,0.,0.));
#31827=DIRECTION('center_axis',(0.,0.,1.));
#31828=DIRECTION('ref_axis',(1.,0.,0.));
#31829=DIRECTION('center_axis',(0.,0.,1.));
#31830=DIRECTION('ref_axis',(1.,0.,0.));
#31831=DIRECTION('center_axis',(0.,0.,1.));
#31832=DIRECTION('ref_axis',(1.,0.,0.));
#31833=DIRECTION('center_axis',(0.,0.,1.));
#31834=DIRECTION('ref_axis',(1.,0.,0.));
#31835=DIRECTION('center_axis',(0.,0.,1.));
#31836=DIRECTION('ref_axis',(1.,0.,0.));
#31837=DIRECTION('center_axis',(0.,0.,1.));
#31838=DIRECTION('ref_axis',(1.,0.,0.));
#31839=DIRECTION('center_axis',(0.,0.,1.));
#31840=DIRECTION('ref_axis',(1.,0.,0.));
#31841=DIRECTION('',(0.,0.,-1.));
#31842=DIRECTION('center_axis',(0.,0.,-1.));
#31843=DIRECTION('ref_axis',(1.,0.,0.));
#31844=DIRECTION('',(0.,0.,1.));
#31845=DIRECTION('center_axis',(0.,0.,1.));
#31846=DIRECTION('ref_axis',(1.,0.,0.));
#31847=DIRECTION('center_axis',(-0.259973473447872,-0.96561575852067,0.));
#31848=DIRECTION('ref_axis',(0.96561575852067,-0.259973473447872,0.));
#31849=DIRECTION('',(0.96561575852067,-0.259973473447872,0.));
#31850=DIRECTION('',(0.,0.,1.));
#31851=DIRECTION('center_axis',(-0.259973473447872,0.96561575852067,0.));
#31852=DIRECTION('ref_axis',(-0.96561575852067,-0.259973473447872,0.));
#31853=DIRECTION('',(-0.96561575852067,-0.259973473447872,0.));
#31854=DIRECTION('center_axis',(0.,0.,1.));
#31855=DIRECTION('ref_axis',(1.,0.,0.));
#31856=DIRECTION('center_axis',(0.,0.,-1.));
#31857=DIRECTION('ref_axis',(1.,0.,0.));
#31858=DIRECTION('center_axis',(0.,0.,1.));
#31859=DIRECTION('ref_axis',(1.,0.,0.));
#31860=DIRECTION('',(-0.707106781186548,-8.65956056235493E-17,-0.707106781186548));
#31861=DIRECTION('center_axis',(0.,0.,1.));
#31862=DIRECTION('ref_axis',(1.,0.,0.));
#31863=DIRECTION('',(-0.842487928864452,-1.03175014540413E-16,0.538715221353255));
#31864=DIRECTION('center_axis',(0.,0.,-1.));
#31865=DIRECTION('ref_axis',(1.,0.,0.));
#31866=DIRECTION('center_axis',(0.5,0.866025403784439,0.));
#31867=DIRECTION('ref_axis',(0.866025403784439,-0.5,0.));
#31868=DIRECTION('',(0.866025403784439,-0.5,0.));
#31869=DIRECTION('',(0.,0.,-1.));
#31870=DIRECTION('',(0.866025403784439,-0.5,0.));
#31871=DIRECTION('',(0.,0.,-1.));
#31872=DIRECTION('center_axis',(-0.5,0.866025403784439,0.));
#31873=DIRECTION('ref_axis',(0.866025403784439,0.5,0.));
#31874=DIRECTION('',(0.866025403784439,0.5,0.));
#31875=DIRECTION('',(0.,0.,-1.));
#31876=DIRECTION('',(0.866025403784439,0.5,0.));
#31877=DIRECTION('center_axis',(-1.,-1.60246890531964E-16,0.));
#31878=DIRECTION('ref_axis',(-1.60246890531964E-16,1.,0.));
#31879=DIRECTION('',(-1.60246890531964E-16,1.,0.));
#31880=DIRECTION('',(0.,0.,-1.));
#31881=DIRECTION('',(-1.60246890531964E-16,1.,0.));
#31882=DIRECTION('center_axis',(-0.5,-0.866025403784439,0.));
#31883=DIRECTION('ref_axis',(-0.866025403784439,0.5,0.));
#31884=DIRECTION('',(-0.866025403784439,0.5,0.));
#31885=DIRECTION('',(0.,0.,-1.));
#31886=DIRECTION('',(-0.866025403784439,0.5,0.));
#31887=DIRECTION('center_axis',(0.5,-0.866025403784439,0.));
#31888=DIRECTION('ref_axis',(-0.866025403784439,-0.5,0.));
#31889=DIRECTION('',(-0.866025403784439,-0.5,0.));
#31890=DIRECTION('',(0.,0.,-1.));
#31891=DIRECTION('',(-0.866025403784439,-0.5,0.));
#31892=DIRECTION('center_axis',(1.,-3.20493781063927E-16,0.));
#31893=DIRECTION('ref_axis',(-3.20493781063927E-16,-1.,0.));
#31894=DIRECTION('',(-3.20493781063927E-16,-1.,0.));
#31895=DIRECTION('',(-3.20493781063927E-16,-1.,0.));
#31896=DIRECTION('center_axis',(0.,0.,-1.));
#31897=DIRECTION('ref_axis',(-1.,0.,0.));
#31898=DIRECTION('center_axis',(0.,0.,-1.));
#31899=DIRECTION('ref_axis',(-1.,0.,0.));
#31900=DIRECTION('center_axis',(0.,0.,1.));
#31901=DIRECTION('ref_axis',(1.,0.,0.));
#31902=DIRECTION('center_axis',(0.,0.,1.));
#31903=DIRECTION('ref_axis',(1.,0.,0.));
#31904=DIRECTION('',(0.707106781186547,8.65956056235493E-17,-0.707106781186548));
#31905=DIRECTION('center_axis',(0.,0.,1.));
#31906=DIRECTION('ref_axis',(1.,0.,0.));
#31907=DIRECTION('center_axis',(0.,0.,1.));
#31908=DIRECTION('ref_axis',(1.,0.,0.));
#31909=DIRECTION('center_axis',(0.,0.,1.));
#31910=DIRECTION('ref_axis',(1.,0.,0.));
#31911=DIRECTION('center_axis',(0.,0.,1.));
#31912=DIRECTION('ref_axis',(1.,0.,0.));
#31913=DIRECTION('',(0.707106781186548,8.65956056235494E-17,-0.707106781186547));
#31914=DIRECTION('center_axis',(0.,0.,-1.));
#31915=DIRECTION('ref_axis',(-1.,0.,0.));
#31916=DIRECTION('center_axis',(0.,0.,1.));
#31917=DIRECTION('ref_axis',(1.,0.,0.));
#31918=DIRECTION('axis',(0.,0.,1.));
#31919=DIRECTION('refdir',(1.,0.,0.));
#31920=DIRECTION('center_axis',(0.,0.,1.));
#31921=DIRECTION('ref_axis',(1.,0.,0.));
#31922=DIRECTION('',(0.,0.,-1.));
#31923=DIRECTION('center_axis',(0.,0.,-1.));
#31924=DIRECTION('ref_axis',(1.,0.,0.));
#31925=DIRECTION('',(0.,0.,-1.));
#31926=DIRECTION('center_axis',(0.,0.,1.));
#31927=DIRECTION('ref_axis',(1.,0.,0.));
#31928=DIRECTION('center_axis',(0.,0.,-1.));
#31929=DIRECTION('ref_axis',(1.,0.,0.));
#31930=DIRECTION('center_axis',(0.,0.,1.));
#31931=DIRECTION('ref_axis',(1.,0.,0.));
#31932=DIRECTION('',(0.,0.,-1.));
#31933=DIRECTION('center_axis',(0.,0.,1.));
#31934=DIRECTION('ref_axis',(1.,0.,0.));
#31935=DIRECTION('',(0.,0.,-1.));
#31936=DIRECTION('center_axis',(0.,0.,1.));
#31937=DIRECTION('ref_axis',(1.,0.,0.));
#31938=DIRECTION('',(0.,0.,-1.));
#31939=DIRECTION('center_axis',(0.,0.,1.));
#31940=DIRECTION('ref_axis',(1.,0.,0.));
#31941=DIRECTION('',(0.,0.,-1.));
#31942=DIRECTION('center_axis',(0.,0.,1.));
#31943=DIRECTION('ref_axis',(1.,0.,0.));
#31944=DIRECTION('',(0.,0.,-1.));
#31945=DIRECTION('center_axis',(0.,0.,1.));
#31946=DIRECTION('ref_axis',(1.,0.,0.));
#31947=DIRECTION('',(0.,0.,-1.));
#31948=DIRECTION('center_axis',(0.,0.,1.));
#31949=DIRECTION('ref_axis',(1.,0.,0.));
#31950=DIRECTION('',(0.,0.,-1.));
#31951=DIRECTION('center_axis',(0.,0.,1.));
#31952=DIRECTION('ref_axis',(1.,0.,0.));
#31953=DIRECTION('',(0.,0.,-1.));
#31954=DIRECTION('center_axis',(0.,0.,1.));
#31955=DIRECTION('ref_axis',(1.,0.,0.));
#31956=DIRECTION('',(0.,0.,-1.));
#31957=DIRECTION('center_axis',(0.,0.,1.));
#31958=DIRECTION('ref_axis',(1.,0.,0.));
#31959=DIRECTION('',(0.,0.,-1.));
#31960=DIRECTION('center_axis',(0.,0.,1.));
#31961=DIRECTION('ref_axis',(1.,0.,0.));
#31962=DIRECTION('',(0.,0.,-1.));
#31963=DIRECTION('center_axis',(0.,0.,1.));
#31964=DIRECTION('ref_axis',(1.,0.,0.));
#31965=DIRECTION('',(0.,0.,-1.));
#31966=DIRECTION('center_axis',(0.,0.,1.));
#31967=DIRECTION('ref_axis',(1.,0.,0.));
#31968=DIRECTION('',(0.,0.,-1.));
#31969=DIRECTION('center_axis',(0.,0.,1.));
#31970=DIRECTION('ref_axis',(1.,0.,0.));
#31971=DIRECTION('',(0.,0.,-1.));
#31972=DIRECTION('center_axis',(0.,0.,1.));
#31973=DIRECTION('ref_axis',(1.,0.,0.));
#31974=DIRECTION('',(0.,0.,-1.));
#31975=DIRECTION('center_axis',(0.,0.,1.));
#31976=DIRECTION('ref_axis',(1.,0.,0.));
#31977=DIRECTION('',(0.,0.,-1.));
#31978=DIRECTION('center_axis',(0.,0.,1.));
#31979=DIRECTION('ref_axis',(1.,0.,0.));
#31980=DIRECTION('',(0.,0.,-1.));
#31981=DIRECTION('center_axis',(0.,0.,1.));
#31982=DIRECTION('ref_axis',(1.,0.,0.));
#31983=DIRECTION('',(0.,0.,-1.));
#31984=DIRECTION('center_axis',(0.,0.,1.));
#31985=DIRECTION('ref_axis',(1.,0.,0.));
#31986=DIRECTION('',(0.,0.,-1.));
#31987=DIRECTION('center_axis',(0.,0.,1.));
#31988=DIRECTION('ref_axis',(1.,0.,0.));
#31989=DIRECTION('',(0.,0.,-1.));
#31990=DIRECTION('center_axis',(0.,0.,1.));
#31991=DIRECTION('ref_axis',(1.,0.,0.));
#31992=DIRECTION('',(0.,0.,-1.));
#31993=DIRECTION('center_axis',(0.,0.,1.));
#31994=DIRECTION('ref_axis',(1.,0.,0.));
#31995=DIRECTION('',(0.,0.,-1.));
#31996=DIRECTION('center_axis',(0.,0.,1.));
#31997=DIRECTION('ref_axis',(-0.0038548301263327,-0.999992570114747,0.));
#31998=DIRECTION('',(0.,0.,1.));
#31999=DIRECTION('center_axis',(0.,0.,1.));
#32000=DIRECTION('ref_axis',(1.,-8.97481250249747E-15,0.));
#32001=DIRECTION('center_axis',(0.,0.,1.));
#32002=DIRECTION('ref_axis',(1.,-8.97481250249747E-15,0.));
#32003=DIRECTION('',(0.,0.,1.));
#32004=DIRECTION('center_axis',(0.,0.,1.));
#32005=DIRECTION('ref_axis',(1.,-8.97481250249747E-15,0.));
#32006=DIRECTION('',(0.,0.,1.));
#32007=DIRECTION('center_axis',(0.,0.,1.));
#32008=DIRECTION('ref_axis',(1.,-8.97481250249747E-15,0.));
#32009=DIRECTION('',(0.,0.,1.));
#32010=DIRECTION('center_axis',(0.,0.,1.));
#32011=DIRECTION('ref_axis',(1.,-8.97481250249747E-15,0.));
#32012=DIRECTION('',(0.,0.,1.));
#32013=DIRECTION('center_axis',(0.,0.,1.));
#32014=DIRECTION('ref_axis',(1.,-8.97481250249747E-15,0.));
#32015=DIRECTION('',(0.,0.,1.));
#32016=DIRECTION('center_axis',(0.,0.,1.));
#32017=DIRECTION('ref_axis',(1.,-8.97481250249747E-15,0.));
#32018=DIRECTION('',(0.,0.,1.));
#32019=DIRECTION('center_axis',(0.,0.,1.));
#32020=DIRECTION('ref_axis',(1.,-8.97481250249747E-15,0.));
#32021=DIRECTION('',(0.,0.,1.));
#32022=DIRECTION('center_axis',(0.,0.,1.));
#32023=DIRECTION('ref_axis',(1.,-8.97481250249747E-15,0.));
#32024=DIRECTION('',(0.,0.,1.));
#32025=DIRECTION('center_axis',(0.,0.,1.));
#32026=DIRECTION('ref_axis',(1.,-8.97481250249747E-15,0.));
#32027=DIRECTION('',(0.,0.,1.));
#32028=DIRECTION('center_axis',(0.,0.,1.));
#32029=DIRECTION('ref_axis',(1.,-8.97481250249747E-15,0.));
#32030=DIRECTION('',(0.,0.,1.));
#32031=DIRECTION('center_axis',(0.,0.,1.));
#32032=DIRECTION('ref_axis',(1.,-8.97481250249747E-15,0.));
#32033=DIRECTION('',(0.,0.,1.));
#32034=DIRECTION('center_axis',(0.,0.,1.));
#32035=DIRECTION('ref_axis',(1.,-8.97481250249747E-15,0.));
#32036=DIRECTION('',(0.,0.,1.));
#32037=DIRECTION('center_axis',(0.,0.,1.));
#32038=DIRECTION('ref_axis',(1.,-8.97481250249747E-15,0.));
#32039=DIRECTION('',(0.,0.,1.));
#32040=DIRECTION('center_axis',(0.,0.,1.));
#32041=DIRECTION('ref_axis',(1.,-8.97481250249747E-15,0.));
#32042=DIRECTION('',(0.,0.,1.));
#32043=DIRECTION('center_axis',(0.,0.,1.));
#32044=DIRECTION('ref_axis',(1.,-8.97481250249747E-15,0.));
#32045=DIRECTION('',(0.,0.,1.));
#32046=DIRECTION('center_axis',(0.,0.,1.));
#32047=DIRECTION('ref_axis',(1.,-8.97481250249747E-15,0.));
#32048=DIRECTION('',(0.,0.,1.));
#32049=DIRECTION('center_axis',(0.,0.,1.));
#32050=DIRECTION('ref_axis',(1.,-8.97481250249747E-15,0.));
#32051=DIRECTION('',(0.,0.,1.));
#32052=DIRECTION('center_axis',(0.,0.,1.));
#32053=DIRECTION('ref_axis',(1.,-8.97481250249747E-15,0.));
#32054=DIRECTION('',(0.,0.,1.));
#32055=DIRECTION('center_axis',(0.,0.,1.));
#32056=DIRECTION('ref_axis',(1.,-8.97481250249747E-15,0.));
#32057=DIRECTION('',(0.,0.,1.));
#32058=DIRECTION('center_axis',(0.,0.,1.));
#32059=DIRECTION('ref_axis',(1.,-8.97481250249747E-15,0.));
#32060=DIRECTION('',(0.,0.,1.));
#32061=DIRECTION('center_axis',(0.,0.,1.));
#32062=DIRECTION('ref_axis',(1.,-8.97481250249747E-15,0.));
#32063=DIRECTION('',(0.,0.,1.));
#32064=DIRECTION('center_axis',(0.,0.,1.));
#32065=DIRECTION('ref_axis',(1.,-8.97481250249747E-15,0.));
#32066=DIRECTION('',(0.,0.,1.));
#32067=DIRECTION('center_axis',(0.,0.,1.));
#32068=DIRECTION('ref_axis',(1.,-8.97481250249747E-15,0.));
#32069=DIRECTION('',(0.,0.,1.));
#32070=DIRECTION('center_axis',(0.,0.,-1.));
#32071=DIRECTION('ref_axis',(1.,-8.97481250249747E-15,0.));
#32072=DIRECTION('center_axis',(0.,0.,1.));
#32073=DIRECTION('ref_axis',(1.,0.,0.));
#32074=DIRECTION('center_axis',(0.,0.,1.));
#32075=DIRECTION('ref_axis',(1.,0.,0.));
#32076=DIRECTION('center_axis',(0.,0.,1.));
#32077=DIRECTION('ref_axis',(1.,0.,0.));
#32078=DIRECTION('center_axis',(0.,0.,1.));
#32079=DIRECTION('ref_axis',(1.,0.,0.));
#32080=DIRECTION('center_axis',(0.,0.,-1.));
#32081=DIRECTION('ref_axis',(1.,-8.97481250249747E-15,0.));
#32082=DIRECTION('center_axis',(0.,0.,1.));
#32083=DIRECTION('ref_axis',(-0.952277678384196,0.305233063823706,0.));
#32084=DIRECTION('center_axis',(0.,0.,1.));
#32085=DIRECTION('ref_axis',(0.984807753012208,-0.17364817766693,0.));
#32086=DIRECTION('center_axis',(0.,0.,-1.));
#32087=DIRECTION('ref_axis',(1.,0.,0.));
#32088=DIRECTION('',(-0.996089805327885,-0.0883464754353932,0.));
#32089=DIRECTION('',(0.905801965515954,-0.423701309022563,0.));
#32090=DIRECTION('center_axis',(-0.423701309022563,-0.905801965515954,0.));
#32091=DIRECTION('ref_axis',(0.905801965515954,-0.423701309022563,0.));
#32092=DIRECTION('',(0.,0.,1.));
#32093=DIRECTION('',(0.,0.,1.));
#32094=DIRECTION('center_axis',(-0.0883464754353932,0.996089805327885,0.));
#32095=DIRECTION('ref_axis',(-0.996089805327885,-0.0883464754353932,0.));
#32096=DIRECTION('',(0.,0.,-1.));
#32097=DIRECTION('center_axis',(0.,0.,1.));
#32098=DIRECTION('ref_axis',(0.939692620785908,-0.342020143325669,0.));
#32099=DIRECTION('center_axis',(0.,0.,-1.));
#32100=DIRECTION('ref_axis',(1.,0.,0.));
#32101=DIRECTION('',(-0.996298167445974,0.0859648855277176,0.));
#32102=DIRECTION('',(0.818465838146947,-0.574555194725812,0.));
#32103=DIRECTION('center_axis',(-0.574555194725812,-0.818465838146947,0.));
#32104=DIRECTION('ref_axis',(0.818465838146947,-0.574555194725812,0.));
#32105=DIRECTION('',(0.,0.,1.));
#32106=DIRECTION('',(0.,0.,1.));
#32107=DIRECTION('center_axis',(0.0859648855277176,0.996298167445974,0.));
#32108=DIRECTION('ref_axis',(-0.996298167445974,0.0859648855277176,0.));
#32109=DIRECTION('',(0.,0.,-1.));
#32110=DIRECTION('center_axis',(0.,0.,1.));
#32111=DIRECTION('ref_axis',(0.866025403784438,-0.5,0.));
#32112=DIRECTION('center_axis',(0.,0.,-1.));
#32113=DIRECTION('ref_axis',(1.,0.,0.));
#32114=DIRECTION('',(-0.966234513897416,0.257664246944399,0.));
#32115=DIRECTION('',(0.706261040449543,-0.707951511576272,0.));
#32116=DIRECTION('center_axis',(-0.707951511576272,-0.706261040449543,0.));
#32117=DIRECTION('ref_axis',(0.706261040449543,-0.707951511576272,0.));
#32118=DIRECTION('',(0.,0.,1.));
#32119=DIRECTION('',(0.,0.,1.));
#32120=DIRECTION('center_axis',(0.257664246944399,0.966234513897416,0.));
#32121=DIRECTION('ref_axis',(-0.966234513897416,0.257664246944399,0.));
#32122=DIRECTION('',(0.,0.,-1.));
#32123=DIRECTION('center_axis',(0.,0.,1.));
#32124=DIRECTION('ref_axis',(0.766044443118978,-0.64278760968654,0.));
#32125=DIRECTION('center_axis',(0.,0.,-1.));
#32126=DIRECTION('ref_axis',(1.,0.,0.));
#32127=DIRECTION('',(-0.906812313582341,0.421534610602074,0.));
#32128=DIRECTION('',(0.572596858423411,-0.819837079988238,0.));
#32129=DIRECTION('center_axis',(-0.819837079988238,-0.572596858423411,0.));
#32130=DIRECTION('ref_axis',(0.572596858423411,-0.819837079988238,0.));
#32131=DIRECTION('',(0.,0.,1.));
#32132=DIRECTION('',(0.,0.,1.));
#32133=DIRECTION('center_axis',(0.421534610602074,0.906812313582341,0.));
#32134=DIRECTION('ref_axis',(-0.906812313582341,0.421534610602074,0.));
#32135=DIRECTION('',(0.,0.,-1.));
#32136=DIRECTION('center_axis',(0.,0.,1.));
#32137=DIRECTION('ref_axis',(0.642787609686539,-0.766044443118978,0.));
#32138=DIRECTION('center_axis',(0.,0.,-1.));
#32139=DIRECTION('ref_axis',(1.,0.,0.));
#32140=DIRECTION('',(-0.819837079988238,0.572596858423411,0.));
#32141=DIRECTION('',(0.421534610602074,-0.906812313582341,0.));
#32142=DIRECTION('center_axis',(-0.906812313582341,-0.421534610602074,0.));
#32143=DIRECTION('ref_axis',(0.421534610602074,-0.906812313582341,0.));
#32144=DIRECTION('',(0.,0.,1.));
#32145=DIRECTION('',(0.,0.,1.));
#32146=DIRECTION('center_axis',(0.572596858423411,0.819837079988238,0.));
#32147=DIRECTION('ref_axis',(-0.819837079988238,0.572596858423411,0.));
#32148=DIRECTION('',(0.,0.,-1.));
#32149=DIRECTION('center_axis',(0.,0.,1.));
#32150=DIRECTION('ref_axis',(0.5,-0.866025403784438,0.));
#32151=DIRECTION('center_axis',(0.,0.,-1.));
#32152=DIRECTION('ref_axis',(1.,0.,0.));
#32153=DIRECTION('',(-0.707951511576272,0.706261040449544,0.));
#32154=DIRECTION('',(0.257664246944398,-0.966234513897416,0.));
#32155=DIRECTION('center_axis',(-0.966234513897416,-0.257664246944398,0.));
#32156=DIRECTION('ref_axis',(0.257664246944398,-0.966234513897416,0.));
#32157=DIRECTION('',(0.,0.,1.));
#32158=DIRECTION('',(0.,0.,1.));
#32159=DIRECTION('center_axis',(0.706261040449544,0.707951511576272,0.));
#32160=DIRECTION('ref_axis',(-0.707951511576272,0.706261040449544,0.));
#32161=DIRECTION('',(0.,0.,-1.));
#32162=DIRECTION('center_axis',(0.,0.,1.));
#32163=DIRECTION('ref_axis',(0.342020143325668,-0.939692620785909,0.));
#32164=DIRECTION('center_axis',(0.,0.,-1.));
#32165=DIRECTION('ref_axis',(1.,0.,0.));
#32166=DIRECTION('',(-0.57455519472581,0.818465838146948,0.));
#32167=DIRECTION('',(0.0859648855277162,-0.996298167445974,0.));
#32168=DIRECTION('center_axis',(-0.996298167445974,-0.0859648855277162,
0.));
#32169=DIRECTION('ref_axis',(0.0859648855277162,-0.996298167445974,0.));
#32170=DIRECTION('',(0.,0.,1.));
#32171=DIRECTION('',(0.,0.,1.));
#32172=DIRECTION('center_axis',(0.818465838146948,0.57455519472581,0.));
#32173=DIRECTION('ref_axis',(-0.57455519472581,0.818465838146948,0.));
#32174=DIRECTION('',(0.,0.,-1.));
#32175=DIRECTION('center_axis',(0.,0.,1.));
#32176=DIRECTION('ref_axis',(0.17364817766693,-0.984807753012208,0.));
#32177=DIRECTION('center_axis',(0.,0.,-1.));
#32178=DIRECTION('ref_axis',(1.,0.,0.));
#32179=DIRECTION('',(-0.423701309022563,0.905801965515955,0.));
#32180=DIRECTION('',(-0.0883464754353936,-0.996089805327885,0.));
#32181=DIRECTION('center_axis',(-0.996089805327885,0.0883464754353937,0.));
#32182=DIRECTION('ref_axis',(-0.0883464754353937,-0.996089805327885,0.));
#32183=DIRECTION('',(0.,0.,1.));
#32184=DIRECTION('',(0.,0.,1.));
#32185=DIRECTION('center_axis',(0.905801965515955,0.423701309022563,0.));
#32186=DIRECTION('ref_axis',(-0.423701309022563,0.905801965515955,0.));
#32187=DIRECTION('',(0.,0.,-1.));
#32188=DIRECTION('center_axis',(0.,0.,1.));
#32189=DIRECTION('ref_axis',(-1.94289029309402E-16,-1.,0.));
#32190=DIRECTION('center_axis',(0.,0.,-1.));
#32191=DIRECTION('ref_axis',(1.,0.,0.));
#32192=DIRECTION('',(-0.259973473447872,0.96561575852067,0.));
#32193=DIRECTION('',(-0.259973473447873,-0.96561575852067,0.));
#32194=DIRECTION('center_axis',(-0.96561575852067,0.259973473447873,0.));
#32195=DIRECTION('ref_axis',(-0.259973473447873,-0.96561575852067,0.));
#32196=DIRECTION('',(0.,0.,1.));
#32197=DIRECTION('',(0.,0.,1.));
#32198=DIRECTION('center_axis',(0.96561575852067,0.259973473447872,0.));
#32199=DIRECTION('ref_axis',(-0.259973473447872,0.96561575852067,0.));
#32200=DIRECTION('',(0.,0.,-1.));
#32201=DIRECTION('center_axis',(0.,0.,1.));
#32202=DIRECTION('ref_axis',(-0.17364817766693,-0.984807753012208,0.));
#32203=DIRECTION('center_axis',(0.,0.,-1.));
#32204=DIRECTION('ref_axis',(1.,0.,0.));
#32205=DIRECTION('',(-0.0883464754353933,0.996089805327885,0.));
#32206=DIRECTION('',(-0.423701309022563,-0.905801965515955,0.));
#32207=DIRECTION('center_axis',(-0.905801965515955,0.423701309022563,0.));
#32208=DIRECTION('ref_axis',(-0.423701309022563,-0.905801965515955,0.));
#32209=DIRECTION('',(0.,0.,1.));
#32210=DIRECTION('',(0.,0.,1.));
#32211=DIRECTION('center_axis',(0.996089805327885,0.0883464754353932,0.));
#32212=DIRECTION('ref_axis',(-0.0883464754353932,0.996089805327885,0.));
#32213=DIRECTION('',(0.,0.,-1.));
#32214=DIRECTION('center_axis',(0.,0.,1.));
#32215=DIRECTION('ref_axis',(-0.342020143325669,-0.939692620785908,0.));
#32216=DIRECTION('center_axis',(0.,0.,-1.));
#32217=DIRECTION('ref_axis',(1.,0.,0.));
#32218=DIRECTION('',(0.0859648855277175,0.996298167445974,0.));
#32219=DIRECTION('',(-0.574555194725811,-0.818465838146947,0.));
#32220=DIRECTION('center_axis',(-0.818465838146947,0.574555194725811,0.));
#32221=DIRECTION('ref_axis',(-0.574555194725811,-0.818465838146947,0.));
#32222=DIRECTION('',(0.,0.,1.));
#32223=DIRECTION('',(0.,0.,1.));
#32224=DIRECTION('center_axis',(0.996298167445974,-0.0859648855277175,0.));
#32225=DIRECTION('ref_axis',(0.0859648855277175,0.996298167445974,0.));
#32226=DIRECTION('',(0.,0.,-1.));
#32227=DIRECTION('center_axis',(0.,0.,1.));
#32228=DIRECTION('ref_axis',(-0.5,-0.866025403784438,0.));
#32229=DIRECTION('center_axis',(0.,0.,-1.));
#32230=DIRECTION('ref_axis',(1.,0.,0.));
#32231=DIRECTION('',(0.257664246944399,0.966234513897416,0.));
#32232=DIRECTION('',(-0.707951511576272,-0.706261040449543,0.));
#32233=DIRECTION('center_axis',(-0.706261040449543,0.707951511576272,0.));
#32234=DIRECTION('ref_axis',(-0.707951511576272,-0.706261040449543,0.));
#32235=DIRECTION('',(0.,0.,1.));
#32236=DIRECTION('',(0.,0.,1.));
#32237=DIRECTION('center_axis',(0.966234513897416,-0.257664246944399,0.));
#32238=DIRECTION('ref_axis',(0.257664246944399,0.966234513897416,0.));
#32239=DIRECTION('',(0.,0.,-1.));
#32240=DIRECTION('center_axis',(0.,0.,1.));
#32241=DIRECTION('ref_axis',(-0.642787609686539,-0.766044443118978,0.));
#32242=DIRECTION('center_axis',(0.,0.,-1.));
#32243=DIRECTION('ref_axis',(1.,0.,0.));
#32244=DIRECTION('',(0.421534610602074,0.906812313582341,0.));
#32245=DIRECTION('',(-0.819837079988238,-0.572596858423411,0.));
#32246=DIRECTION('center_axis',(-0.572596858423411,0.819837079988238,0.));
#32247=DIRECTION('ref_axis',(-0.819837079988238,-0.572596858423411,0.));
#32248=DIRECTION('',(0.,0.,1.));
#32249=DIRECTION('',(0.,0.,1.));
#32250=DIRECTION('center_axis',(0.906812313582341,-0.421534610602074,0.));
#32251=DIRECTION('ref_axis',(0.421534610602074,0.906812313582341,0.));
#32252=DIRECTION('',(0.,0.,-1.));
#32253=DIRECTION('center_axis',(0.,0.,1.));
#32254=DIRECTION('ref_axis',(-0.766044443118978,-0.642787609686539,0.));
#32255=DIRECTION('center_axis',(0.,0.,-1.));
#32256=DIRECTION('ref_axis',(1.,0.,0.));
#32257=DIRECTION('',(0.572596858423411,0.819837079988238,0.));
#32258=DIRECTION('',(-0.906812313582341,-0.421534610602074,0.));
#32259=DIRECTION('center_axis',(-0.421534610602074,0.906812313582341,0.));
#32260=DIRECTION('ref_axis',(-0.906812313582341,-0.421534610602074,0.));
#32261=DIRECTION('',(0.,0.,1.));
#32262=DIRECTION('',(0.,0.,1.));
#32263=DIRECTION('center_axis',(0.819837079988238,-0.572596858423411,0.));
#32264=DIRECTION('ref_axis',(0.572596858423411,0.819837079988238,0.));
#32265=DIRECTION('',(0.,0.,-1.));
#32266=DIRECTION('center_axis',(0.,0.,1.));
#32267=DIRECTION('ref_axis',(-0.866025403784439,-0.5,0.));
#32268=DIRECTION('center_axis',(0.,0.,-1.));
#32269=DIRECTION('ref_axis',(1.,0.,0.));
#32270=DIRECTION('',(0.706261040449544,0.707951511576271,0.));
#32271=DIRECTION('',(-0.966234513897416,-0.257664246944398,0.));
#32272=DIRECTION('center_axis',(-0.257664246944398,0.966234513897416,0.));
#32273=DIRECTION('ref_axis',(-0.966234513897416,-0.257664246944398,0.));
#32274=DIRECTION('',(0.,0.,1.));
#32275=DIRECTION('',(0.,0.,1.));
#32276=DIRECTION('center_axis',(0.707951511576271,-0.706261040449544,0.));
#32277=DIRECTION('ref_axis',(0.706261040449544,0.707951511576271,0.));
#32278=DIRECTION('',(0.,0.,-1.));
#32279=DIRECTION('center_axis',(0.,0.,1.));
#32280=DIRECTION('ref_axis',(-0.939692620785909,-0.342020143325669,0.));
#32281=DIRECTION('center_axis',(0.,0.,-1.));
#32282=DIRECTION('ref_axis',(1.,0.,0.));
#32283=DIRECTION('',(0.818465838146948,0.574555194725811,0.));
#32284=DIRECTION('',(-0.996298167445974,-0.0859648855277167,0.));
#32285=DIRECTION('center_axis',(-0.0859648855277167,0.996298167445974,0.));
#32286=DIRECTION('ref_axis',(-0.996298167445974,-0.0859648855277167,0.));
#32287=DIRECTION('',(0.,0.,1.));
#32288=DIRECTION('',(0.,0.,1.));
#32289=DIRECTION('center_axis',(0.574555194725811,-0.818465838146948,0.));
#32290=DIRECTION('ref_axis',(0.818465838146948,0.574555194725811,0.));
#32291=DIRECTION('',(0.,0.,-1.));
#32292=DIRECTION('center_axis',(0.,0.,1.));
#32293=DIRECTION('ref_axis',(-0.984807753012208,-0.17364817766693,0.));
#32294=DIRECTION('center_axis',(0.,0.,-1.));
#32295=DIRECTION('ref_axis',(1.,0.,0.));
#32296=DIRECTION('',(0.905801965515955,0.423701309022563,0.));
#32297=DIRECTION('',(-0.996089805327885,0.0883464754353936,0.));
#32298=DIRECTION('center_axis',(0.0883464754353936,0.996089805327885,0.));
#32299=DIRECTION('ref_axis',(-0.996089805327885,0.0883464754353936,0.));
#32300=DIRECTION('',(0.,0.,1.));
#32301=DIRECTION('',(0.,0.,1.));
#32302=DIRECTION('center_axis',(0.423701309022563,-0.905801965515955,0.));
#32303=DIRECTION('ref_axis',(0.905801965515955,0.423701309022563,0.));
#32304=DIRECTION('',(0.,0.,-1.));
#32305=DIRECTION('center_axis',(0.,0.,1.));
#32306=DIRECTION('ref_axis',(-1.,1.11022302462516E-16,0.));
#32307=DIRECTION('center_axis',(0.,0.,-1.));
#32308=DIRECTION('ref_axis',(1.,0.,0.));
#32309=DIRECTION('',(0.96561575852067,0.259973473447872,0.));
#32310=DIRECTION('',(-0.96561575852067,0.259973473447873,0.));
#32311=DIRECTION('center_axis',(0.,0.,-1.));
#32312=DIRECTION('ref_axis',(1.,0.,0.));
#32313=DIRECTION('center_axis',(0.259973473447873,0.96561575852067,0.));
#32314=DIRECTION('ref_axis',(-0.96561575852067,0.259973473447873,0.));
#32315=DIRECTION('',(0.,0.,1.));
#32316=DIRECTION('',(0.,0.,1.));
#32317=DIRECTION('center_axis',(0.259973473447872,-0.96561575852067,0.));
#32318=DIRECTION('ref_axis',(0.96561575852067,0.259973473447872,0.));
#32319=DIRECTION('',(0.,0.,-1.));
#32320=DIRECTION('center_axis',(0.,0.,1.));
#32321=DIRECTION('ref_axis',(-0.984807753012208,0.173648177666931,0.));
#32322=DIRECTION('center_axis',(0.,0.,-1.));
#32323=DIRECTION('ref_axis',(1.,0.,0.));
#32324=DIRECTION('',(0.996089805327885,0.0883464754353928,0.));
#32325=DIRECTION('',(-0.905801965515954,0.423701309022564,0.));
#32326=DIRECTION('center_axis',(0.423701309022564,0.905801965515954,0.));
#32327=DIRECTION('ref_axis',(-0.905801965515954,0.423701309022564,0.));
#32328=DIRECTION('',(0.,0.,1.));
#32329=DIRECTION('',(0.,0.,1.));
#32330=DIRECTION('center_axis',(0.0883464754353928,-0.996089805327885,0.));
#32331=DIRECTION('ref_axis',(0.996089805327885,0.0883464754353928,0.));
#32332=DIRECTION('',(0.,0.,-1.));
#32333=DIRECTION('center_axis',(0.,0.,1.));
#32334=DIRECTION('ref_axis',(-0.939692620785908,0.342020143325669,0.));
#32335=DIRECTION('center_axis',(0.,0.,-1.));
#32336=DIRECTION('ref_axis',(1.,0.,0.));
#32337=DIRECTION('',(0.996298167445974,-0.085964885527717,0.));
#32338=DIRECTION('',(-0.818465838146948,0.574555194725811,0.));
#32339=DIRECTION('center_axis',(0.574555194725811,0.818465838146948,0.));
#32340=DIRECTION('ref_axis',(-0.818465838146948,0.574555194725811,0.));
#32341=DIRECTION('',(0.,0.,1.));
#32342=DIRECTION('',(0.,0.,1.));
#32343=DIRECTION('center_axis',(-0.085964885527717,-0.996298167445974,0.));
#32344=DIRECTION('ref_axis',(0.996298167445974,-0.085964885527717,0.));
#32345=DIRECTION('',(0.,0.,-1.));
#32346=DIRECTION('center_axis',(0.,0.,1.));
#32347=DIRECTION('ref_axis',(-0.866025403784439,0.5,0.));
#32348=DIRECTION('center_axis',(0.,0.,-1.));
#32349=DIRECTION('ref_axis',(1.,0.,0.));
#32350=DIRECTION('',(0.966234513897416,-0.257664246944398,0.));
#32351=DIRECTION('',(-0.706261040449544,0.707951511576272,0.));
#32352=DIRECTION('center_axis',(0.707951511576272,0.706261040449544,0.));
#32353=DIRECTION('ref_axis',(-0.706261040449544,0.707951511576272,0.));
#32354=DIRECTION('',(0.,0.,1.));
#32355=DIRECTION('',(0.,0.,1.));
#32356=DIRECTION('center_axis',(-0.257664246944398,-0.966234513897416,0.));
#32357=DIRECTION('ref_axis',(0.966234513897416,-0.257664246944398,0.));
#32358=DIRECTION('',(0.,0.,-1.));
#32359=DIRECTION('center_axis',(0.,0.,1.));
#32360=DIRECTION('ref_axis',(-0.766044443118978,0.642787609686539,0.));
#32361=DIRECTION('center_axis',(0.,0.,-1.));
#32362=DIRECTION('ref_axis',(1.,0.,0.));
#32363=DIRECTION('',(0.906812313582341,-0.421534610602074,0.));
#32364=DIRECTION('',(-0.572596858423411,0.819837079988238,0.));
#32365=DIRECTION('center_axis',(0.819837079988238,0.572596858423411,0.));
#32366=DIRECTION('ref_axis',(-0.572596858423411,0.819837079988238,0.));
#32367=DIRECTION('',(0.,0.,1.));
#32368=DIRECTION('',(0.,0.,1.));
#32369=DIRECTION('center_axis',(-0.421534610602074,-0.906812313582341,0.));
#32370=DIRECTION('ref_axis',(0.906812313582341,-0.421534610602074,0.));
#32371=DIRECTION('',(0.,0.,-1.));
#32372=DIRECTION('center_axis',(0.,0.,1.));
#32373=DIRECTION('ref_axis',(-0.642787609686539,0.766044443118978,0.));
#32374=DIRECTION('center_axis',(0.,0.,-1.));
#32375=DIRECTION('ref_axis',(1.,0.,0.));
#32376=DIRECTION('',(0.819837079988238,-0.572596858423411,0.));
#32377=DIRECTION('',(-0.421534610602074,0.906812313582341,0.));
#32378=DIRECTION('center_axis',(0.906812313582341,0.421534610602074,0.));
#32379=DIRECTION('ref_axis',(-0.421534610602074,0.906812313582341,0.));
#32380=DIRECTION('',(0.,0.,1.));
#32381=DIRECTION('',(0.,0.,1.));
#32382=DIRECTION('center_axis',(-0.572596858423411,-0.819837079988238,0.));
#32383=DIRECTION('ref_axis',(0.819837079988238,-0.572596858423411,0.));
#32384=DIRECTION('',(0.,0.,-1.));
#32385=DIRECTION('center_axis',(0.,0.,1.));
#32386=DIRECTION('ref_axis',(-0.5,0.866025403784439,0.));
#32387=DIRECTION('center_axis',(0.,0.,-1.));
#32388=DIRECTION('ref_axis',(1.,0.,0.));
#32389=DIRECTION('',(0.707951511576272,-0.706261040449544,0.));
#32390=DIRECTION('',(-0.257664246944398,0.966234513897416,0.));
#32391=DIRECTION('center_axis',(0.966234513897416,0.257664246944398,0.));
#32392=DIRECTION('ref_axis',(-0.257664246944398,0.966234513897416,0.));
#32393=DIRECTION('',(0.,0.,1.));
#32394=DIRECTION('',(0.,0.,1.));
#32395=DIRECTION('center_axis',(-0.706261040449544,-0.707951511576272,0.));
#32396=DIRECTION('ref_axis',(0.707951511576272,-0.706261040449544,0.));
#32397=DIRECTION('',(0.,0.,-1.));
#32398=DIRECTION('center_axis',(0.,0.,1.));
#32399=DIRECTION('ref_axis',(-0.342020143325669,0.939692620785909,0.));
#32400=DIRECTION('center_axis',(0.,0.,-1.));
#32401=DIRECTION('ref_axis',(1.,0.,0.));
#32402=DIRECTION('',(0.574555194725811,-0.818465838146948,0.));
#32403=DIRECTION('',(-0.0859648855277167,0.996298167445974,0.));
#32404=DIRECTION('center_axis',(0.996298167445974,0.0859648855277167,0.));
#32405=DIRECTION('ref_axis',(-0.0859648855277167,0.996298167445974,0.));
#32406=DIRECTION('',(0.,0.,1.));
#32407=DIRECTION('',(0.,0.,1.));
#32408=DIRECTION('center_axis',(-0.818465838146948,-0.574555194725811,0.));
#32409=DIRECTION('ref_axis',(0.574555194725811,-0.818465838146948,0.));
#32410=DIRECTION('',(0.,0.,-1.));
#32411=DIRECTION('center_axis',(0.,0.,1.));
#32412=DIRECTION('ref_axis',(-0.17364817766693,0.984807753012208,0.));
#32413=DIRECTION('center_axis',(0.,0.,-1.));
#32414=DIRECTION('ref_axis',(1.,0.,0.));
#32415=DIRECTION('',(0.423701309022563,-0.905801965515955,0.));
#32416=DIRECTION('',(0.0883464754353932,0.996089805327885,0.));
#32417=DIRECTION('center_axis',(0.996089805327885,-0.0883464754353932,0.));
#32418=DIRECTION('ref_axis',(0.0883464754353932,0.996089805327885,0.));
#32419=DIRECTION('',(0.,0.,1.));
#32420=DIRECTION('',(0.,0.,1.));
#32421=DIRECTION('center_axis',(-0.905801965515955,-0.423701309022563,0.));
#32422=DIRECTION('ref_axis',(0.423701309022563,-0.905801965515955,0.));
#32423=DIRECTION('',(0.,0.,-1.));
#32424=DIRECTION('center_axis',(0.,0.,1.));
#32425=DIRECTION('ref_axis',(5.55111512312578E-17,1.,0.));
#32426=DIRECTION('center_axis',(0.,0.,-1.));
#32427=DIRECTION('ref_axis',(1.,0.,0.));
#32428=DIRECTION('',(0.259973473447872,-0.96561575852067,0.));
#32429=DIRECTION('',(0.259973473447872,0.96561575852067,0.));
#32430=DIRECTION('center_axis',(0.96561575852067,-0.259973473447873,0.));
#32431=DIRECTION('ref_axis',(0.259973473447873,0.96561575852067,0.));
#32432=DIRECTION('',(0.,0.,1.));
#32433=DIRECTION('',(0.,0.,1.));
#32434=DIRECTION('center_axis',(-0.96561575852067,-0.259973473447872,0.));
#32435=DIRECTION('ref_axis',(0.259973473447872,-0.96561575852067,0.));
#32436=DIRECTION('',(0.,0.,-1.));
#32437=DIRECTION('center_axis',(0.,0.,1.));
#32438=DIRECTION('ref_axis',(0.17364817766693,0.984807753012208,0.));
#32439=DIRECTION('center_axis',(0.,0.,-1.));
#32440=DIRECTION('ref_axis',(1.,0.,0.));
#32441=DIRECTION('',(0.0883464754353931,-0.996089805327885,0.));
#32442=DIRECTION('',(0.423701309022563,0.905801965515954,0.));
#32443=DIRECTION('center_axis',(0.905801965515954,-0.423701309022563,0.));
#32444=DIRECTION('ref_axis',(0.423701309022563,0.905801965515954,0.));
#32445=DIRECTION('',(0.,0.,1.));
#32446=DIRECTION('',(0.,0.,1.));
#32447=DIRECTION('center_axis',(-0.996089805327885,-0.0883464754353932,
0.));
#32448=DIRECTION('ref_axis',(0.0883464754353932,-0.996089805327885,0.));
#32449=DIRECTION('',(0.,0.,-1.));
#32450=DIRECTION('center_axis',(0.,0.,1.));
#32451=DIRECTION('ref_axis',(0.342020143325669,0.939692620785908,0.));
#32452=DIRECTION('center_axis',(0.,0.,-1.));
#32453=DIRECTION('ref_axis',(1.,0.,0.));
#32454=DIRECTION('',(-0.085964885527717,-0.996298167445974,0.));
#32455=DIRECTION('',(0.574555194725811,0.818465838146948,0.));
#32456=DIRECTION('center_axis',(0.818465838146948,-0.574555194725811,0.));
#32457=DIRECTION('ref_axis',(0.574555194725811,0.818465838146948,0.));
#32458=DIRECTION('',(0.,0.,1.));
#32459=DIRECTION('',(0.,0.,1.));
#32460=DIRECTION('center_axis',(-0.996298167445974,0.085964885527717,0.));
#32461=DIRECTION('ref_axis',(-0.085964885527717,-0.996298167445974,0.));
#32462=DIRECTION('',(0.,0.,-1.));
#32463=DIRECTION('center_axis',(0.,0.,1.));
#32464=DIRECTION('ref_axis',(0.5,0.866025403784439,0.));
#32465=DIRECTION('center_axis',(0.,0.,-1.));
#32466=DIRECTION('ref_axis',(1.,0.,0.));
#32467=DIRECTION('',(-0.257664246944398,-0.966234513897416,0.));
#32468=DIRECTION('',(0.707951511576272,0.706261040449544,0.));
#32469=DIRECTION('center_axis',(0.706261040449544,-0.707951511576272,0.));
#32470=DIRECTION('ref_axis',(0.707951511576272,0.706261040449544,0.));
#32471=DIRECTION('',(0.,0.,1.));
#32472=DIRECTION('',(0.,0.,1.));
#32473=DIRECTION('center_axis',(-0.966234513897416,0.257664246944398,0.));
#32474=DIRECTION('ref_axis',(-0.257664246944398,-0.966234513897416,0.));
#32475=DIRECTION('',(0.,0.,-1.));
#32476=DIRECTION('center_axis',(0.,0.,1.));
#32477=DIRECTION('ref_axis',(0.642787609686539,0.766044443118978,0.));
#32478=DIRECTION('center_axis',(0.,0.,-1.));
#32479=DIRECTION('ref_axis',(1.,0.,0.));
#32480=DIRECTION('',(-0.421534610602074,-0.906812313582341,0.));
#32481=DIRECTION('',(0.819837079988238,0.572596858423411,0.));
#32482=DIRECTION('center_axis',(0.572596858423411,-0.819837079988238,0.));
#32483=DIRECTION('ref_axis',(0.819837079988238,0.572596858423411,0.));
#32484=DIRECTION('',(0.,0.,1.));
#32485=DIRECTION('',(0.,0.,1.));
#32486=DIRECTION('center_axis',(-0.906812313582341,0.421534610602074,0.));
#32487=DIRECTION('ref_axis',(-0.421534610602074,-0.906812313582341,0.));
#32488=DIRECTION('',(0.,0.,-1.));
#32489=DIRECTION('center_axis',(0.,0.,1.));
#32490=DIRECTION('ref_axis',(0.766044443118978,0.642787609686539,0.));
#32491=DIRECTION('center_axis',(0.,0.,-1.));
#32492=DIRECTION('ref_axis',(1.,0.,0.));
#32493=DIRECTION('',(-0.572596858423411,-0.819837079988238,0.));
#32494=DIRECTION('',(0.906812313582341,0.421534610602074,0.));
#32495=DIRECTION('center_axis',(0.421534610602074,-0.906812313582341,0.));
#32496=DIRECTION('ref_axis',(0.906812313582341,0.421534610602074,0.));
#32497=DIRECTION('',(0.,0.,1.));
#32498=DIRECTION('',(0.,0.,1.));
#32499=DIRECTION('center_axis',(-0.819837079988238,0.572596858423411,0.));
#32500=DIRECTION('ref_axis',(-0.572596858423411,-0.819837079988238,0.));
#32501=DIRECTION('',(0.,0.,-1.));
#32502=DIRECTION('center_axis',(0.,0.,1.));
#32503=DIRECTION('ref_axis',(0.866025403784439,0.5,0.));
#32504=DIRECTION('center_axis',(0.,0.,-1.));
#32505=DIRECTION('ref_axis',(1.,0.,0.));
#32506=DIRECTION('',(-0.706261040449544,-0.707951511576272,0.));
#32507=DIRECTION('',(0.966234513897416,0.257664246944398,0.));
#32508=DIRECTION('center_axis',(0.257664246944398,-0.966234513897416,0.));
#32509=DIRECTION('ref_axis',(0.966234513897416,0.257664246944398,0.));
#32510=DIRECTION('',(0.,0.,1.));
#32511=DIRECTION('',(0.,0.,1.));
#32512=DIRECTION('center_axis',(-0.707951511576272,0.706261040449544,0.));
#32513=DIRECTION('ref_axis',(-0.706261040449544,-0.707951511576272,0.));
#32514=DIRECTION('',(0.,0.,-1.));
#32515=DIRECTION('center_axis',(0.,0.,1.));
#32516=DIRECTION('ref_axis',(0.939692620785909,0.342020143325669,0.));
#32517=DIRECTION('center_axis',(0.,0.,-1.));
#32518=DIRECTION('ref_axis',(1.,0.,0.));
#32519=DIRECTION('',(-0.818465838146948,-0.574555194725811,0.));
#32520=DIRECTION('',(0.996298167445974,0.0859648855277167,0.));
#32521=DIRECTION('center_axis',(0.0859648855277167,-0.996298167445974,0.));
#32522=DIRECTION('ref_axis',(0.996298167445974,0.0859648855277167,0.));
#32523=DIRECTION('',(0.,0.,1.));
#32524=DIRECTION('',(0.,0.,1.));
#32525=DIRECTION('center_axis',(-0.574555194725811,0.818465838146948,0.));
#32526=DIRECTION('ref_axis',(-0.818465838146948,-0.574555194725811,0.));
#32527=DIRECTION('',(0.,0.,-1.));
#32528=DIRECTION('center_axis',(0.,0.,1.));
#32529=DIRECTION('ref_axis',(0.984807753012208,0.17364817766693,0.));
#32530=DIRECTION('center_axis',(0.,0.,-1.));
#32531=DIRECTION('ref_axis',(1.,0.,0.));
#32532=DIRECTION('',(-0.905801965515955,-0.423701309022563,0.));
#32533=DIRECTION('',(0.996089805327885,-0.0883464754353932,0.));
#32534=DIRECTION('center_axis',(-0.0883464754353933,-0.996089805327885,
0.));
#32535=DIRECTION('ref_axis',(0.996089805327885,-0.0883464754353933,0.));
#32536=DIRECTION('',(0.,0.,1.));
#32537=DIRECTION('',(0.,0.,1.));
#32538=DIRECTION('center_axis',(-0.423701309022563,0.905801965515955,0.));
#32539=DIRECTION('ref_axis',(-0.905801965515954,-0.423701309022563,0.));
#32540=DIRECTION('',(0.,0.,-1.));
#32541=DIRECTION('center_axis',(0.,0.,1.));
#32542=DIRECTION('ref_axis',(1.,0.,0.));
#32543=DIRECTION('center_axis',(0.,0.,1.));
#32544=DIRECTION('ref_axis',(1.,0.,0.));
#32545=DIRECTION('center_axis',(0.,0.,1.));
#32546=DIRECTION('ref_axis',(1.,0.,0.));
#32547=DIRECTION('center_axis',(0.,0.,1.));
#32548=DIRECTION('ref_axis',(1.,0.,0.));
#32549=DIRECTION('center_axis',(0.,0.,1.));
#32550=DIRECTION('ref_axis',(1.,0.,0.));
#32551=DIRECTION('center_axis',(0.,0.,1.));
#32552=DIRECTION('ref_axis',(1.,0.,0.));
#32553=DIRECTION('center_axis',(0.,0.,1.));
#32554=DIRECTION('ref_axis',(1.,0.,0.));
#32555=DIRECTION('center_axis',(0.,0.,1.));
#32556=DIRECTION('ref_axis',(1.,0.,0.));
#32557=DIRECTION('center_axis',(0.,0.,1.));
#32558=DIRECTION('ref_axis',(1.,0.,0.));
#32559=DIRECTION('center_axis',(0.,0.,1.));
#32560=DIRECTION('ref_axis',(1.,0.,0.));
#32561=DIRECTION('center_axis',(0.,0.,1.));
#32562=DIRECTION('ref_axis',(1.,0.,0.));
#32563=DIRECTION('center_axis',(0.,0.,1.));
#32564=DIRECTION('ref_axis',(1.,0.,0.));
#32565=DIRECTION('center_axis',(0.,0.,1.));
#32566=DIRECTION('ref_axis',(1.,0.,0.));
#32567=DIRECTION('center_axis',(0.,0.,1.));
#32568=DIRECTION('ref_axis',(1.,0.,0.));
#32569=DIRECTION('center_axis',(0.,0.,1.));
#32570=DIRECTION('ref_axis',(1.,0.,0.));
#32571=DIRECTION('center_axis',(0.,0.,1.));
#32572=DIRECTION('ref_axis',(1.,0.,0.));
#32573=DIRECTION('center_axis',(0.,0.,1.));
#32574=DIRECTION('ref_axis',(1.,0.,0.));
#32575=DIRECTION('center_axis',(0.,0.,1.));
#32576=DIRECTION('ref_axis',(1.,0.,0.));
#32577=DIRECTION('',(0.,0.,-1.));
#32578=DIRECTION('center_axis',(0.,0.,1.));
#32579=DIRECTION('ref_axis',(1.,0.,0.));
#32580=DIRECTION('center_axis',(0.,0.,1.));
#32581=DIRECTION('ref_axis',(1.,0.,0.));
#32582=DIRECTION('center_axis',(0.,0.,1.));
#32583=DIRECTION('ref_axis',(1.,0.,0.));
#32584=DIRECTION('center_axis',(0.,0.,1.));
#32585=DIRECTION('ref_axis',(1.,0.,0.));
#32586=DIRECTION('center_axis',(0.,0.,1.));
#32587=DIRECTION('ref_axis',(1.,0.,0.));
#32588=DIRECTION('center_axis',(0.,0.,1.));
#32589=DIRECTION('ref_axis',(1.,0.,0.));
#32590=DIRECTION('center_axis',(0.,0.,1.));
#32591=DIRECTION('ref_axis',(1.,0.,0.));
#32592=DIRECTION('center_axis',(0.,0.,1.));
#32593=DIRECTION('ref_axis',(1.,0.,0.));
#32594=DIRECTION('center_axis',(0.,0.,1.));
#32595=DIRECTION('ref_axis',(1.,0.,0.));
#32596=DIRECTION('center_axis',(0.,0.,1.));
#32597=DIRECTION('ref_axis',(1.,0.,0.));
#32598=DIRECTION('center_axis',(0.,0.,1.));
#32599=DIRECTION('ref_axis',(1.,0.,0.));
#32600=DIRECTION('center_axis',(0.,0.,1.));
#32601=DIRECTION('ref_axis',(1.,0.,0.));
#32602=DIRECTION('center_axis',(0.,0.,1.));
#32603=DIRECTION('ref_axis',(1.,0.,0.));
#32604=DIRECTION('center_axis',(0.,0.,1.));
#32605=DIRECTION('ref_axis',(1.,0.,0.));
#32606=DIRECTION('center_axis',(0.,0.,1.));
#32607=DIRECTION('ref_axis',(1.,0.,0.));
#32608=DIRECTION('center_axis',(0.,0.,1.));
#32609=DIRECTION('ref_axis',(1.,0.,0.));
#32610=DIRECTION('center_axis',(0.,0.,1.));
#32611=DIRECTION('ref_axis',(1.,0.,0.));
#32612=DIRECTION('center_axis',(0.,0.,1.));
#32613=DIRECTION('ref_axis',(1.,0.,0.));
#32614=DIRECTION('center_axis',(0.,0.,1.));
#32615=DIRECTION('ref_axis',(1.,0.,0.));
#32616=DIRECTION('',(0.,0.,-1.));
#32617=DIRECTION('center_axis',(0.,0.,-1.));
#32618=DIRECTION('ref_axis',(1.,0.,0.));
#32619=DIRECTION('',(0.,0.,1.));
#32620=DIRECTION('center_axis',(0.,0.,1.));
#32621=DIRECTION('ref_axis',(1.,0.,0.));
#32622=DIRECTION('center_axis',(-0.259973473447872,-0.96561575852067,0.));
#32623=DIRECTION('ref_axis',(0.96561575852067,-0.259973473447872,0.));
#32624=DIRECTION('',(0.96561575852067,-0.259973473447872,0.));
#32625=DIRECTION('',(0.,0.,1.));
#32626=DIRECTION('center_axis',(-0.259973473447872,0.96561575852067,0.));
#32627=DIRECTION('ref_axis',(-0.96561575852067,-0.259973473447872,0.));
#32628=DIRECTION('',(-0.96561575852067,-0.259973473447872,0.));
#32629=DIRECTION('center_axis',(0.,0.,1.));
#32630=DIRECTION('ref_axis',(1.,0.,0.));
#32631=DIRECTION('center_axis',(0.,0.,-1.));
#32632=DIRECTION('ref_axis',(1.,0.,0.));
#32633=DIRECTION('center_axis',(0.,0.,1.));
#32634=DIRECTION('ref_axis',(1.,0.,0.));
#32635=DIRECTION('',(-0.707106781186548,-8.65956056235493E-17,-0.707106781186548));
#32636=DIRECTION('center_axis',(0.,0.,1.));
#32637=DIRECTION('ref_axis',(1.,0.,0.));
#32638=DIRECTION('',(-0.842487928864452,-1.03175014540413E-16,0.538715221353255));
#32639=DIRECTION('center_axis',(0.,0.,-1.));
#32640=DIRECTION('ref_axis',(1.,0.,0.));
#32641=DIRECTION('center_axis',(0.5,0.866025403784439,0.));
#32642=DIRECTION('ref_axis',(0.866025403784439,-0.5,0.));
#32643=DIRECTION('',(0.866025403784439,-0.5,0.));
#32644=DIRECTION('',(0.,0.,-1.));
#32645=DIRECTION('',(0.866025403784439,-0.5,0.));
#32646=DIRECTION('',(0.,0.,-1.));
#32647=DIRECTION('center_axis',(-0.5,0.866025403784439,0.));
#32648=DIRECTION('ref_axis',(0.866025403784439,0.5,0.));
#32649=DIRECTION('',(0.866025403784439,0.5,0.));
#32650=DIRECTION('',(0.,0.,-1.));
#32651=DIRECTION('',(0.866025403784439,0.5,0.));
#32652=DIRECTION('center_axis',(-1.,-1.60246890531964E-16,0.));
#32653=DIRECTION('ref_axis',(-1.60246890531964E-16,1.,0.));
#32654=DIRECTION('',(-1.60246890531964E-16,1.,0.));
#32655=DIRECTION('',(0.,0.,-1.));
#32656=DIRECTION('',(-1.60246890531964E-16,1.,0.));
#32657=DIRECTION('center_axis',(-0.5,-0.866025403784439,0.));
#32658=DIRECTION('ref_axis',(-0.866025403784439,0.5,0.));
#32659=DIRECTION('',(-0.866025403784439,0.5,0.));
#32660=DIRECTION('',(0.,0.,-1.));
#32661=DIRECTION('',(-0.866025403784439,0.5,0.));
#32662=DIRECTION('center_axis',(0.5,-0.866025403784439,0.));
#32663=DIRECTION('ref_axis',(-0.866025403784439,-0.5,0.));
#32664=DIRECTION('',(-0.866025403784439,-0.5,0.));
#32665=DIRECTION('',(0.,0.,-1.));
#32666=DIRECTION('',(-0.866025403784439,-0.5,0.));
#32667=DIRECTION('center_axis',(1.,-3.20493781063927E-16,0.));
#32668=DIRECTION('ref_axis',(-3.20493781063927E-16,-1.,0.));
#32669=DIRECTION('',(-3.20493781063927E-16,-1.,0.));
#32670=DIRECTION('',(-3.20493781063927E-16,-1.,0.));
#32671=DIRECTION('center_axis',(0.,0.,-1.));
#32672=DIRECTION('ref_axis',(-1.,0.,0.));
#32673=DIRECTION('center_axis',(0.,0.,-1.));
#32674=DIRECTION('ref_axis',(-1.,0.,0.));
#32675=DIRECTION('center_axis',(0.,0.,1.));
#32676=DIRECTION('ref_axis',(1.,0.,0.));
#32677=DIRECTION('center_axis',(0.,0.,1.));
#32678=DIRECTION('ref_axis',(1.,0.,0.));
#32679=DIRECTION('',(0.707106781186547,8.65956056235493E-17,-0.707106781186548));
#32680=DIRECTION('center_axis',(0.,0.,1.));
#32681=DIRECTION('ref_axis',(1.,0.,0.));
#32682=DIRECTION('center_axis',(0.,0.,1.));
#32683=DIRECTION('ref_axis',(1.,0.,0.));
#32684=DIRECTION('center_axis',(0.,0.,1.));
#32685=DIRECTION('ref_axis',(1.,0.,0.));
#32686=DIRECTION('center_axis',(0.,0.,1.));
#32687=DIRECTION('ref_axis',(1.,0.,0.));
#32688=DIRECTION('',(0.707106781186548,8.65956056235494E-17,-0.707106781186547));
#32689=DIRECTION('center_axis',(0.,0.,-1.));
#32690=DIRECTION('ref_axis',(-1.,0.,0.));
#32691=DIRECTION('center_axis',(0.,0.,1.));
#32692=DIRECTION('ref_axis',(1.,0.,0.));
#32693=DIRECTION('axis',(0.,0.,1.));
#32694=DIRECTION('refdir',(1.,0.,0.));
#32695=DIRECTION('center_axis',(0.,0.,1.));
#32696=DIRECTION('ref_axis',(1.,0.,0.));
#32697=DIRECTION('',(0.,0.,-1.));
#32698=DIRECTION('center_axis',(0.,0.,-1.));
#32699=DIRECTION('ref_axis',(1.,0.,0.));
#32700=DIRECTION('',(0.,0.,-1.));
#32701=DIRECTION('center_axis',(0.,0.,1.));
#32702=DIRECTION('ref_axis',(1.,0.,0.));
#32703=DIRECTION('center_axis',(0.,0.,-1.));
#32704=DIRECTION('ref_axis',(1.,0.,0.));
#32705=DIRECTION('center_axis',(0.,0.,1.));
#32706=DIRECTION('ref_axis',(1.,0.,0.));
#32707=DIRECTION('',(0.,0.,-1.));
#32708=DIRECTION('center_axis',(0.,0.,1.));
#32709=DIRECTION('ref_axis',(1.,0.,0.));
#32710=DIRECTION('',(0.,0.,-1.));
#32711=DIRECTION('center_axis',(0.,0.,1.));
#32712=DIRECTION('ref_axis',(1.,0.,0.));
#32713=DIRECTION('',(0.,0.,-1.));
#32714=DIRECTION('center_axis',(0.,0.,1.));
#32715=DIRECTION('ref_axis',(1.,0.,0.));
#32716=DIRECTION('',(0.,0.,-1.));
#32717=DIRECTION('center_axis',(0.,0.,1.));
#32718=DIRECTION('ref_axis',(1.,0.,0.));
#32719=DIRECTION('',(0.,0.,-1.));
#32720=DIRECTION('center_axis',(0.,0.,1.));
#32721=DIRECTION('ref_axis',(1.,0.,0.));
#32722=DIRECTION('',(0.,0.,-1.));
#32723=DIRECTION('center_axis',(0.,0.,1.));
#32724=DIRECTION('ref_axis',(1.,0.,0.));
#32725=DIRECTION('',(0.,0.,-1.));
#32726=DIRECTION('center_axis',(0.,0.,1.));
#32727=DIRECTION('ref_axis',(1.,0.,0.));
#32728=DIRECTION('',(0.,0.,-1.));
#32729=DIRECTION('center_axis',(0.,0.,1.));
#32730=DIRECTION('ref_axis',(1.,0.,0.));
#32731=DIRECTION('',(0.,0.,-1.));
#32732=DIRECTION('center_axis',(0.,0.,1.));
#32733=DIRECTION('ref_axis',(1.,0.,0.));
#32734=DIRECTION('',(0.,0.,-1.));
#32735=DIRECTION('center_axis',(0.,0.,1.));
#32736=DIRECTION('ref_axis',(1.,0.,0.));
#32737=DIRECTION('',(0.,0.,-1.));
#32738=DIRECTION('center_axis',(0.,0.,1.));
#32739=DIRECTION('ref_axis',(0.795872373896981,-0.605464420480332,0.));
#32740=DIRECTION('',(0.,0.,1.));
#32741=DIRECTION('center_axis',(0.,0.,1.));
#32742=DIRECTION('ref_axis',(1.,8.36459283980496E-14,0.));
#32743=DIRECTION('center_axis',(0.,0.,1.));
#32744=DIRECTION('ref_axis',(1.,8.36459283980496E-14,0.));
#32745=DIRECTION('',(0.,0.,1.));
#32746=DIRECTION('center_axis',(0.,0.,1.));
#32747=DIRECTION('ref_axis',(1.,8.36459283980496E-14,0.));
#32748=DIRECTION('',(0.,0.,1.));
#32749=DIRECTION('center_axis',(0.,0.,1.));
#32750=DIRECTION('ref_axis',(1.,8.36459283980496E-14,0.));
#32751=DIRECTION('',(0.,0.,1.));
#32752=DIRECTION('center_axis',(0.,0.,1.));
#32753=DIRECTION('ref_axis',(1.,8.36459283980496E-14,0.));
#32754=DIRECTION('',(0.,0.,1.));
#32755=DIRECTION('center_axis',(0.,0.,1.));
#32756=DIRECTION('ref_axis',(1.,8.36459283980496E-14,0.));
#32757=DIRECTION('',(0.,0.,1.));
#32758=DIRECTION('center_axis',(0.,0.,1.));
#32759=DIRECTION('ref_axis',(1.,8.36459283980496E-14,0.));
#32760=DIRECTION('',(0.,0.,1.));
#32761=DIRECTION('center_axis',(0.,0.,1.));
#32762=DIRECTION('ref_axis',(1.,8.36459283980496E-14,0.));
#32763=DIRECTION('',(0.,0.,1.));
#32764=DIRECTION('center_axis',(0.,0.,1.));
#32765=DIRECTION('ref_axis',(1.,8.36459283980496E-14,0.));
#32766=DIRECTION('',(0.,0.,1.));
#32767=DIRECTION('center_axis',(0.,0.,1.));
#32768=DIRECTION('ref_axis',(1.,8.36459283980496E-14,0.));
#32769=DIRECTION('',(0.,0.,1.));
#32770=DIRECTION('center_axis',(0.,0.,1.));
#32771=DIRECTION('ref_axis',(1.,8.36459283980496E-14,0.));
#32772=DIRECTION('',(0.,0.,1.));
#32773=DIRECTION('center_axis',(0.,0.,1.));
#32774=DIRECTION('ref_axis',(1.,8.36459283980496E-14,0.));
#32775=DIRECTION('',(0.,0.,1.));
#32776=DIRECTION('center_axis',(0.,0.,-1.));
#32777=DIRECTION('ref_axis',(1.,8.36459283980496E-14,0.));
#32778=DIRECTION('center_axis',(0.,0.,1.));
#32779=DIRECTION('ref_axis',(1.,0.,0.));
#32780=DIRECTION('center_axis',(0.,0.,1.));
#32781=DIRECTION('ref_axis',(1.,0.,0.));
#32782=DIRECTION('center_axis',(0.,0.,1.));
#32783=DIRECTION('ref_axis',(1.,0.,0.));
#32784=DIRECTION('center_axis',(0.,0.,1.));
#32785=DIRECTION('ref_axis',(1.,0.,0.));
#32786=DIRECTION('center_axis',(0.,0.,-1.));
#32787=DIRECTION('ref_axis',(1.,8.36459283980496E-14,0.));
#32788=DIRECTION('center_axis',(0.,0.,1.));
#32789=DIRECTION('ref_axis',(1.,8.36459283980496E-14,0.));
#32790=DIRECTION('center_axis',(0.,0.,1.));
#32791=DIRECTION('ref_axis',(-0.669920523853501,-0.74243281966778,0.));
#32792=DIRECTION('center_axis',(0.,0.,1.));
#32793=DIRECTION('ref_axis',(1.,0.,0.));
#32794=DIRECTION('center_axis',(0.,0.,1.));
#32795=DIRECTION('ref_axis',(0.984807753012208,-0.17364817766693,0.));
#32796=DIRECTION('center_axis',(0.,0.,-1.));
#32797=DIRECTION('ref_axis',(1.,0.,0.));
#32798=DIRECTION('',(-0.996089805327885,-0.0883464754353932,0.));
#32799=DIRECTION('',(0.905801965515954,-0.423701309022563,0.));
#32800=DIRECTION('center_axis',(-0.423701309022563,-0.905801965515954,0.));
#32801=DIRECTION('ref_axis',(0.905801965515954,-0.423701309022563,0.));
#32802=DIRECTION('',(0.,0.,1.));
#32803=DIRECTION('',(0.,0.,1.));
#32804=DIRECTION('center_axis',(-0.0883464754353932,0.996089805327885,0.));
#32805=DIRECTION('ref_axis',(-0.996089805327885,-0.0883464754353932,0.));
#32806=DIRECTION('',(0.,0.,-1.));
#32807=DIRECTION('center_axis',(0.,0.,1.));
#32808=DIRECTION('ref_axis',(0.939692620785908,-0.342020143325669,0.));
#32809=DIRECTION('center_axis',(0.,0.,-1.));
#32810=DIRECTION('ref_axis',(1.,0.,0.));
#32811=DIRECTION('',(-0.996298167445974,0.0859648855277176,0.));
#32812=DIRECTION('',(0.818465838146947,-0.574555194725812,0.));
#32813=DIRECTION('center_axis',(-0.574555194725812,-0.818465838146947,0.));
#32814=DIRECTION('ref_axis',(0.818465838146947,-0.574555194725812,0.));
#32815=DIRECTION('',(0.,0.,1.));
#32816=DIRECTION('',(0.,0.,1.));
#32817=DIRECTION('center_axis',(0.0859648855277176,0.996298167445974,0.));
#32818=DIRECTION('ref_axis',(-0.996298167445974,0.0859648855277176,0.));
#32819=DIRECTION('',(0.,0.,-1.));
#32820=DIRECTION('center_axis',(0.,0.,1.));
#32821=DIRECTION('ref_axis',(0.866025403784438,-0.5,0.));
#32822=DIRECTION('center_axis',(0.,0.,-1.));
#32823=DIRECTION('ref_axis',(1.,0.,0.));
#32824=DIRECTION('',(-0.966234513897416,0.257664246944399,0.));
#32825=DIRECTION('',(0.706261040449543,-0.707951511576272,0.));
#32826=DIRECTION('center_axis',(-0.707951511576272,-0.706261040449543,0.));
#32827=DIRECTION('ref_axis',(0.706261040449543,-0.707951511576272,0.));
#32828=DIRECTION('',(0.,0.,1.));
#32829=DIRECTION('',(0.,0.,1.));
#32830=DIRECTION('center_axis',(0.257664246944399,0.966234513897416,0.));
#32831=DIRECTION('ref_axis',(-0.966234513897416,0.257664246944399,0.));
#32832=DIRECTION('',(0.,0.,-1.));
#32833=DIRECTION('center_axis',(0.,0.,1.));
#32834=DIRECTION('ref_axis',(0.766044443118978,-0.64278760968654,0.));
#32835=DIRECTION('center_axis',(0.,0.,-1.));
#32836=DIRECTION('ref_axis',(1.,0.,0.));
#32837=DIRECTION('',(-0.906812313582341,0.421534610602074,0.));
#32838=DIRECTION('',(0.572596858423411,-0.819837079988238,0.));
#32839=DIRECTION('center_axis',(-0.819837079988238,-0.572596858423411,0.));
#32840=DIRECTION('ref_axis',(0.572596858423411,-0.819837079988238,0.));
#32841=DIRECTION('',(0.,0.,1.));
#32842=DIRECTION('',(0.,0.,1.));
#32843=DIRECTION('center_axis',(0.421534610602074,0.906812313582341,0.));
#32844=DIRECTION('ref_axis',(-0.906812313582341,0.421534610602074,0.));
#32845=DIRECTION('',(0.,0.,-1.));
#32846=DIRECTION('center_axis',(0.,0.,1.));
#32847=DIRECTION('ref_axis',(0.642787609686539,-0.766044443118978,0.));
#32848=DIRECTION('center_axis',(0.,0.,-1.));
#32849=DIRECTION('ref_axis',(1.,0.,0.));
#32850=DIRECTION('',(-0.819837079988238,0.572596858423411,0.));
#32851=DIRECTION('',(0.421534610602074,-0.906812313582341,0.));
#32852=DIRECTION('center_axis',(-0.906812313582341,-0.421534610602074,0.));
#32853=DIRECTION('ref_axis',(0.421534610602074,-0.906812313582341,0.));
#32854=DIRECTION('',(0.,0.,1.));
#32855=DIRECTION('',(0.,0.,1.));
#32856=DIRECTION('center_axis',(0.572596858423411,0.819837079988238,0.));
#32857=DIRECTION('ref_axis',(-0.819837079988238,0.572596858423411,0.));
#32858=DIRECTION('',(0.,0.,-1.));
#32859=DIRECTION('center_axis',(0.,0.,1.));
#32860=DIRECTION('ref_axis',(0.5,-0.866025403784438,0.));
#32861=DIRECTION('center_axis',(0.,0.,-1.));
#32862=DIRECTION('ref_axis',(1.,0.,0.));
#32863=DIRECTION('',(-0.707951511576272,0.706261040449544,0.));
#32864=DIRECTION('',(0.257664246944398,-0.966234513897416,0.));
#32865=DIRECTION('center_axis',(-0.966234513897416,-0.257664246944398,0.));
#32866=DIRECTION('ref_axis',(0.257664246944398,-0.966234513897416,0.));
#32867=DIRECTION('',(0.,0.,1.));
#32868=DIRECTION('',(0.,0.,1.));
#32869=DIRECTION('center_axis',(0.706261040449544,0.707951511576272,0.));
#32870=DIRECTION('ref_axis',(-0.707951511576272,0.706261040449544,0.));
#32871=DIRECTION('',(0.,0.,-1.));
#32872=DIRECTION('center_axis',(0.,0.,1.));
#32873=DIRECTION('ref_axis',(0.342020143325668,-0.939692620785909,0.));
#32874=DIRECTION('center_axis',(0.,0.,-1.));
#32875=DIRECTION('ref_axis',(1.,0.,0.));
#32876=DIRECTION('',(-0.57455519472581,0.818465838146948,0.));
#32877=DIRECTION('',(0.0859648855277162,-0.996298167445974,0.));
#32878=DIRECTION('center_axis',(-0.996298167445974,-0.0859648855277162,
0.));
#32879=DIRECTION('ref_axis',(0.0859648855277162,-0.996298167445974,0.));
#32880=DIRECTION('',(0.,0.,1.));
#32881=DIRECTION('',(0.,0.,1.));
#32882=DIRECTION('center_axis',(0.818465838146948,0.57455519472581,0.));
#32883=DIRECTION('ref_axis',(-0.57455519472581,0.818465838146948,0.));
#32884=DIRECTION('',(0.,0.,-1.));
#32885=DIRECTION('center_axis',(0.,0.,1.));
#32886=DIRECTION('ref_axis',(0.17364817766693,-0.984807753012208,0.));
#32887=DIRECTION('center_axis',(0.,0.,-1.));
#32888=DIRECTION('ref_axis',(1.,0.,0.));
#32889=DIRECTION('',(-0.423701309022563,0.905801965515955,0.));
#32890=DIRECTION('',(-0.0883464754353936,-0.996089805327885,0.));
#32891=DIRECTION('center_axis',(-0.996089805327885,0.0883464754353937,0.));
#32892=DIRECTION('ref_axis',(-0.0883464754353937,-0.996089805327885,0.));
#32893=DIRECTION('',(0.,0.,1.));
#32894=DIRECTION('',(0.,0.,1.));
#32895=DIRECTION('center_axis',(0.905801965515955,0.423701309022563,0.));
#32896=DIRECTION('ref_axis',(-0.423701309022563,0.905801965515955,0.));
#32897=DIRECTION('',(0.,0.,-1.));
#32898=DIRECTION('center_axis',(0.,0.,1.));
#32899=DIRECTION('ref_axis',(-1.94289029309402E-16,-1.,0.));
#32900=DIRECTION('center_axis',(0.,0.,-1.));
#32901=DIRECTION('ref_axis',(1.,0.,0.));
#32902=DIRECTION('',(-0.259973473447872,0.96561575852067,0.));
#32903=DIRECTION('',(-0.259973473447873,-0.96561575852067,0.));
#32904=DIRECTION('center_axis',(-0.96561575852067,0.259973473447873,0.));
#32905=DIRECTION('ref_axis',(-0.259973473447873,-0.96561575852067,0.));
#32906=DIRECTION('',(0.,0.,1.));
#32907=DIRECTION('',(0.,0.,1.));
#32908=DIRECTION('center_axis',(0.96561575852067,0.259973473447872,0.));
#32909=DIRECTION('ref_axis',(-0.259973473447872,0.96561575852067,0.));
#32910=DIRECTION('',(0.,0.,-1.));
#32911=DIRECTION('center_axis',(0.,0.,1.));
#32912=DIRECTION('ref_axis',(-0.17364817766693,-0.984807753012208,0.));
#32913=DIRECTION('center_axis',(0.,0.,-1.));
#32914=DIRECTION('ref_axis',(1.,0.,0.));
#32915=DIRECTION('',(-0.0883464754353933,0.996089805327885,0.));
#32916=DIRECTION('',(-0.423701309022563,-0.905801965515955,0.));
#32917=DIRECTION('center_axis',(-0.905801965515955,0.423701309022563,0.));
#32918=DIRECTION('ref_axis',(-0.423701309022563,-0.905801965515955,0.));
#32919=DIRECTION('',(0.,0.,1.));
#32920=DIRECTION('',(0.,0.,1.));
#32921=DIRECTION('center_axis',(0.996089805327885,0.0883464754353932,0.));
#32922=DIRECTION('ref_axis',(-0.0883464754353932,0.996089805327885,0.));
#32923=DIRECTION('',(0.,0.,-1.));
#32924=DIRECTION('center_axis',(0.,0.,1.));
#32925=DIRECTION('ref_axis',(-0.342020143325669,-0.939692620785908,0.));
#32926=DIRECTION('center_axis',(0.,0.,-1.));
#32927=DIRECTION('ref_axis',(1.,0.,0.));
#32928=DIRECTION('',(0.0859648855277175,0.996298167445974,0.));
#32929=DIRECTION('',(-0.574555194725811,-0.818465838146947,0.));
#32930=DIRECTION('center_axis',(-0.818465838146947,0.574555194725811,0.));
#32931=DIRECTION('ref_axis',(-0.574555194725811,-0.818465838146947,0.));
#32932=DIRECTION('',(0.,0.,1.));
#32933=DIRECTION('',(0.,0.,1.));
#32934=DIRECTION('center_axis',(0.996298167445974,-0.0859648855277175,0.));
#32935=DIRECTION('ref_axis',(0.0859648855277175,0.996298167445974,0.));
#32936=DIRECTION('',(0.,0.,-1.));
#32937=DIRECTION('center_axis',(0.,0.,1.));
#32938=DIRECTION('ref_axis',(-0.5,-0.866025403784438,0.));
#32939=DIRECTION('center_axis',(0.,0.,-1.));
#32940=DIRECTION('ref_axis',(1.,0.,0.));
#32941=DIRECTION('',(0.257664246944399,0.966234513897416,0.));
#32942=DIRECTION('',(-0.707951511576272,-0.706261040449543,0.));
#32943=DIRECTION('center_axis',(-0.706261040449543,0.707951511576272,0.));
#32944=DIRECTION('ref_axis',(-0.707951511576272,-0.706261040449543,0.));
#32945=DIRECTION('',(0.,0.,1.));
#32946=DIRECTION('',(0.,0.,1.));
#32947=DIRECTION('center_axis',(0.966234513897416,-0.257664246944399,0.));
#32948=DIRECTION('ref_axis',(0.257664246944399,0.966234513897416,0.));
#32949=DIRECTION('',(0.,0.,-1.));
#32950=DIRECTION('center_axis',(0.,0.,1.));
#32951=DIRECTION('ref_axis',(-0.642787609686539,-0.766044443118978,0.));
#32952=DIRECTION('center_axis',(0.,0.,-1.));
#32953=DIRECTION('ref_axis',(1.,0.,0.));
#32954=DIRECTION('',(0.421534610602074,0.906812313582341,0.));
#32955=DIRECTION('',(-0.819837079988238,-0.572596858423411,0.));
#32956=DIRECTION('center_axis',(-0.572596858423411,0.819837079988238,0.));
#32957=DIRECTION('ref_axis',(-0.819837079988238,-0.572596858423411,0.));
#32958=DIRECTION('',(0.,0.,1.));
#32959=DIRECTION('',(0.,0.,1.));
#32960=DIRECTION('center_axis',(0.906812313582341,-0.421534610602074,0.));
#32961=DIRECTION('ref_axis',(0.421534610602074,0.906812313582341,0.));
#32962=DIRECTION('',(0.,0.,-1.));
#32963=DIRECTION('center_axis',(0.,0.,1.));
#32964=DIRECTION('ref_axis',(-0.766044443118978,-0.642787609686539,0.));
#32965=DIRECTION('center_axis',(0.,0.,-1.));
#32966=DIRECTION('ref_axis',(1.,0.,0.));
#32967=DIRECTION('',(0.572596858423411,0.819837079988238,0.));
#32968=DIRECTION('',(-0.906812313582341,-0.421534610602074,0.));
#32969=DIRECTION('center_axis',(-0.421534610602074,0.906812313582341,0.));
#32970=DIRECTION('ref_axis',(-0.906812313582341,-0.421534610602074,0.));
#32971=DIRECTION('',(0.,0.,1.));
#32972=DIRECTION('',(0.,0.,1.));
#32973=DIRECTION('center_axis',(0.819837079988238,-0.572596858423411,0.));
#32974=DIRECTION('ref_axis',(0.572596858423411,0.819837079988238,0.));
#32975=DIRECTION('',(0.,0.,-1.));
#32976=DIRECTION('center_axis',(0.,0.,1.));
#32977=DIRECTION('ref_axis',(-0.866025403784439,-0.5,0.));
#32978=DIRECTION('center_axis',(0.,0.,-1.));
#32979=DIRECTION('ref_axis',(1.,0.,0.));
#32980=DIRECTION('',(0.706261040449544,0.707951511576271,0.));
#32981=DIRECTION('',(-0.966234513897416,-0.257664246944398,0.));
#32982=DIRECTION('center_axis',(-0.257664246944398,0.966234513897416,0.));
#32983=DIRECTION('ref_axis',(-0.966234513897416,-0.257664246944398,0.));
#32984=DIRECTION('',(0.,0.,1.));
#32985=DIRECTION('',(0.,0.,1.));
#32986=DIRECTION('center_axis',(0.707951511576271,-0.706261040449544,0.));
#32987=DIRECTION('ref_axis',(0.706261040449544,0.707951511576271,0.));
#32988=DIRECTION('',(0.,0.,-1.));
#32989=DIRECTION('center_axis',(0.,0.,1.));
#32990=DIRECTION('ref_axis',(-0.939692620785909,-0.342020143325669,0.));
#32991=DIRECTION('center_axis',(0.,0.,-1.));
#32992=DIRECTION('ref_axis',(1.,0.,0.));
#32993=DIRECTION('',(0.818465838146948,0.574555194725811,0.));
#32994=DIRECTION('',(-0.996298167445974,-0.0859648855277167,0.));
#32995=DIRECTION('center_axis',(-0.0859648855277167,0.996298167445974,0.));
#32996=DIRECTION('ref_axis',(-0.996298167445974,-0.0859648855277167,0.));
#32997=DIRECTION('',(0.,0.,1.));
#32998=DIRECTION('',(0.,0.,1.));
#32999=DIRECTION('center_axis',(0.574555194725811,-0.818465838146948,0.));
#33000=DIRECTION('ref_axis',(0.818465838146948,0.574555194725811,0.));
#33001=DIRECTION('',(0.,0.,-1.));
#33002=DIRECTION('center_axis',(0.,0.,1.));
#33003=DIRECTION('ref_axis',(-0.984807753012208,-0.17364817766693,0.));
#33004=DIRECTION('center_axis',(0.,0.,-1.));
#33005=DIRECTION('ref_axis',(1.,0.,0.));
#33006=DIRECTION('',(0.905801965515955,0.423701309022563,0.));
#33007=DIRECTION('',(-0.996089805327885,0.0883464754353936,0.));
#33008=DIRECTION('center_axis',(0.0883464754353936,0.996089805327885,0.));
#33009=DIRECTION('ref_axis',(-0.996089805327885,0.0883464754353936,0.));
#33010=DIRECTION('',(0.,0.,1.));
#33011=DIRECTION('',(0.,0.,1.));
#33012=DIRECTION('center_axis',(0.423701309022563,-0.905801965515955,0.));
#33013=DIRECTION('ref_axis',(0.905801965515955,0.423701309022563,0.));
#33014=DIRECTION('',(0.,0.,-1.));
#33015=DIRECTION('center_axis',(0.,0.,1.));
#33016=DIRECTION('ref_axis',(-1.,1.11022302462516E-16,0.));
#33017=DIRECTION('center_axis',(0.,0.,-1.));
#33018=DIRECTION('ref_axis',(1.,0.,0.));
#33019=DIRECTION('',(0.96561575852067,0.259973473447872,0.));
#33020=DIRECTION('',(-0.96561575852067,0.259973473447873,0.));
#33021=DIRECTION('center_axis',(0.,0.,-1.));
#33022=DIRECTION('ref_axis',(1.,0.,0.));
#33023=DIRECTION('center_axis',(0.259973473447873,0.96561575852067,0.));
#33024=DIRECTION('ref_axis',(-0.96561575852067,0.259973473447873,0.));
#33025=DIRECTION('',(0.,0.,1.));
#33026=DIRECTION('',(0.,0.,1.));
#33027=DIRECTION('center_axis',(0.259973473447872,-0.96561575852067,0.));
#33028=DIRECTION('ref_axis',(0.96561575852067,0.259973473447872,0.));
#33029=DIRECTION('',(0.,0.,-1.));
#33030=DIRECTION('center_axis',(0.,0.,1.));
#33031=DIRECTION('ref_axis',(-0.984807753012208,0.173648177666931,0.));
#33032=DIRECTION('center_axis',(0.,0.,-1.));
#33033=DIRECTION('ref_axis',(1.,0.,0.));
#33034=DIRECTION('',(0.996089805327885,0.0883464754353928,0.));
#33035=DIRECTION('',(-0.905801965515954,0.423701309022564,0.));
#33036=DIRECTION('center_axis',(0.423701309022564,0.905801965515954,0.));
#33037=DIRECTION('ref_axis',(-0.905801965515954,0.423701309022564,0.));
#33038=DIRECTION('',(0.,0.,1.));
#33039=DIRECTION('',(0.,0.,1.));
#33040=DIRECTION('center_axis',(0.0883464754353928,-0.996089805327885,0.));
#33041=DIRECTION('ref_axis',(0.996089805327885,0.0883464754353928,0.));
#33042=DIRECTION('',(0.,0.,-1.));
#33043=DIRECTION('center_axis',(0.,0.,1.));
#33044=DIRECTION('ref_axis',(-0.939692620785908,0.342020143325669,0.));
#33045=DIRECTION('center_axis',(0.,0.,-1.));
#33046=DIRECTION('ref_axis',(1.,0.,0.));
#33047=DIRECTION('',(0.996298167445974,-0.085964885527717,0.));
#33048=DIRECTION('',(-0.818465838146948,0.574555194725811,0.));
#33049=DIRECTION('center_axis',(0.574555194725811,0.818465838146948,0.));
#33050=DIRECTION('ref_axis',(-0.818465838146948,0.574555194725811,0.));
#33051=DIRECTION('',(0.,0.,1.));
#33052=DIRECTION('',(0.,0.,1.));
#33053=DIRECTION('center_axis',(-0.085964885527717,-0.996298167445974,0.));
#33054=DIRECTION('ref_axis',(0.996298167445974,-0.085964885527717,0.));
#33055=DIRECTION('',(0.,0.,-1.));
#33056=DIRECTION('center_axis',(0.,0.,1.));
#33057=DIRECTION('ref_axis',(-0.866025403784439,0.5,0.));
#33058=DIRECTION('center_axis',(0.,0.,-1.));
#33059=DIRECTION('ref_axis',(1.,0.,0.));
#33060=DIRECTION('',(0.966234513897416,-0.257664246944398,0.));
#33061=DIRECTION('',(-0.706261040449544,0.707951511576272,0.));
#33062=DIRECTION('center_axis',(0.707951511576272,0.706261040449544,0.));
#33063=DIRECTION('ref_axis',(-0.706261040449544,0.707951511576272,0.));
#33064=DIRECTION('',(0.,0.,1.));
#33065=DIRECTION('',(0.,0.,1.));
#33066=DIRECTION('center_axis',(-0.257664246944398,-0.966234513897416,0.));
#33067=DIRECTION('ref_axis',(0.966234513897416,-0.257664246944398,0.));
#33068=DIRECTION('',(0.,0.,-1.));
#33069=DIRECTION('center_axis',(0.,0.,1.));
#33070=DIRECTION('ref_axis',(-0.766044443118978,0.642787609686539,0.));
#33071=DIRECTION('center_axis',(0.,0.,-1.));
#33072=DIRECTION('ref_axis',(1.,0.,0.));
#33073=DIRECTION('',(0.906812313582341,-0.421534610602074,0.));
#33074=DIRECTION('',(-0.572596858423411,0.819837079988238,0.));
#33075=DIRECTION('center_axis',(0.819837079988238,0.572596858423411,0.));
#33076=DIRECTION('ref_axis',(-0.572596858423411,0.819837079988238,0.));
#33077=DIRECTION('',(0.,0.,1.));
#33078=DIRECTION('',(0.,0.,1.));
#33079=DIRECTION('center_axis',(-0.421534610602074,-0.906812313582341,0.));
#33080=DIRECTION('ref_axis',(0.906812313582341,-0.421534610602074,0.));
#33081=DIRECTION('',(0.,0.,-1.));
#33082=DIRECTION('center_axis',(0.,0.,1.));
#33083=DIRECTION('ref_axis',(-0.642787609686539,0.766044443118978,0.));
#33084=DIRECTION('center_axis',(0.,0.,-1.));
#33085=DIRECTION('ref_axis',(1.,0.,0.));
#33086=DIRECTION('',(0.819837079988238,-0.572596858423411,0.));
#33087=DIRECTION('',(-0.421534610602074,0.906812313582341,0.));
#33088=DIRECTION('center_axis',(0.906812313582341,0.421534610602074,0.));
#33089=DIRECTION('ref_axis',(-0.421534610602074,0.906812313582341,0.));
#33090=DIRECTION('',(0.,0.,1.));
#33091=DIRECTION('',(0.,0.,1.));
#33092=DIRECTION('center_axis',(-0.572596858423411,-0.819837079988238,0.));
#33093=DIRECTION('ref_axis',(0.819837079988238,-0.572596858423411,0.));
#33094=DIRECTION('',(0.,0.,-1.));
#33095=DIRECTION('center_axis',(0.,0.,1.));
#33096=DIRECTION('ref_axis',(-0.5,0.866025403784439,0.));
#33097=DIRECTION('center_axis',(0.,0.,-1.));
#33098=DIRECTION('ref_axis',(1.,0.,0.));
#33099=DIRECTION('',(0.707951511576272,-0.706261040449544,0.));
#33100=DIRECTION('',(-0.257664246944398,0.966234513897416,0.));
#33101=DIRECTION('center_axis',(0.966234513897416,0.257664246944398,0.));
#33102=DIRECTION('ref_axis',(-0.257664246944398,0.966234513897416,0.));
#33103=DIRECTION('',(0.,0.,1.));
#33104=DIRECTION('',(0.,0.,1.));
#33105=DIRECTION('center_axis',(-0.706261040449544,-0.707951511576272,0.));
#33106=DIRECTION('ref_axis',(0.707951511576272,-0.706261040449544,0.));
#33107=DIRECTION('',(0.,0.,-1.));
#33108=DIRECTION('center_axis',(0.,0.,1.));
#33109=DIRECTION('ref_axis',(-0.342020143325669,0.939692620785909,0.));
#33110=DIRECTION('center_axis',(0.,0.,-1.));
#33111=DIRECTION('ref_axis',(1.,0.,0.));
#33112=DIRECTION('',(0.574555194725811,-0.818465838146948,0.));
#33113=DIRECTION('',(-0.0859648855277167,0.996298167445974,0.));
#33114=DIRECTION('center_axis',(0.996298167445974,0.0859648855277167,0.));
#33115=DIRECTION('ref_axis',(-0.0859648855277167,0.996298167445974,0.));
#33116=DIRECTION('',(0.,0.,1.));
#33117=DIRECTION('',(0.,0.,1.));
#33118=DIRECTION('center_axis',(-0.818465838146948,-0.574555194725811,0.));
#33119=DIRECTION('ref_axis',(0.574555194725811,-0.818465838146948,0.));
#33120=DIRECTION('',(0.,0.,-1.));
#33121=DIRECTION('center_axis',(0.,0.,1.));
#33122=DIRECTION('ref_axis',(-0.17364817766693,0.984807753012208,0.));
#33123=DIRECTION('center_axis',(0.,0.,-1.));
#33124=DIRECTION('ref_axis',(1.,0.,0.));
#33125=DIRECTION('',(0.423701309022563,-0.905801965515955,0.));
#33126=DIRECTION('',(0.0883464754353932,0.996089805327885,0.));
#33127=DIRECTION('center_axis',(0.996089805327885,-0.0883464754353932,0.));
#33128=DIRECTION('ref_axis',(0.0883464754353932,0.996089805327885,0.));
#33129=DIRECTION('',(0.,0.,1.));
#33130=DIRECTION('',(0.,0.,1.));
#33131=DIRECTION('center_axis',(-0.905801965515955,-0.423701309022563,0.));
#33132=DIRECTION('ref_axis',(0.423701309022563,-0.905801965515955,0.));
#33133=DIRECTION('',(0.,0.,-1.));
#33134=DIRECTION('center_axis',(0.,0.,1.));
#33135=DIRECTION('ref_axis',(5.55111512312578E-17,1.,0.));
#33136=DIRECTION('center_axis',(0.,0.,-1.));
#33137=DIRECTION('ref_axis',(1.,0.,0.));
#33138=DIRECTION('',(0.259973473447872,-0.96561575852067,0.));
#33139=DIRECTION('',(0.259973473447872,0.96561575852067,0.));
#33140=DIRECTION('center_axis',(0.96561575852067,-0.259973473447873,0.));
#33141=DIRECTION('ref_axis',(0.259973473447873,0.96561575852067,0.));
#33142=DIRECTION('',(0.,0.,1.));
#33143=DIRECTION('',(0.,0.,1.));
#33144=DIRECTION('center_axis',(-0.96561575852067,-0.259973473447872,0.));
#33145=DIRECTION('ref_axis',(0.259973473447872,-0.96561575852067,0.));
#33146=DIRECTION('',(0.,0.,-1.));
#33147=DIRECTION('center_axis',(0.,0.,1.));
#33148=DIRECTION('ref_axis',(0.17364817766693,0.984807753012208,0.));
#33149=DIRECTION('center_axis',(0.,0.,-1.));
#33150=DIRECTION('ref_axis',(1.,0.,0.));
#33151=DIRECTION('',(0.0883464754353931,-0.996089805327885,0.));
#33152=DIRECTION('',(0.423701309022563,0.905801965515954,0.));
#33153=DIRECTION('center_axis',(0.905801965515954,-0.423701309022563,0.));
#33154=DIRECTION('ref_axis',(0.423701309022563,0.905801965515954,0.));
#33155=DIRECTION('',(0.,0.,1.));
#33156=DIRECTION('',(0.,0.,1.));
#33157=DIRECTION('center_axis',(-0.996089805327885,-0.0883464754353932,
0.));
#33158=DIRECTION('ref_axis',(0.0883464754353932,-0.996089805327885,0.));
#33159=DIRECTION('',(0.,0.,-1.));
#33160=DIRECTION('center_axis',(0.,0.,1.));
#33161=DIRECTION('ref_axis',(0.342020143325669,0.939692620785908,0.));
#33162=DIRECTION('center_axis',(0.,0.,-1.));
#33163=DIRECTION('ref_axis',(1.,0.,0.));
#33164=DIRECTION('',(-0.085964885527717,-0.996298167445974,0.));
#33165=DIRECTION('',(0.574555194725811,0.818465838146948,0.));
#33166=DIRECTION('center_axis',(0.818465838146948,-0.574555194725811,0.));
#33167=DIRECTION('ref_axis',(0.574555194725811,0.818465838146948,0.));
#33168=DIRECTION('',(0.,0.,1.));
#33169=DIRECTION('',(0.,0.,1.));
#33170=DIRECTION('center_axis',(-0.996298167445974,0.085964885527717,0.));
#33171=DIRECTION('ref_axis',(-0.085964885527717,-0.996298167445974,0.));
#33172=DIRECTION('',(0.,0.,-1.));
#33173=DIRECTION('center_axis',(0.,0.,1.));
#33174=DIRECTION('ref_axis',(0.5,0.866025403784439,0.));
#33175=DIRECTION('center_axis',(0.,0.,-1.));
#33176=DIRECTION('ref_axis',(1.,0.,0.));
#33177=DIRECTION('',(-0.257664246944398,-0.966234513897416,0.));
#33178=DIRECTION('',(0.707951511576272,0.706261040449544,0.));
#33179=DIRECTION('center_axis',(0.706261040449544,-0.707951511576272,0.));
#33180=DIRECTION('ref_axis',(0.707951511576272,0.706261040449544,0.));
#33181=DIRECTION('',(0.,0.,1.));
#33182=DIRECTION('',(0.,0.,1.));
#33183=DIRECTION('center_axis',(-0.966234513897416,0.257664246944398,0.));
#33184=DIRECTION('ref_axis',(-0.257664246944398,-0.966234513897416,0.));
#33185=DIRECTION('',(0.,0.,-1.));
#33186=DIRECTION('center_axis',(0.,0.,1.));
#33187=DIRECTION('ref_axis',(0.642787609686539,0.766044443118978,0.));
#33188=DIRECTION('center_axis',(0.,0.,-1.));
#33189=DIRECTION('ref_axis',(1.,0.,0.));
#33190=DIRECTION('',(-0.421534610602074,-0.906812313582341,0.));
#33191=DIRECTION('',(0.819837079988238,0.572596858423411,0.));
#33192=DIRECTION('center_axis',(0.572596858423411,-0.819837079988238,0.));
#33193=DIRECTION('ref_axis',(0.819837079988238,0.572596858423411,0.));
#33194=DIRECTION('',(0.,0.,1.));
#33195=DIRECTION('',(0.,0.,1.));
#33196=DIRECTION('center_axis',(-0.906812313582341,0.421534610602074,0.));
#33197=DIRECTION('ref_axis',(-0.421534610602074,-0.906812313582341,0.));
#33198=DIRECTION('',(0.,0.,-1.));
#33199=DIRECTION('center_axis',(0.,0.,1.));
#33200=DIRECTION('ref_axis',(0.766044443118978,0.642787609686539,0.));
#33201=DIRECTION('center_axis',(0.,0.,-1.));
#33202=DIRECTION('ref_axis',(1.,0.,0.));
#33203=DIRECTION('',(-0.572596858423411,-0.819837079988238,0.));
#33204=DIRECTION('',(0.906812313582341,0.421534610602074,0.));
#33205=DIRECTION('center_axis',(0.421534610602074,-0.906812313582341,0.));
#33206=DIRECTION('ref_axis',(0.906812313582341,0.421534610602074,0.));
#33207=DIRECTION('',(0.,0.,1.));
#33208=DIRECTION('',(0.,0.,1.));
#33209=DIRECTION('center_axis',(-0.819837079988238,0.572596858423411,0.));
#33210=DIRECTION('ref_axis',(-0.572596858423411,-0.819837079988238,0.));
#33211=DIRECTION('',(0.,0.,-1.));
#33212=DIRECTION('center_axis',(0.,0.,1.));
#33213=DIRECTION('ref_axis',(0.866025403784439,0.5,0.));
#33214=DIRECTION('center_axis',(0.,0.,-1.));
#33215=DIRECTION('ref_axis',(1.,0.,0.));
#33216=DIRECTION('',(-0.706261040449544,-0.707951511576272,0.));
#33217=DIRECTION('',(0.966234513897416,0.257664246944398,0.));
#33218=DIRECTION('center_axis',(0.257664246944398,-0.966234513897416,0.));
#33219=DIRECTION('ref_axis',(0.966234513897416,0.257664246944398,0.));
#33220=DIRECTION('',(0.,0.,1.));
#33221=DIRECTION('',(0.,0.,1.));
#33222=DIRECTION('center_axis',(-0.707951511576272,0.706261040449544,0.));
#33223=DIRECTION('ref_axis',(-0.706261040449544,-0.707951511576272,0.));
#33224=DIRECTION('',(0.,0.,-1.));
#33225=DIRECTION('center_axis',(0.,0.,1.));
#33226=DIRECTION('ref_axis',(0.939692620785909,0.342020143325669,0.));
#33227=DIRECTION('center_axis',(0.,0.,-1.));
#33228=DIRECTION('ref_axis',(1.,0.,0.));
#33229=DIRECTION('',(-0.818465838146948,-0.574555194725811,0.));
#33230=DIRECTION('',(0.996298167445974,0.0859648855277167,0.));
#33231=DIRECTION('center_axis',(0.0859648855277167,-0.996298167445974,0.));
#33232=DIRECTION('ref_axis',(0.996298167445974,0.0859648855277167,0.));
#33233=DIRECTION('',(0.,0.,1.));
#33234=DIRECTION('',(0.,0.,1.));
#33235=DIRECTION('center_axis',(-0.574555194725811,0.818465838146948,0.));
#33236=DIRECTION('ref_axis',(-0.818465838146948,-0.574555194725811,0.));
#33237=DIRECTION('',(0.,0.,-1.));
#33238=DIRECTION('center_axis',(0.,0.,1.));
#33239=DIRECTION('ref_axis',(0.984807753012208,0.17364817766693,0.));
#33240=DIRECTION('center_axis',(0.,0.,-1.));
#33241=DIRECTION('ref_axis',(1.,0.,0.));
#33242=DIRECTION('',(-0.905801965515955,-0.423701309022563,0.));
#33243=DIRECTION('',(0.996089805327885,-0.0883464754353932,0.));
#33244=DIRECTION('center_axis',(-0.0883464754353933,-0.996089805327885,
0.));
#33245=DIRECTION('ref_axis',(0.996089805327885,-0.0883464754353933,0.));
#33246=DIRECTION('',(0.,0.,1.));
#33247=DIRECTION('',(0.,0.,1.));
#33248=DIRECTION('center_axis',(-0.423701309022563,0.905801965515955,0.));
#33249=DIRECTION('ref_axis',(-0.905801965515954,-0.423701309022563,0.));
#33250=DIRECTION('',(0.,0.,-1.));
#33251=DIRECTION('center_axis',(0.,0.,1.));
#33252=DIRECTION('ref_axis',(1.,0.,0.));
#33253=DIRECTION('center_axis',(0.,0.,1.));
#33254=DIRECTION('ref_axis',(1.,0.,0.));
#33255=DIRECTION('center_axis',(0.,0.,1.));
#33256=DIRECTION('ref_axis',(1.,0.,0.));
#33257=DIRECTION('center_axis',(0.,0.,1.));
#33258=DIRECTION('ref_axis',(1.,0.,0.));
#33259=DIRECTION('center_axis',(0.,0.,1.));
#33260=DIRECTION('ref_axis',(1.,0.,0.));
#33261=DIRECTION('center_axis',(0.,0.,1.));
#33262=DIRECTION('ref_axis',(1.,0.,0.));
#33263=DIRECTION('center_axis',(0.,0.,1.));
#33264=DIRECTION('ref_axis',(1.,0.,0.));
#33265=DIRECTION('center_axis',(0.,0.,1.));
#33266=DIRECTION('ref_axis',(1.,0.,0.));
#33267=DIRECTION('center_axis',(0.,0.,1.));
#33268=DIRECTION('ref_axis',(1.,0.,0.));
#33269=DIRECTION('center_axis',(0.,0.,1.));
#33270=DIRECTION('ref_axis',(1.,0.,0.));
#33271=DIRECTION('center_axis',(0.,0.,1.));
#33272=DIRECTION('ref_axis',(1.,0.,0.));
#33273=DIRECTION('center_axis',(0.,0.,1.));
#33274=DIRECTION('ref_axis',(1.,0.,0.));
#33275=DIRECTION('center_axis',(0.,0.,1.));
#33276=DIRECTION('ref_axis',(1.,0.,0.));
#33277=DIRECTION('center_axis',(0.,0.,1.));
#33278=DIRECTION('ref_axis',(1.,0.,0.));
#33279=DIRECTION('center_axis',(0.,0.,1.));
#33280=DIRECTION('ref_axis',(1.,0.,0.));
#33281=DIRECTION('center_axis',(0.,0.,1.));
#33282=DIRECTION('ref_axis',(1.,0.,0.));
#33283=DIRECTION('center_axis',(0.,0.,1.));
#33284=DIRECTION('ref_axis',(1.,0.,0.));
#33285=DIRECTION('center_axis',(0.,0.,1.));
#33286=DIRECTION('ref_axis',(1.,0.,0.));
#33287=DIRECTION('',(0.,0.,-1.));
#33288=DIRECTION('center_axis',(0.,0.,1.));
#33289=DIRECTION('ref_axis',(1.,0.,0.));
#33290=DIRECTION('center_axis',(0.,0.,1.));
#33291=DIRECTION('ref_axis',(1.,0.,0.));
#33292=DIRECTION('center_axis',(0.,0.,1.));
#33293=DIRECTION('ref_axis',(1.,0.,0.));
#33294=DIRECTION('center_axis',(0.,0.,1.));
#33295=DIRECTION('ref_axis',(1.,0.,0.));
#33296=DIRECTION('center_axis',(0.,0.,1.));
#33297=DIRECTION('ref_axis',(1.,0.,0.));
#33298=DIRECTION('center_axis',(0.,0.,1.));
#33299=DIRECTION('ref_axis',(1.,0.,0.));
#33300=DIRECTION('center_axis',(0.,0.,1.));
#33301=DIRECTION('ref_axis',(1.,0.,0.));
#33302=DIRECTION('center_axis',(0.,0.,1.));
#33303=DIRECTION('ref_axis',(1.,0.,0.));
#33304=DIRECTION('center_axis',(0.,0.,1.));
#33305=DIRECTION('ref_axis',(1.,0.,0.));
#33306=DIRECTION('center_axis',(0.,0.,1.));
#33307=DIRECTION('ref_axis',(1.,0.,0.));
#33308=DIRECTION('center_axis',(0.,0.,1.));
#33309=DIRECTION('ref_axis',(1.,0.,0.));
#33310=DIRECTION('center_axis',(0.,0.,1.));
#33311=DIRECTION('ref_axis',(1.,0.,0.));
#33312=DIRECTION('center_axis',(0.,0.,1.));
#33313=DIRECTION('ref_axis',(1.,0.,0.));
#33314=DIRECTION('center_axis',(0.,0.,1.));
#33315=DIRECTION('ref_axis',(1.,0.,0.));
#33316=DIRECTION('center_axis',(0.,0.,1.));
#33317=DIRECTION('ref_axis',(1.,0.,0.));
#33318=DIRECTION('center_axis',(0.,0.,1.));
#33319=DIRECTION('ref_axis',(1.,0.,0.));
#33320=DIRECTION('center_axis',(0.,0.,1.));
#33321=DIRECTION('ref_axis',(1.,0.,0.));
#33322=DIRECTION('center_axis',(0.,0.,1.));
#33323=DIRECTION('ref_axis',(1.,0.,0.));
#33324=DIRECTION('center_axis',(0.,0.,1.));
#33325=DIRECTION('ref_axis',(1.,0.,0.));
#33326=DIRECTION('',(0.,0.,-1.));
#33327=DIRECTION('center_axis',(0.,0.,-1.));
#33328=DIRECTION('ref_axis',(1.,0.,0.));
#33329=DIRECTION('',(0.,0.,1.));
#33330=DIRECTION('center_axis',(0.,0.,1.));
#33331=DIRECTION('ref_axis',(1.,0.,0.));
#33332=DIRECTION('center_axis',(-0.259973473447872,-0.96561575852067,0.));
#33333=DIRECTION('ref_axis',(0.96561575852067,-0.259973473447872,0.));
#33334=DIRECTION('',(0.96561575852067,-0.259973473447872,0.));
#33335=DIRECTION('',(0.,0.,1.));
#33336=DIRECTION('center_axis',(-0.259973473447872,0.96561575852067,0.));
#33337=DIRECTION('ref_axis',(-0.96561575852067,-0.259973473447872,0.));
#33338=DIRECTION('',(-0.96561575852067,-0.259973473447872,0.));
#33339=DIRECTION('center_axis',(0.,0.,1.));
#33340=DIRECTION('ref_axis',(1.,0.,0.));
#33341=DIRECTION('center_axis',(0.,0.,-1.));
#33342=DIRECTION('ref_axis',(1.,0.,0.));
#33343=DIRECTION('center_axis',(0.,0.,1.));
#33344=DIRECTION('ref_axis',(1.,0.,0.));
#33345=DIRECTION('',(-0.707106781186548,-8.65956056235493E-17,-0.707106781186547));
#33346=DIRECTION('center_axis',(0.,0.,1.));
#33347=DIRECTION('ref_axis',(1.,0.,0.));
#33348=DIRECTION('',(-0.843867183172891,-1.03343924477817E-16,0.536552119708654));
#33349=DIRECTION('center_axis',(0.,0.,-1.));
#33350=DIRECTION('ref_axis',(1.,0.,0.));
#33351=DIRECTION('center_axis',(0.5,0.866025403784439,0.));
#33352=DIRECTION('ref_axis',(0.866025403784439,-0.5,0.));
#33353=DIRECTION('',(0.866025403784439,-0.5,0.));
#33354=DIRECTION('',(0.,0.,-1.));
#33355=DIRECTION('',(0.866025403784439,-0.5,0.));
#33356=DIRECTION('',(0.,0.,-1.));
#33357=DIRECTION('center_axis',(-0.5,0.866025403784439,0.));
#33358=DIRECTION('ref_axis',(0.866025403784439,0.5,0.));
#33359=DIRECTION('',(0.866025403784439,0.5,0.));
#33360=DIRECTION('',(0.,0.,-1.));
#33361=DIRECTION('',(0.866025403784439,0.5,0.));
#33362=DIRECTION('center_axis',(-1.,-1.20185167898973E-16,0.));
#33363=DIRECTION('ref_axis',(-1.20185167898973E-16,1.,0.));
#33364=DIRECTION('',(-1.20185167898973E-16,1.,0.));
#33365=DIRECTION('',(0.,0.,-1.));
#33366=DIRECTION('',(-1.20185167898973E-16,1.,0.));
#33367=DIRECTION('center_axis',(-0.5,-0.866025403784439,0.));
#33368=DIRECTION('ref_axis',(-0.866025403784439,0.5,0.));
#33369=DIRECTION('',(-0.866025403784439,0.5,0.));
#33370=DIRECTION('',(0.,0.,-1.));
#33371=DIRECTION('',(-0.866025403784439,0.5,0.));
#33372=DIRECTION('center_axis',(0.5,-0.866025403784439,0.));
#33373=DIRECTION('ref_axis',(-0.866025403784439,-0.5,0.));
#33374=DIRECTION('',(-0.866025403784439,-0.5,0.));
#33375=DIRECTION('',(0.,0.,-1.));
#33376=DIRECTION('',(-0.866025403784439,-0.5,0.));
#33377=DIRECTION('center_axis',(1.,-3.60555503696918E-16,0.));
#33378=DIRECTION('ref_axis',(-3.60555503696918E-16,-1.,0.));
#33379=DIRECTION('',(-3.60555503696918E-16,-1.,0.));
#33380=DIRECTION('',(-3.60555503696918E-16,-1.,0.));
#33381=DIRECTION('center_axis',(0.,0.,-1.));
#33382=DIRECTION('ref_axis',(-1.,0.,0.));
#33383=DIRECTION('center_axis',(0.,0.,-1.));
#33384=DIRECTION('ref_axis',(-1.,0.,0.));
#33385=DIRECTION('center_axis',(0.,0.,1.));
#33386=DIRECTION('ref_axis',(1.,0.,0.));
#33387=DIRECTION('center_axis',(0.,0.,1.));
#33388=DIRECTION('ref_axis',(1.,0.,0.));
#33389=DIRECTION('',(0.707106781186548,8.65956056235494E-17,-0.707106781186547));
#33390=DIRECTION('center_axis',(0.,0.,1.));
#33391=DIRECTION('ref_axis',(1.,0.,0.));
#33392=DIRECTION('center_axis',(0.,0.,1.));
#33393=DIRECTION('ref_axis',(1.,0.,0.));
#33394=DIRECTION('',(0.707106781186548,8.65956056235494E-17,-0.707106781186547));
#33395=DIRECTION('center_axis',(0.,0.,-1.));
#33396=DIRECTION('ref_axis',(-1.,0.,0.));
#33397=DIRECTION('center_axis',(0.,0.,1.));
#33398=DIRECTION('ref_axis',(1.,0.,0.));
#33399=DIRECTION('axis',(0.,0.,1.));
#33400=DIRECTION('refdir',(1.,0.,0.));
#33401=DIRECTION('center_axis',(0.,0.,1.));
#33402=DIRECTION('ref_axis',(1.,0.,0.));
#33403=DIRECTION('',(0.,0.,-1.));
#33404=DIRECTION('center_axis',(0.,0.,-1.));
#33405=DIRECTION('ref_axis',(1.,0.,0.));
#33406=DIRECTION('',(0.,0.,-1.));
#33407=DIRECTION('center_axis',(0.,0.,1.));
#33408=DIRECTION('ref_axis',(1.,0.,0.));
#33409=DIRECTION('center_axis',(0.,0.,-1.));
#33410=DIRECTION('ref_axis',(1.,0.,0.));
#33411=DIRECTION('center_axis',(0.,0.,1.));
#33412=DIRECTION('ref_axis',(1.,0.,0.));
#33413=DIRECTION('',(0.,0.,-1.));
#33414=DIRECTION('center_axis',(0.,0.,1.));
#33415=DIRECTION('ref_axis',(1.,0.,0.));
#33416=DIRECTION('',(0.,0.,-1.));
#33417=DIRECTION('center_axis',(0.,0.,1.));
#33418=DIRECTION('ref_axis',(1.,0.,0.));
#33419=DIRECTION('',(0.,0.,-1.));
#33420=DIRECTION('center_axis',(0.,0.,1.));
#33421=DIRECTION('ref_axis',(1.,0.,0.));
#33422=DIRECTION('',(0.,0.,-1.));
#33423=DIRECTION('center_axis',(0.,0.,1.));
#33424=DIRECTION('ref_axis',(1.,0.,0.));
#33425=DIRECTION('',(0.,0.,-1.));
#33426=DIRECTION('center_axis',(0.,0.,1.));
#33427=DIRECTION('ref_axis',(1.,0.,0.));
#33428=DIRECTION('',(0.,0.,-1.));
#33429=DIRECTION('center_axis',(0.,0.,1.));
#33430=DIRECTION('ref_axis',(-0.128707264998563,-0.991682630651858,0.));
#33431=DIRECTION('',(0.,0.,1.));
#33432=DIRECTION('center_axis',(0.,0.,1.));
#33433=DIRECTION('ref_axis',(1.,3.87383608070041E-14,0.));
#33434=DIRECTION('center_axis',(0.,0.,1.));
#33435=DIRECTION('ref_axis',(1.,3.87383608070041E-14,0.));
#33436=DIRECTION('',(0.,0.,1.));
#33437=DIRECTION('center_axis',(0.,0.,1.));
#33438=DIRECTION('ref_axis',(1.,3.87383608070041E-14,0.));
#33439=DIRECTION('',(0.,0.,1.));
#33440=DIRECTION('center_axis',(0.,0.,1.));
#33441=DIRECTION('ref_axis',(1.,3.87383608070041E-14,0.));
#33442=DIRECTION('',(0.,0.,1.));
#33443=DIRECTION('center_axis',(0.,0.,1.));
#33444=DIRECTION('ref_axis',(1.,3.87383608070041E-14,0.));
#33445=DIRECTION('',(0.,0.,1.));
#33446=DIRECTION('center_axis',(0.,0.,1.));
#33447=DIRECTION('ref_axis',(1.,3.87383608070041E-14,0.));
#33448=DIRECTION('',(0.,0.,1.));
#33449=DIRECTION('center_axis',(0.,0.,1.));
#33450=DIRECTION('ref_axis',(1.,3.87383608070041E-14,0.));
#33451=DIRECTION('',(0.,0.,1.));
#33452=DIRECTION('center_axis',(0.,0.,1.));
#33453=DIRECTION('ref_axis',(1.,3.87383608070041E-14,0.));
#33454=DIRECTION('',(0.,0.,1.));
#33455=DIRECTION('center_axis',(0.,0.,-1.));
#33456=DIRECTION('ref_axis',(1.,3.87383608070041E-14,0.));
#33457=DIRECTION('center_axis',(0.,0.,1.));
#33458=DIRECTION('ref_axis',(1.,0.,0.));
#33459=DIRECTION('center_axis',(0.,0.,-1.));
#33460=DIRECTION('ref_axis',(1.,3.87383608070041E-14,0.));
#33461=DIRECTION('center_axis',(0.,0.,1.));
#33462=DIRECTION('ref_axis',(1.,3.87383608070041E-14,0.));
#33463=DIRECTION('center_axis',(0.,-1.,0.));
#33464=DIRECTION('ref_axis',(1.,0.,0.));
#33465=DIRECTION('',(-1.,0.,0.));
#33466=DIRECTION('',(0.,0.,1.));
#33467=DIRECTION('',(1.,0.,0.));
#33468=DIRECTION('',(0.,0.,1.));
#33469=DIRECTION('center_axis',(1.,0.,0.));
#33470=DIRECTION('ref_axis',(0.,1.,0.));
#33471=DIRECTION('',(0.,-1.,0.));
#33472=DIRECTION('',(0.,0.,1.));
#33473=DIRECTION('',(0.,1.,0.));
#33474=DIRECTION('',(0.,0.,-1.));
#33475=DIRECTION('center_axis',(-1.,0.,0.));
#33476=DIRECTION('ref_axis',(0.,-1.,0.));
#33477=DIRECTION('',(0.,1.,0.));
#33478=DIRECTION('',(0.,0.,1.));
#33479=DIRECTION('',(0.,-1.,0.));
#33480=DIRECTION('',(0.,0.,1.));
#33481=DIRECTION('center_axis',(-1.,0.,0.));
#33482=DIRECTION('ref_axis',(0.,-1.,0.));
#33483=DIRECTION('',(0.,1.,0.));
#33484=DIRECTION('',(0.,-1.,0.));
#33485=DIRECTION('',(0.,0.,-1.));
#33486=DIRECTION('center_axis',(0.,1.,0.));
#33487=DIRECTION('ref_axis',(-1.,0.,0.));
#33488=DIRECTION('',(1.,0.,0.));
#33489=DIRECTION('',(-1.,0.,0.));
#33490=DIRECTION('center_axis',(1.,0.,0.));
#33491=DIRECTION('ref_axis',(0.,1.,0.));
#33492=DIRECTION('',(0.,-1.,0.));
#33493=DIRECTION('',(0.,0.,1.));
#33494=DIRECTION('',(0.,1.,0.));
#33495=DIRECTION('center_axis',(0.,0.,1.));
#33496=DIRECTION('ref_axis',(1.,0.,0.));
#33497=DIRECTION('center_axis',(0.,0.,1.));
#33498=DIRECTION('ref_axis',(1.,0.,0.));
#33499=DIRECTION('',(-1.,0.,0.));
#33500=DIRECTION('',(0.,1.,0.));
#33501=DIRECTION('',(1.,0.,0.));
#33502=DIRECTION('',(1.,0.,0.));
#33503=DIRECTION('',(0.,-1.,0.));
#33504=DIRECTION('',(-1.,0.,0.));
#33505=DIRECTION('center_axis',(0.,-1.,0.));
#33506=DIRECTION('ref_axis',(1.,0.,0.));
#33507=DIRECTION('',(1.,0.,0.));
#33508=DIRECTION('',(0.,0.,1.));
#33509=DIRECTION('center_axis',(0.,1.,0.));
#33510=DIRECTION('ref_axis',(-1.,0.,0.));
#33511=DIRECTION('',(0.,0.,1.));
#33512=DIRECTION('',(-1.,0.,0.));
#33513=DIRECTION('center_axis',(0.,1.,0.));
#33514=DIRECTION('ref_axis',(-1.,0.,0.));
#33515=DIRECTION('',(-1.,0.,0.));
#33516=DIRECTION('',(0.,0.,1.));
#33517=DIRECTION('center_axis',(0.,-1.,0.));
#33518=DIRECTION('ref_axis',(1.,0.,0.));
#33519=DIRECTION('',(0.,0.,1.));
#33520=DIRECTION('',(1.,0.,0.));
#33521=DIRECTION('center_axis',(-1.,0.,0.));
#33522=DIRECTION('ref_axis',(0.,-1.,0.));
#33523=DIRECTION('',(0.,-1.,0.));
#33524=DIRECTION('center_axis',(1.,0.,0.));
#33525=DIRECTION('ref_axis',(0.,1.,0.));
#33526=DIRECTION('',(0.,1.,0.));
#33527=DIRECTION('center_axis',(0.,0.,1.));
#33528=DIRECTION('ref_axis',(1.,0.,0.));
#33529=DIRECTION('center_axis',(0.,0.,-1.));
#33530=DIRECTION('ref_axis',(-1.,0.,0.));
#33531=DIRECTION('center_axis',(0.,0.,1.));
#33532=DIRECTION('ref_axis',(1.,0.,0.));
#33533=DIRECTION('center_axis',(0.,0.,1.));
#33534=DIRECTION('ref_axis',(1.,0.,0.));
#33535=DIRECTION('',(0.707106781186548,8.65956056235493E-17,-0.707106781186548));
#33536=DIRECTION('center_axis',(0.,0.,1.));
#33537=DIRECTION('ref_axis',(0.977648531888111,-0.210245922902257,0.));
#33538=DIRECTION('center_axis',(0.,0.,1.));
#33539=DIRECTION('ref_axis',(1.,0.,0.));
#33540=DIRECTION('center_axis',(0.,0.,-1.));
#33541=DIRECTION('ref_axis',(-1.,0.,0.));
#33542=DIRECTION('center_axis',(0.,0.,1.));
#33543=DIRECTION('ref_axis',(1.,0.,0.));
#33544=DIRECTION('center_axis',(0.,0.,1.));
#33545=DIRECTION('ref_axis',(1.,0.,0.));
#33546=DIRECTION('center_axis',(0.,0.,1.));
#33547=DIRECTION('ref_axis',(1.,0.,0.));
#33548=DIRECTION('',(0.,0.,-1.));
#33549=DIRECTION('center_axis',(0.,0.,-1.));
#33550=DIRECTION('ref_axis',(1.,0.,0.));
#33551=DIRECTION('',(-0.52999894000318,-6.49061505426384E-17,-0.847998304005088));
#33552=DIRECTION('axis',(0.,0.,1.));
#33553=DIRECTION('refdir',(1.,0.,0.));
#33554=DIRECTION('center_axis',(0.,0.,1.));
#33555=DIRECTION('ref_axis',(1.,0.,0.));
#33556=DIRECTION('',(0.,0.,-1.));
#33557=DIRECTION('center_axis',(0.,0.,-1.));
#33558=DIRECTION('ref_axis',(1.,0.,0.));
#33559=DIRECTION('',(0.,0.,-1.));
#33560=DIRECTION('center_axis',(0.,0.,1.));
#33561=DIRECTION('ref_axis',(1.,0.,0.));
#33562=DIRECTION('center_axis',(0.,0.,-1.));
#33563=DIRECTION('ref_axis',(1.,0.,0.));
#33564=DIRECTION('center_axis',(0.,0.,1.));
#33565=DIRECTION('ref_axis',(1.,0.,0.));
#33566=DIRECTION('',(0.,0.,-1.));
#33567=DIRECTION('center_axis',(0.,0.,1.));
#33568=DIRECTION('ref_axis',(1.,0.,0.));
#33569=DIRECTION('',(0.,0.,-1.));
#33570=DIRECTION('center_axis',(0.,0.,1.));
#33571=DIRECTION('ref_axis',(1.,0.,0.));
#33572=DIRECTION('',(0.,0.,-1.));
#33573=DIRECTION('center_axis',(0.,0.,1.));
#33574=DIRECTION('ref_axis',(1.,0.,0.));
#33575=DIRECTION('',(0.,0.,-1.));
#33576=DIRECTION('center_axis',(0.,0.,1.));
#33577=DIRECTION('ref_axis',(1.,0.,0.));
#33578=DIRECTION('',(0.,0.,-1.));
#33579=DIRECTION('center_axis',(0.,0.,1.));
#33580=DIRECTION('ref_axis',(1.,0.,0.));
#33581=DIRECTION('',(0.,0.,-1.));
#33582=DIRECTION('center_axis',(0.,0.,1.));
#33583=DIRECTION('ref_axis',(1.,0.,0.));
#33584=DIRECTION('',(0.,0.,-1.));
#33585=DIRECTION('center_axis',(0.,0.,1.));
#33586=DIRECTION('ref_axis',(1.,0.,0.));
#33587=DIRECTION('',(0.,0.,-1.));
#33588=DIRECTION('center_axis',(0.,0.,1.));
#33589=DIRECTION('ref_axis',(1.,0.,0.));
#33590=DIRECTION('',(0.,0.,-1.));
#33591=DIRECTION('center_axis',(0.,0.,1.));
#33592=DIRECTION('ref_axis',(1.,0.,0.));
#33593=DIRECTION('',(0.,0.,-1.));
#33594=DIRECTION('center_axis',(0.,0.,1.));
#33595=DIRECTION('ref_axis',(1.,0.,0.));
#33596=DIRECTION('',(0.,0.,-1.));
#33597=DIRECTION('center_axis',(0.,0.,1.));
#33598=DIRECTION('ref_axis',(1.,0.,0.));
#33599=DIRECTION('',(0.,0.,-1.));
#33600=DIRECTION('center_axis',(0.,0.,1.));
#33601=DIRECTION('ref_axis',(1.,0.,0.));
#33602=DIRECTION('',(0.,0.,-1.));
#33603=DIRECTION('center_axis',(0.,0.,1.));
#33604=DIRECTION('ref_axis',(1.,0.,0.));
#33605=DIRECTION('',(0.,0.,-1.));
#33606=DIRECTION('center_axis',(0.,0.,1.));
#33607=DIRECTION('ref_axis',(1.,0.,0.));
#33608=DIRECTION('',(0.,0.,-1.));
#33609=DIRECTION('center_axis',(0.,0.,1.));
#33610=DIRECTION('ref_axis',(1.,1.10752194731043E-13,0.));
#33611=DIRECTION('',(0.,0.,1.));
#33612=DIRECTION('center_axis',(0.,0.,1.));
#33613=DIRECTION('ref_axis',(1.,1.10752194731043E-13,0.));
#33614=DIRECTION('center_axis',(0.,0.,1.));
#33615=DIRECTION('ref_axis',(1.,1.10752194731043E-13,0.));
#33616=DIRECTION('',(0.,0.,1.));
#33617=DIRECTION('center_axis',(0.,0.,1.));
#33618=DIRECTION('ref_axis',(1.,1.10752194731043E-13,0.));
#33619=DIRECTION('center_axis',(0.,0.,1.));
#33620=DIRECTION('ref_axis',(1.,1.10752194731043E-13,0.));
#33621=DIRECTION('',(0.,0.,1.));
#33622=DIRECTION('center_axis',(0.,0.,1.));
#33623=DIRECTION('ref_axis',(1.,1.10752194731043E-13,0.));
#33624=DIRECTION('',(0.,0.,1.));
#33625=DIRECTION('center_axis',(0.,0.,1.));
#33626=DIRECTION('ref_axis',(1.,1.10752194731043E-13,0.));
#33627=DIRECTION('',(0.,0.,1.));
#33628=DIRECTION('center_axis',(0.,0.,1.));
#33629=DIRECTION('ref_axis',(1.,1.10752194731043E-13,0.));
#33630=DIRECTION('',(0.,0.,1.));
#33631=DIRECTION('center_axis',(0.,0.,1.));
#33632=DIRECTION('ref_axis',(1.,1.10752194731043E-13,0.));
#33633=DIRECTION('',(0.,0.,1.));
#33634=DIRECTION('center_axis',(0.,0.,1.));
#33635=DIRECTION('ref_axis',(1.,1.10752194731043E-13,0.));
#33636=DIRECTION('',(0.,0.,1.));
#33637=DIRECTION('center_axis',(0.,0.,1.));
#33638=DIRECTION('ref_axis',(1.,1.10752194731043E-13,0.));
#33639=DIRECTION('',(0.,0.,1.));
#33640=DIRECTION('center_axis',(0.,0.,1.));
#33641=DIRECTION('ref_axis',(1.,1.10752194731043E-13,0.));
#33642=DIRECTION('',(0.,0.,1.));
#33643=DIRECTION('center_axis',(0.,0.,1.));
#33644=DIRECTION('ref_axis',(1.,1.10752194731043E-13,0.));
#33645=DIRECTION('',(0.,0.,1.));
#33646=DIRECTION('center_axis',(0.,0.,1.));
#33647=DIRECTION('ref_axis',(1.,1.10752194731043E-13,0.));
#33648=DIRECTION('',(0.,0.,1.));
#33649=DIRECTION('center_axis',(0.,0.,1.));
#33650=DIRECTION('ref_axis',(1.,1.10752194731043E-13,0.));
#33651=DIRECTION('',(0.,0.,1.));
#33652=DIRECTION('center_axis',(0.,0.,1.));
#33653=DIRECTION('ref_axis',(1.,1.10752194731043E-13,0.));
#33654=DIRECTION('',(0.,0.,1.));
#33655=DIRECTION('center_axis',(0.,0.,1.));
#33656=DIRECTION('ref_axis',(1.,1.10752194731043E-13,0.));
#33657=DIRECTION('',(0.,0.,1.));
#33658=DIRECTION('center_axis',(0.,0.,1.));
#33659=DIRECTION('ref_axis',(1.,1.10752194731043E-13,0.));
#33660=DIRECTION('',(0.,0.,1.));
#33661=DIRECTION('center_axis',(0.,0.,1.));
#33662=DIRECTION('ref_axis',(1.,1.10752194731043E-13,0.));
#33663=DIRECTION('',(0.,0.,1.));
#33664=DIRECTION('center_axis',(0.,0.,-1.));
#33665=DIRECTION('ref_axis',(1.,1.10752194731043E-13,0.));
#33666=DIRECTION('center_axis',(0.,0.,1.));
#33667=DIRECTION('ref_axis',(1.,0.,0.));
#33668=DIRECTION('center_axis',(0.,0.,-1.));
#33669=DIRECTION('ref_axis',(1.,1.10752194731043E-13,0.));
#33670=DIRECTION('center_axis',(0.,0.,1.));
#33671=DIRECTION('ref_axis',(1.,1.10752194731043E-13,0.));
#33672=DIRECTION('center_axis',(0.,0.,1.));
#33673=DIRECTION('ref_axis',(1.,0.,0.));
#33674=DIRECTION('center_axis',(0.,0.,1.));
#33675=DIRECTION('ref_axis',(1.,0.,0.));
#33676=DIRECTION('center_axis',(0.,-1.,0.));
#33677=DIRECTION('ref_axis',(1.,0.,0.));
#33678=DIRECTION('',(-1.,0.,0.));
#33679=DIRECTION('',(0.,0.,1.));
#33680=DIRECTION('',(1.,0.,0.));
#33681=DIRECTION('',(0.,0.,1.));
#33682=DIRECTION('center_axis',(1.,0.,0.));
#33683=DIRECTION('ref_axis',(0.,1.,0.));
#33684=DIRECTION('',(0.,-1.,0.));
#33685=DIRECTION('',(0.,0.,1.));
#33686=DIRECTION('',(0.,1.,0.));
#33687=DIRECTION('',(0.,0.,-1.));
#33688=DIRECTION('center_axis',(-1.,0.,0.));
#33689=DIRECTION('ref_axis',(0.,-1.,0.));
#33690=DIRECTION('',(0.,1.,0.));
#33691=DIRECTION('',(0.,0.,1.));
#33692=DIRECTION('',(0.,-1.,0.));
#33693=DIRECTION('',(0.,0.,1.));
#33694=DIRECTION('center_axis',(-1.,0.,0.));
#33695=DIRECTION('ref_axis',(0.,-1.,0.));
#33696=DIRECTION('',(0.,1.,0.));
#33697=DIRECTION('',(0.,-1.,0.));
#33698=DIRECTION('',(0.,0.,-1.));
#33699=DIRECTION('center_axis',(0.,1.,0.));
#33700=DIRECTION('ref_axis',(-1.,0.,0.));
#33701=DIRECTION('',(1.,0.,0.));
#33702=DIRECTION('',(-1.,0.,0.));
#33703=DIRECTION('center_axis',(1.,0.,0.));
#33704=DIRECTION('ref_axis',(0.,1.,0.));
#33705=DIRECTION('',(0.,-1.,0.));
#33706=DIRECTION('',(0.,0.,1.));
#33707=DIRECTION('',(0.,1.,0.));
#33708=DIRECTION('center_axis',(0.,0.,1.));
#33709=DIRECTION('ref_axis',(1.,0.,0.));
#33710=DIRECTION('center_axis',(0.,0.,1.));
#33711=DIRECTION('ref_axis',(1.,0.,0.));
#33712=DIRECTION('',(-1.,0.,0.));
#33713=DIRECTION('',(0.,1.,0.));
#33714=DIRECTION('',(1.,0.,0.));
#33715=DIRECTION('',(1.,0.,0.));
#33716=DIRECTION('',(0.,-1.,0.));
#33717=DIRECTION('',(-1.,0.,0.));
#33718=DIRECTION('center_axis',(0.,-1.,0.));
#33719=DIRECTION('ref_axis',(1.,0.,0.));
#33720=DIRECTION('',(1.,0.,0.));
#33721=DIRECTION('',(0.,0.,1.));
#33722=DIRECTION('center_axis',(0.,1.,0.));
#33723=DIRECTION('ref_axis',(-1.,0.,0.));
#33724=DIRECTION('',(0.,0.,1.));
#33725=DIRECTION('',(-1.,0.,0.));
#33726=DIRECTION('center_axis',(0.,1.,0.));
#33727=DIRECTION('ref_axis',(-1.,0.,0.));
#33728=DIRECTION('',(-1.,0.,0.));
#33729=DIRECTION('',(0.,0.,1.));
#33730=DIRECTION('center_axis',(0.,-1.,0.));
#33731=DIRECTION('ref_axis',(1.,0.,0.));
#33732=DIRECTION('',(0.,0.,1.));
#33733=DIRECTION('',(1.,0.,0.));
#33734=DIRECTION('center_axis',(-1.,0.,0.));
#33735=DIRECTION('ref_axis',(0.,-1.,0.));
#33736=DIRECTION('',(0.,-1.,0.));
#33737=DIRECTION('center_axis',(1.,0.,0.));
#33738=DIRECTION('ref_axis',(0.,1.,0.));
#33739=DIRECTION('',(0.,1.,0.));
#33740=DIRECTION('center_axis',(0.,0.,1.));
#33741=DIRECTION('ref_axis',(1.,0.,0.));
#33742=DIRECTION('center_axis',(0.,0.,-1.));
#33743=DIRECTION('ref_axis',(-1.,0.,0.));
#33744=DIRECTION('center_axis',(0.,0.,1.));
#33745=DIRECTION('ref_axis',(1.,0.,0.));
#33746=DIRECTION('center_axis',(0.,0.,1.));
#33747=DIRECTION('ref_axis',(1.,0.,0.));
#33748=DIRECTION('',(0.707106781186548,8.65956056235493E-17,-0.707106781186548));
#33749=DIRECTION('center_axis',(0.,0.,-1.));
#33750=DIRECTION('ref_axis',(-1.,0.,0.));
#33751=DIRECTION('center_axis',(0.,0.,1.));
#33752=DIRECTION('ref_axis',(1.,0.,0.));
#33753=DIRECTION('center_axis',(0.,0.,1.));
#33754=DIRECTION('ref_axis',(1.,0.,0.));
#33755=DIRECTION('center_axis',(0.,0.,1.));
#33756=DIRECTION('ref_axis',(1.,0.,0.));
#33757=DIRECTION('',(0.,0.,-1.));
#33758=DIRECTION('center_axis',(0.,0.,-1.));
#33759=DIRECTION('ref_axis',(1.,0.,0.));
#33760=DIRECTION('',(-0.52999894000318,-6.49061505426384E-17,-0.847998304005088));
#33761=DIRECTION('',(0.,0.,1.));
#33762=DIRECTION('',(1.,0.,0.));
#33763=DIRECTION('',(0.,0.,1.));
#33764=DIRECTION('',(1.,0.,0.));
#33765=DIRECTION('',(0.,0.,1.));
#33766=DIRECTION('',(1.,0.,0.));
#33767=DIRECTION('',(0.,0.,1.));
#33768=DIRECTION('',(1.,0.,0.));
#33769=DIRECTION('',(0.,0.,1.));
#33770=DIRECTION('',(1.,0.,0.));
#33771=DIRECTION('',(0.,0.,1.));
#33772=DIRECTION('',(1.,0.,0.));
#33773=DIRECTION('',(0.,0.,1.));
#33774=DIRECTION('',(1.,0.,0.));
#33775=DIRECTION('',(0.,0.,1.));
#33776=DIRECTION('',(1.,0.,0.));
#33777=DIRECTION('',(0.,0.,1.));
#33778=DIRECTION('',(1.,0.,0.));
#33779=DIRECTION('',(0.,0.,1.));
#33780=DIRECTION('',(1.,0.,0.));
#33781=DIRECTION('',(0.,0.,1.));
#33782=DIRECTION('',(0.866025403784439,0.5,0.));
#33783=DIRECTION('',(0.,0.,1.));
#33784=DIRECTION('',(0.866025403784439,0.5,0.));
#33785=DIRECTION('',(0.,0.,1.));
#33786=DIRECTION('',(1.,0.,0.));
#33787=DIRECTION('',(0.,0.,1.));
#33788=DIRECTION('',(1.,0.,0.));
#33789=DIRECTION('',(0.,0.,1.));
#33790=DIRECTION('',(1.,0.,0.));
#33791=DIRECTION('',(0.,0.,1.));
#33792=DIRECTION('',(1.,0.,0.));
#33793=DIRECTION('',(0.,0.,-1.));
#33794=DIRECTION('',(1.,0.,0.));
#33795=DIRECTION('',(0.,0.,1.));
#33796=DIRECTION('',(1.,0.,0.));
#33797=DIRECTION('',(0.,0.,1.));
#33798=DIRECTION('',(1.,0.,0.));
#33799=DIRECTION('',(1.,0.,0.));
#33800=DIRECTION('',(0.,1.,0.));
#33801=DIRECTION('',(0.,0.,1.));
#33802=DIRECTION('',(1.,0.,0.));
#33803=DIRECTION('',(0.,0.,1.));
#33804=DIRECTION('',(1.,0.,0.));
#33805=DIRECTION('',(0.,0.,-1.));
#33806=DIRECTION('',(1.,0.,0.));
#33807=DIRECTION('',(0.,0.,-1.));
#33808=DIRECTION('',(1.,0.,0.));
#33809=DIRECTION('',(0.,0.,-1.));
#33810=DIRECTION('',(1.,0.,0.));
#33811=DIRECTION('',(0.,0.,1.));
#33812=DIRECTION('',(1.,0.,0.));
#33813=DIRECTION('',(0.,0.,1.));
#33814=DIRECTION('',(1.,0.,0.));
#33815=DIRECTION('',(0.,0.,1.));
#33816=DIRECTION('',(1.,0.,0.));
#33817=DIRECTION('',(0.,0.,1.));
#33818=DIRECTION('',(1.,0.,0.));
#33819=DIRECTION('',(0.,0.,1.));
#33820=DIRECTION('',(1.,0.,0.));
#33821=DIRECTION('',(0.,0.,1.));
#33822=DIRECTION('',(1.,0.,0.));
#33823=DIRECTION('',(0.,0.,1.));
#33824=DIRECTION('',(1.,0.,0.));
#33825=DIRECTION('',(0.,0.,1.));
#33826=DIRECTION('',(1.,0.,0.));
#33827=DIRECTION('',(0.,0.,1.));
#33828=DIRECTION('',(1.,0.,0.));
#33829=DIRECTION('',(0.,0.,1.));
#33830=DIRECTION('',(1.,0.,0.));
#33831=DIRECTION('',(0.,0.,1.));
#33832=DIRECTION('',(1.,0.,0.));
#33833=DIRECTION('',(0.,0.,-1.));
#33834=DIRECTION('',(1.,0.,0.));
#33835=DIRECTION('',(0.,0.,-1.));
#33836=DIRECTION('',(1.,0.,0.));
#33837=DIRECTION('',(0.,0.,-1.));
#33838=DIRECTION('',(1.,0.,0.));
#33839=DIRECTION('',(0.,0.,-1.));
#33840=DIRECTION('',(1.,0.,0.));
#33841=DIRECTION('',(0.,0.,-1.));
#33842=DIRECTION('',(1.,0.,0.));
#33843=DIRECTION('',(0.,0.,-1.));
#33844=DIRECTION('',(1.,0.,0.));
#33845=DIRECTION('',(0.,0.,1.));
#33846=DIRECTION('',(1.,0.,0.));
#33847=DIRECTION('',(0.,0.,-1.));
#33848=DIRECTION('',(1.,0.,0.));
#33849=DIRECTION('',(0.,0.,-1.));
#33850=DIRECTION('',(1.,0.,0.));
#33851=DIRECTION('',(0.,0.,1.));
#33852=DIRECTION('',(1.,0.,0.));
#33853=DIRECTION('',(0.,0.,1.));
#33854=DIRECTION('',(1.,0.,0.));
#33855=DIRECTION('',(0.,0.,1.));
#33856=DIRECTION('',(1.,0.,0.));
#33857=DIRECTION('',(0.,0.,1.));
#33858=DIRECTION('',(1.,0.,0.));
#33859=DIRECTION('',(0.,0.,1.));
#33860=DIRECTION('',(1.,0.,0.));
#33861=DIRECTION('',(0.,0.,1.));
#33862=DIRECTION('',(1.,0.,0.));
#33863=DIRECTION('',(-0.866025403784439,-0.5,0.));
#33864=DIRECTION('',(0.,0.,1.));
#33865=DIRECTION('',(-0.866025403784439,-0.5,0.));
#33866=DIRECTION('',(0.,0.,1.));
#33867=DIRECTION('',(0.,0.,1.));
#33868=DIRECTION('',(1.,0.,0.));
#33869=CARTESIAN_POINT('',(0.,0.,0.));
#33870=CARTESIAN_POINT('',(0.,0.,0.));
#33871=CARTESIAN_POINT('Origin',(0.,1.44777340356572E-16,0.0843933982822012));
#33872=CARTESIAN_POINT('',(4.7287867965644,1.15821872285257E-15,0.0587867965644029));
#33873=CARTESIAN_POINT('Origin',(0.,2.89554680713143E-16,0.0587867965644029));
#33874=CARTESIAN_POINT('',(4.75,-5.81707229594993E-16,0.11));
#33875=CARTESIAN_POINT('',(4.7393933982822,-2.90853614797496E-16,0.0843933982822012));
#33876=CARTESIAN_POINT('',(-4.75,-5.81707229594993E-16,0.11));
#33877=CARTESIAN_POINT('Origin',(0.,0.,0.11));
#33878=CARTESIAN_POINT('Origin',(0.,0.,0.11));
#33879=CARTESIAN_POINT('Origin',(0.,0.,0.04));
#33880=CARTESIAN_POINT('',(4.6912132034356,0.,0.0212132034355967));
#33881=CARTESIAN_POINT('',(4.71,5.76808642398403E-16,0.04));
#33882=CARTESIAN_POINT('Origin',(0.,2.8725396168526E-16,0.0212132034355967));
#33883=CARTESIAN_POINT('Origin',(0.,0.,0.7));
#33884=CARTESIAN_POINT('',(-4.75,-5.81707229594993E-16,0.65));
#33885=CARTESIAN_POINT('Origin',(0.,0.,0.65));
#33886=CARTESIAN_POINT('',(-4.75,-5.81707229594993E-16,0.7));
#33887=CARTESIAN_POINT('Origin',(0.,1.4362698084263E-16,1.3893933982822));
#33888=CARTESIAN_POINT('',(4.6912132034356,1.14901584674104E-15,1.3787867965644));
#33889=CARTESIAN_POINT('Origin',(0.,2.8725396168526E-16,1.3787867965644));
#33890=CARTESIAN_POINT('',(4.64,-5.68236114804372E-16,1.4));
#33891=CARTESIAN_POINT('',(4.6656066017178,-2.84118057402186E-16,1.3893933982822));
#33892=CARTESIAN_POINT('Origin',(0.,0.,1.4));
#33893=CARTESIAN_POINT('Origin',(0.,0.,1.36));
#33894=CARTESIAN_POINT('',(4.7287867965644,0.,1.3412132034356));
#33895=CARTESIAN_POINT('',(4.71,5.76808642398403E-16,1.36));
#33896=CARTESIAN_POINT('Origin',(0.,2.89554680713143E-16,1.3412132034356));
#33897=CARTESIAN_POINT('Origin',(4.095,0.,1.4));
#33898=CARTESIAN_POINT('',(-4.095,-5.01492864250841E-16,1.4));
#33899=CARTESIAN_POINT('Origin',(0.,0.,1.4));
#33900=CARTESIAN_POINT('',(4.44833333333333,-1.57163005890577E-17,1.4));
#33901=CARTESIAN_POINT('Origin',(4.32,0.,1.4));
#33902=CARTESIAN_POINT('',(2.28833333333333,3.74122974434878,1.4));
#33903=CARTESIAN_POINT('Origin',(2.16,3.74122974434878,1.4));
#33904=CARTESIAN_POINT('',(-2.03166666666667,3.74122974434878,1.4));
#33905=CARTESIAN_POINT('Origin',(-2.16,3.74122974434878,1.4));
#33906=CARTESIAN_POINT('',(-4.19166666666667,5.13331116642599E-16,1.4));
#33907=CARTESIAN_POINT('Origin',(-4.32,5.29047417231657E-16,1.4));
#33908=CARTESIAN_POINT('',(-2.03166666666667,-3.74122974434877,1.4));
#33909=CARTESIAN_POINT('Origin',(-2.16,-3.74122974434877,1.4));
#33910=CARTESIAN_POINT('',(2.28833333333333,-3.74122974434878,1.4));
#33911=CARTESIAN_POINT('Origin',(2.16,-3.74122974434878,1.4));
#33912=CARTESIAN_POINT('Origin',(0.,1.4362698084263E-16,0.0106066017177983));
#33913=CARTESIAN_POINT('',(4.64,5.68236114804372E-16,0.));
#33914=CARTESIAN_POINT('',(4.6656066017178,8.58625980772706E-16,0.0106066017177983));
#33915=CARTESIAN_POINT('Origin',(0.,0.,0.));
#33916=CARTESIAN_POINT('Origin',(4.75,0.,0.));
#33917=CARTESIAN_POINT('',(0.78,-9.55224503334935E-17,0.));
#33918=CARTESIAN_POINT('Origin',(0.,0.,0.));
#33919=CARTESIAN_POINT('',(1.92,3.74122974434878,0.));
#33920=CARTESIAN_POINT('Origin',(2.16,3.74122974434878,0.));
#33921=CARTESIAN_POINT('',(-4.56,5.58438940411193E-16,0.));
#33922=CARTESIAN_POINT('Origin',(-4.32,5.29047417231657E-16,0.));
#33923=CARTESIAN_POINT('',(1.92,-3.74122974434878,0.));
#33924=CARTESIAN_POINT('Origin',(2.16,-3.74122974434878,0.));
#33925=CARTESIAN_POINT('',(-2.4,-3.74122974434877,0.));
#33926=CARTESIAN_POINT('Origin',(-2.16,-3.74122974434877,0.));
#33927=CARTESIAN_POINT('',(-2.4,3.74122974434878,0.));
#33928=CARTESIAN_POINT('Origin',(-2.16,3.74122974434878,0.));
#33929=CARTESIAN_POINT('',(4.08,2.93915231795365E-17,0.));
#33930=CARTESIAN_POINT('Origin',(4.32,0.,0.));
#33931=CARTESIAN_POINT('Origin',(0.,-2.23126604418363E-17,0.0106066017177982));
#33932=CARTESIAN_POINT('',(0.728786796564404,0.,0.0212132034355964));
#33933=CARTESIAN_POINT('Origin',(0.,-4.46253208836725E-17,0.0212132034355964));
#33934=CARTESIAN_POINT('',(0.754393398282202,4.77612251667468E-17,0.0106066017177982));
#33935=CARTESIAN_POINT('Origin',(0.,0.,0.025));
#33936=CARTESIAN_POINT('',(0.721213203435596,-1.76646288218042E-16,0.0287867965644036));
#33937=CARTESIAN_POINT('',(0.725,-8.87868929381831E-17,0.025));
#33938=CARTESIAN_POINT('Origin',(0.,-4.41615720545106E-17,0.0287867965644036));
#33939=CARTESIAN_POINT('Origin',(0.,-2.20807860272553E-17,0.0543933982822019));
#33940=CARTESIAN_POINT('',(0.7,8.57252759403147E-17,0.0800000000000001));
#33941=CARTESIAN_POINT('',(0.710606601717798,-1.31185782079179E-16,0.0543933982822019));
#33942=CARTESIAN_POINT('',(-0.7,-8.57252759403147E-17,0.0800000000000001));
#33943=CARTESIAN_POINT('Origin',(0.,0.,0.0800000000000001));
#33944=CARTESIAN_POINT('Origin',(0.,0.,0.0800000000000001));
#33945=CARTESIAN_POINT('Origin',(0.,0.,1.));
#33946=CARTESIAN_POINT('',(0.7,-8.57252759403147E-17,1.92));
#33947=CARTESIAN_POINT('',(-0.7,-8.57252759403147E-17,1.92));
#33948=CARTESIAN_POINT('Origin',(0.,0.,1.92));
#33949=CARTESIAN_POINT('Origin',(0.,0.,1.92));
#33950=CARTESIAN_POINT('',(-0.7,-8.57252759403147E-17,1.));
#33951=CARTESIAN_POINT('Origin',(0.,-2.20807860272553E-17,1.9456066017178));
#33952=CARTESIAN_POINT('',(0.721213203435596,0.,1.9712132034356));
#33953=CARTESIAN_POINT('Origin',(0.,-4.41615720545106E-17,1.9712132034356));
#33954=CARTESIAN_POINT('',(0.710606601717798,4.28626379701574E-17,1.9456066017178));
#33955=CARTESIAN_POINT('Origin',(0.,0.,1.975));
#33956=CARTESIAN_POINT('',(0.728786796564404,-1.7850128353469E-16,1.9787867965644));
#33957=CARTESIAN_POINT('',(0.725,-8.87868929381831E-17,1.975));
#33958=CARTESIAN_POINT('Origin',(0.,-4.46253208836725E-17,1.9787867965644));
#33959=CARTESIAN_POINT('Origin',(0.,-2.23126604418363E-17,1.9893933982822));
#33960=CARTESIAN_POINT('',(0.78,9.55224503334936E-17,2.));
#33961=CARTESIAN_POINT('',(0.754393398282202,-1.37011866934092E-16,1.9893933982822));
#33962=CARTESIAN_POINT('Origin',(0.,0.,2.));
#33963=CARTESIAN_POINT('Origin',(0.7,0.,2.));
#33964=CARTESIAN_POINT('',(4.055,-4.96594277054252E-16,2.));
#33965=CARTESIAN_POINT('Origin',(0.,0.,2.));
#33966=CARTESIAN_POINT('',(-0.18,3.4,2.));
#33967=CARTESIAN_POINT('Origin',(2.0818995585505E-16,3.4,2.));
#33968=CARTESIAN_POINT('',(-3.12448637286709,-1.7,2.));
#33969=CARTESIAN_POINT('Origin',(-2.94448637286709,-1.7,2.));
#33970=CARTESIAN_POINT('',(2.76448637286709,-1.7,2.));
#33971=CARTESIAN_POINT('Origin',(2.94448637286709,-1.7,2.));
#33972=CARTESIAN_POINT('Origin',(4.32,0.,0.015));
#33973=CARTESIAN_POINT('',(4.11,-2.57175827820944E-17,0.03));
#33974=CARTESIAN_POINT('',(4.095,2.75545529808155E-17,0.015));
#33975=CARTESIAN_POINT('',(4.53,-2.57175827820944E-17,0.03));
#33976=CARTESIAN_POINT('Origin',(4.32,0.,0.03));
#33977=CARTESIAN_POINT('Origin',(4.32,0.,0.03));
#33978=CARTESIAN_POINT('Origin',(4.32,0.,0.25));
#33979=CARTESIAN_POINT('',(4.53,-2.57175827820944E-17,0.5));
#33980=CARTESIAN_POINT('Origin',(4.32,0.,0.5));
#33981=CARTESIAN_POINT('',(4.53,-2.57175827820944E-17,0.25));
#33982=CARTESIAN_POINT('Origin',(2.16,3.74122974434878,0.015));
#33983=CARTESIAN_POINT('',(1.95,3.74122974434878,0.03));
#33984=CARTESIAN_POINT('',(1.935,3.74122974434878,0.015));
#33985=CARTESIAN_POINT('',(2.37,3.74122974434878,0.03));
#33986=CARTESIAN_POINT('Origin',(2.16,3.74122974434878,0.03));
#33987=CARTESIAN_POINT('Origin',(2.16,3.74122974434878,0.03));
#33988=CARTESIAN_POINT('Origin',(2.16,3.74122974434878,0.25));
#33989=CARTESIAN_POINT('',(2.37,3.74122974434878,0.5));
#33990=CARTESIAN_POINT('Origin',(2.16,3.74122974434878,0.5));
#33991=CARTESIAN_POINT('',(2.37,3.74122974434878,0.25));
#33992=CARTESIAN_POINT('Origin',(-2.16,3.74122974434878,0.015));
#33993=CARTESIAN_POINT('',(-2.37,3.74122974434878,0.03));
#33994=CARTESIAN_POINT('',(-2.385,3.74122974434878,0.015));
#33995=CARTESIAN_POINT('',(-1.95,3.74122974434878,0.03));
#33996=CARTESIAN_POINT('Origin',(-2.16,3.74122974434878,0.03));
#33997=CARTESIAN_POINT('Origin',(-2.16,3.74122974434878,0.03));
#33998=CARTESIAN_POINT('Origin',(-2.16,3.74122974434878,0.25));
#33999=CARTESIAN_POINT('',(-1.95,3.74122974434878,0.5));
#34000=CARTESIAN_POINT('Origin',(-2.16,3.74122974434878,0.5));
#34001=CARTESIAN_POINT('',(-1.95,3.74122974434878,0.25));
#34002=CARTESIAN_POINT('Origin',(-4.32,5.29047417231657E-16,0.015));
#34003=CARTESIAN_POINT('',(-4.53,5.03329834449562E-16,0.03));
#34004=CARTESIAN_POINT('',(-4.545,5.56601970212472E-16,0.015));
#34005=CARTESIAN_POINT('',(-4.11,5.03329834449562E-16,0.03));
#34006=CARTESIAN_POINT('Origin',(-4.32,5.29047417231657E-16,0.03));
#34007=CARTESIAN_POINT('Origin',(-4.32,5.29047417231657E-16,0.03));
#34008=CARTESIAN_POINT('Origin',(-4.32,5.29047417231657E-16,0.25));
#34009=CARTESIAN_POINT('',(-4.11,5.03329834449562E-16,0.5));
#34010=CARTESIAN_POINT('Origin',(-4.32,5.29047417231657E-16,0.5));
#34011=CARTESIAN_POINT('',(-4.11,5.03329834449562E-16,0.25));
#34012=CARTESIAN_POINT('Origin',(-2.16,-3.74122974434877,0.015));
#34013=CARTESIAN_POINT('',(-2.37,-3.74122974434877,0.03));
#34014=CARTESIAN_POINT('',(-2.385,-3.74122974434877,0.015));
#34015=CARTESIAN_POINT('',(-1.95,-3.74122974434877,0.03));
#34016=CARTESIAN_POINT('Origin',(-2.16,-3.74122974434877,0.03));
#34017=CARTESIAN_POINT('Origin',(-2.16,-3.74122974434877,0.03));
#34018=CARTESIAN_POINT('Origin',(-2.16,-3.74122974434877,0.25));
#34019=CARTESIAN_POINT('',(-1.95,-3.74122974434877,0.5));
#34020=CARTESIAN_POINT('Origin',(-2.16,-3.74122974434877,0.5));
#34021=CARTESIAN_POINT('',(-1.95,-3.74122974434877,0.25));
#34022=CARTESIAN_POINT('Origin',(2.16,-3.74122974434878,0.015));
#34023=CARTESIAN_POINT('',(1.95,-3.74122974434878,0.03));
#34024=CARTESIAN_POINT('',(1.935,-3.74122974434878,0.015));
#34025=CARTESIAN_POINT('',(2.37,-3.74122974434878,0.03));
#34026=CARTESIAN_POINT('Origin',(2.16,-3.74122974434878,0.03));
#34027=CARTESIAN_POINT('Origin',(2.16,-3.74122974434878,0.03));
#34028=CARTESIAN_POINT('Origin',(2.16,-3.74122974434878,0.25));
#34029=CARTESIAN_POINT('',(2.37,-3.74122974434878,0.5));
#34030=CARTESIAN_POINT('Origin',(2.16,-3.74122974434878,0.5));
#34031=CARTESIAN_POINT('',(2.37,-3.74122974434878,0.25));
#34032=CARTESIAN_POINT('Origin',(0.,1.44777340356572E-16,1.3156066017178));
#34033=CARTESIAN_POINT('',(4.75,5.81707229594993E-16,1.29));
#34034=CARTESIAN_POINT('',(4.7393933982822,8.69962976223783E-16,1.3156066017178));
#34035=CARTESIAN_POINT('',(-4.75,-5.81707229594993E-16,1.29));
#34036=CARTESIAN_POINT('Origin',(0.,0.,1.29));
#34037=CARTESIAN_POINT('Origin',(0.,0.,1.29));
#34038=CARTESIAN_POINT('Origin',(0.,0.,0.7));
#34039=CARTESIAN_POINT('',(-4.75,5.81707229594993E-16,0.77));
#34040=CARTESIAN_POINT('',(-4.75,-5.81707229594993E-16,0.7));
#34041=CARTESIAN_POINT('Origin',(0.,0.,0.77));
#34042=CARTESIAN_POINT('Origin',(0.,0.,0.755));
#34043=CARTESIAN_POINT('',(-4.72,-5.78033289197551E-16,0.74));
#34044=CARTESIAN_POINT('',(-4.735,-5.79870259396272E-16,0.755));
#34045=CARTESIAN_POINT('Origin',(0.,0.,0.74));
#34046=CARTESIAN_POINT('Origin',(4.66,0.,0.74));
#34047=CARTESIAN_POINT('',(-4.66,-5.70685408402667E-16,0.74));
#34048=CARTESIAN_POINT('Origin',(0.,0.,0.74));
#34049=CARTESIAN_POINT('Origin',(0.,0.,0.665));
#34050=CARTESIAN_POINT('',(-4.72,5.78033289197551E-16,0.68));
#34051=CARTESIAN_POINT('',(-4.735,5.79870259396272E-16,0.665));
#34052=CARTESIAN_POINT('Origin',(0.,0.,0.68));
#34053=CARTESIAN_POINT('Origin',(4.8,0.,0.68));
#34054=CARTESIAN_POINT('',(-4.66,-5.70685408402667E-16,0.68));
#34055=CARTESIAN_POINT('Origin',(0.,0.,0.68));
#34056=CARTESIAN_POINT('Origin',(0.,0.,0.71));
#34057=CARTESIAN_POINT('',(-4.66,-5.70685408402667E-16,0.71));
#34058=CARTESIAN_POINT('Origin',(2.94448637286709,-1.7,1.36094405976321));
#34059=CARTESIAN_POINT('',(2.94448637286709,-1.7,1.32188811952642));
#34060=CARTESIAN_POINT('',(2.81448637286709,-1.7,1.4));
#34061=CARTESIAN_POINT('',(2.87948637286709,-1.7,1.36094405976321));
#34062=CARTESIAN_POINT('Origin',(2.94448637286709,-1.7,1.4));
#34063=CARTESIAN_POINT('Origin',(2.94448637286709,-1.7,1.675));
#34064=CARTESIAN_POINT('',(2.81448637286709,-1.7,1.95));
#34065=CARTESIAN_POINT('',(2.81448637286709,-1.7,1.675));
#34066=CARTESIAN_POINT('Origin',(2.94448637286709,-1.7,1.95));
#34067=CARTESIAN_POINT('Origin',(2.94448637286709,-1.7,2.));
#34068=CARTESIAN_POINT('',(2.76448637286709,-1.7,2.));
#34069=CARTESIAN_POINT('Origin',(-2.94448637286709,-1.7,1.36094405976321));
#34070=CARTESIAN_POINT('',(-2.94448637286709,-1.7,1.32188811952642));
#34071=CARTESIAN_POINT('',(-3.07448637286709,-1.7,1.4));
#34072=CARTESIAN_POINT('',(-3.00948637286709,-1.7,1.36094405976321));
#34073=CARTESIAN_POINT('Origin',(-2.94448637286709,-1.7,1.4));
#34074=CARTESIAN_POINT('Origin',(-2.94448637286709,-1.7,1.675));
#34075=CARTESIAN_POINT('',(-3.07448637286709,-1.7,1.95));
#34076=CARTESIAN_POINT('',(-3.07448637286709,-1.7,1.675));
#34077=CARTESIAN_POINT('Origin',(-2.94448637286709,-1.7,1.95));
#34078=CARTESIAN_POINT('Origin',(-2.94448637286709,-1.7,2.));
#34079=CARTESIAN_POINT('',(-3.12448637286709,-1.7,2.));
#34080=CARTESIAN_POINT('Origin',(2.0818995585505E-16,3.4,1.36094405976321));
#34081=CARTESIAN_POINT('',(2.0818995585505E-16,3.4,1.32188811952642));
#34082=CARTESIAN_POINT('',(-0.13,3.4,1.4));
#34083=CARTESIAN_POINT('',(-0.0649999999999998,3.4,1.36094405976321));
#34084=CARTESIAN_POINT('Origin',(2.0818995585505E-16,3.4,1.4));
#34085=CARTESIAN_POINT('Origin',(2.0818995585505E-16,3.4,1.675));
#34086=CARTESIAN_POINT('',(-0.13,3.4,1.95));
#34087=CARTESIAN_POINT('',(-0.13,3.4,1.675));
#34088=CARTESIAN_POINT('Origin',(2.0818995585505E-16,3.4,1.95));
#34089=CARTESIAN_POINT('Origin',(2.0818995585505E-16,3.4,2.));
#34090=CARTESIAN_POINT('',(-0.18,3.4,2.));
#34091=CARTESIAN_POINT('Origin',(2.16,-3.74122974434878,1.4125));
#34092=CARTESIAN_POINT('',(2.28,-3.74122974434878,1.375));
#34093=CARTESIAN_POINT('',(2.2925,-3.74122974434878,1.4125));
#34094=CARTESIAN_POINT('Origin',(2.16,-3.74122974434878,1.375));
#34095=CARTESIAN_POINT('Origin',(2.16,-3.74122974434878,0.95));
#34096=CARTESIAN_POINT('',(2.28,-3.74122974434878,0.525));
#34097=CARTESIAN_POINT('',(2.28,-3.74122974434878,0.95));
#34098=CARTESIAN_POINT('Origin',(2.16,-3.74122974434878,0.525));
#34099=CARTESIAN_POINT('Origin',(2.16,-3.74122974434878,0.5125));
#34100=CARTESIAN_POINT('',(2.305,-3.74122974434878,0.5));
#34101=CARTESIAN_POINT('',(2.2925,-3.74122974434878,0.5125));
#34102=CARTESIAN_POINT('Origin',(2.16,-3.74122974434878,0.5));
#34103=CARTESIAN_POINT('Origin',(1.95,-3.74122974434878,0.5));
#34104=CARTESIAN_POINT('Origin',(-2.16,-3.74122974434877,1.4125));
#34105=CARTESIAN_POINT('',(-2.04,-3.74122974434877,1.375));
#34106=CARTESIAN_POINT('',(-2.0275,-3.74122974434877,1.4125));
#34107=CARTESIAN_POINT('Origin',(-2.16,-3.74122974434877,1.375));
#34108=CARTESIAN_POINT('Origin',(-2.16,-3.74122974434877,0.95));
#34109=CARTESIAN_POINT('',(-2.04,-3.74122974434877,0.525));
#34110=CARTESIAN_POINT('',(-2.04,-3.74122974434877,0.95));
#34111=CARTESIAN_POINT('Origin',(-2.16,-3.74122974434877,0.525));
#34112=CARTESIAN_POINT('Origin',(-2.16,-3.74122974434877,0.5125));
#34113=CARTESIAN_POINT('',(-2.015,-3.74122974434877,0.5));
#34114=CARTESIAN_POINT('',(-2.0275,-3.74122974434877,0.5125));
#34115=CARTESIAN_POINT('Origin',(-2.16,-3.74122974434877,0.5));
#34116=CARTESIAN_POINT('Origin',(-2.37,-3.74122974434877,0.5));
#34117=CARTESIAN_POINT('Origin',(-4.32,5.29047417231657E-16,1.4125));
#34118=CARTESIAN_POINT('',(-4.2,5.14351655641888E-16,1.375));
#34119=CARTESIAN_POINT('',(-4.1875,5.12820847142954E-16,1.4125));
#34120=CARTESIAN_POINT('Origin',(-4.32,5.29047417231657E-16,1.375));
#34121=CARTESIAN_POINT('Origin',(-4.32,5.29047417231657E-16,0.95));
#34122=CARTESIAN_POINT('',(-4.2,5.14351655641888E-16,0.525));
#34123=CARTESIAN_POINT('',(-4.2,5.14351655641888E-16,0.95));
#34124=CARTESIAN_POINT('Origin',(-4.32,5.29047417231657E-16,0.525));
#34125=CARTESIAN_POINT('Origin',(-4.32,5.29047417231657E-16,0.5125));
#34126=CARTESIAN_POINT('',(-4.175,5.1129003864402E-16,0.5));
#34127=CARTESIAN_POINT('',(-4.1875,5.12820847142954E-16,0.5125));
#34128=CARTESIAN_POINT('Origin',(-4.32,5.29047417231657E-16,0.5));
#34129=CARTESIAN_POINT('Origin',(-4.53,5.29047417231657E-16,0.5));
#34130=CARTESIAN_POINT('Origin',(-2.16,3.74122974434878,1.4125));
#34131=CARTESIAN_POINT('',(-2.04,3.74122974434878,1.375));
#34132=CARTESIAN_POINT('',(-2.0275,3.74122974434878,1.4125));
#34133=CARTESIAN_POINT('Origin',(-2.16,3.74122974434878,1.375));
#34134=CARTESIAN_POINT('Origin',(-2.16,3.74122974434878,0.95));
#34135=CARTESIAN_POINT('',(-2.04,3.74122974434878,0.525));
#34136=CARTESIAN_POINT('',(-2.04,3.74122974434878,0.95));
#34137=CARTESIAN_POINT('Origin',(-2.16,3.74122974434878,0.525));
#34138=CARTESIAN_POINT('Origin',(-2.16,3.74122974434878,0.5125));
#34139=CARTESIAN_POINT('',(-2.015,3.74122974434878,0.5));
#34140=CARTESIAN_POINT('',(-2.0275,3.74122974434878,0.5125));
#34141=CARTESIAN_POINT('Origin',(-2.16,3.74122974434878,0.5));
#34142=CARTESIAN_POINT('Origin',(-2.37,3.74122974434878,0.5));
#34143=CARTESIAN_POINT('Origin',(2.16,3.74122974434878,1.4125));
#34144=CARTESIAN_POINT('',(2.28,3.74122974434878,1.375));
#34145=CARTESIAN_POINT('',(2.2925,3.74122974434878,1.4125));
#34146=CARTESIAN_POINT('Origin',(2.16,3.74122974434878,1.375));
#34147=CARTESIAN_POINT('Origin',(2.16,3.74122974434878,0.95));
#34148=CARTESIAN_POINT('',(2.28,3.74122974434878,0.525));
#34149=CARTESIAN_POINT('',(2.28,3.74122974434878,0.95));
#34150=CARTESIAN_POINT('Origin',(2.16,3.74122974434878,0.525));
#34151=CARTESIAN_POINT('Origin',(2.16,3.74122974434878,0.5125));
#34152=CARTESIAN_POINT('',(2.305,3.74122974434878,0.5));
#34153=CARTESIAN_POINT('',(2.2925,3.74122974434878,0.5125));
#34154=CARTESIAN_POINT('Origin',(2.16,3.74122974434878,0.5));
#34155=CARTESIAN_POINT('Origin',(1.95,3.74122974434878,0.5));
#34156=CARTESIAN_POINT('Origin',(4.32,0.,1.4125));
#34157=CARTESIAN_POINT('',(4.44,-1.46957615897682E-17,1.375));
#34158=CARTESIAN_POINT('',(4.4525,-1.62265700887025E-17,1.4125));
#34159=CARTESIAN_POINT('Origin',(4.32,0.,1.375));
#34160=CARTESIAN_POINT('Origin',(4.32,0.,0.95));
#34161=CARTESIAN_POINT('',(4.44,-1.46957615897683E-17,0.525));
#34162=CARTESIAN_POINT('',(4.44,-1.46957615897683E-17,0.95));
#34163=CARTESIAN_POINT('Origin',(4.32,0.,0.525));
#34164=CARTESIAN_POINT('Origin',(4.32,0.,0.5125));
#34165=CARTESIAN_POINT('',(4.465,-1.77573785876367E-17,0.5));
#34166=CARTESIAN_POINT('',(4.4525,-1.62265700887025E-17,0.5125));
#34167=CARTESIAN_POINT('Origin',(4.32,0.,0.5));
#34168=CARTESIAN_POINT('Origin',(4.11,0.,0.5));
#34169=CARTESIAN_POINT('Origin',(0.,0.,1.98));
#34170=CARTESIAN_POINT('',(4.095,5.01492864250841E-16,1.96));
#34171=CARTESIAN_POINT('',(4.075,4.99043570652547E-16,1.98));
#34172=CARTESIAN_POINT('',(-4.095,-5.01492864250841E-16,1.96));
#34173=CARTESIAN_POINT('Origin',(0.,0.,1.96));
#34174=CARTESIAN_POINT('Origin',(0.,0.,1.96));
#34175=CARTESIAN_POINT('Origin',(0.,0.,1.7));
#34176=CARTESIAN_POINT('',(-4.095,-5.01492864250841E-16,1.7));
#34177=CARTESIAN_POINT('',(0.,0.,0.));
#34178=CARTESIAN_POINT('Origin',(2.16,-3.74122974434878,2.23154518249895));
#34179=CARTESIAN_POINT('',(2.16,-3.74122974434878,2.26309036499789));
#34180=CARTESIAN_POINT('',(2.265,-3.74122974434878,2.2));
#34181=CARTESIAN_POINT('',(2.2125,-3.74122974434878,2.23154518249895));
#34182=CARTESIAN_POINT('Origin',(2.16,-3.74122974434878,2.2));
#34183=CARTESIAN_POINT('Origin',(2.16,-3.74122974434878,1.825));
#34184=CARTESIAN_POINT('',(2.265,-3.74122974434878,1.45));
#34185=CARTESIAN_POINT('',(2.265,-3.74122974434878,1.825));
#34186=CARTESIAN_POINT('Origin',(2.16,-3.74122974434878,1.45));
#34187=CARTESIAN_POINT('Origin',(2.16,-3.74122974434878,1.4));
#34188=CARTESIAN_POINT('',(2.315,-3.74122974434878,1.4));
#34189=CARTESIAN_POINT('',(2.315,-3.74122974434878,1.4));
#34190=CARTESIAN_POINT('Origin',(2.16,-3.74122974434878,1.4));
#34191=CARTESIAN_POINT('Origin',(-2.16,-3.74122974434877,2.23154518249895));
#34192=CARTESIAN_POINT('',(-2.16,-3.74122974434877,2.26309036499789));
#34193=CARTESIAN_POINT('',(-2.055,-3.74122974434877,2.2));
#34194=CARTESIAN_POINT('',(-2.1075,-3.74122974434877,2.23154518249895));
#34195=CARTESIAN_POINT('Origin',(-2.16,-3.74122974434877,2.2));
#34196=CARTESIAN_POINT('Origin',(-2.16,-3.74122974434877,1.825));
#34197=CARTESIAN_POINT('',(-2.055,-3.74122974434877,1.45));
#34198=CARTESIAN_POINT('',(-2.055,-3.74122974434877,1.825));
#34199=CARTESIAN_POINT('Origin',(-2.16,-3.74122974434877,1.45));
#34200=CARTESIAN_POINT('Origin',(-2.16,-3.74122974434877,1.4));
#34201=CARTESIAN_POINT('',(-2.005,-3.74122974434877,1.4));
#34202=CARTESIAN_POINT('',(-2.005,-3.74122974434877,1.4));
#34203=CARTESIAN_POINT('Origin',(-2.16,-3.74122974434877,1.4));
#34204=CARTESIAN_POINT('Origin',(-4.32,5.29047417231657E-16,2.23154518249895));
#34205=CARTESIAN_POINT('',(-4.32,5.29047417231657E-16,2.26309036499789));
#34206=CARTESIAN_POINT('',(-4.215,5.16188625840609E-16,2.2));
#34207=CARTESIAN_POINT('',(-4.2675,5.22618021536133E-16,2.23154518249895));
#34208=CARTESIAN_POINT('Origin',(-4.32,5.29047417231657E-16,2.2));
#34209=CARTESIAN_POINT('Origin',(-4.32,5.29047417231657E-16,1.825));
#34210=CARTESIAN_POINT('',(-4.215,5.16188625840609E-16,1.45));
#34211=CARTESIAN_POINT('',(-4.215,5.16188625840609E-16,1.825));
#34212=CARTESIAN_POINT('Origin',(-4.32,5.29047417231657E-16,1.45));
#34213=CARTESIAN_POINT('Origin',(-4.32,5.29047417231657E-16,1.4));
#34214=CARTESIAN_POINT('',(-4.165,5.48029442618441E-16,1.4));
#34215=CARTESIAN_POINT('',(-4.165,5.10065391844873E-16,1.4));
#34216=CARTESIAN_POINT('Origin',(-4.32,5.29047417231657E-16,1.4));
#34217=CARTESIAN_POINT('Origin',(-2.16,3.74122974434878,2.23154518249895));
#34218=CARTESIAN_POINT('',(-2.16,3.74122974434878,2.26309036499789));
#34219=CARTESIAN_POINT('',(-2.055,3.74122974434878,2.2));
#34220=CARTESIAN_POINT('',(-2.1075,3.74122974434878,2.23154518249895));
#34221=CARTESIAN_POINT('Origin',(-2.16,3.74122974434878,2.2));
#34222=CARTESIAN_POINT('Origin',(-2.16,3.74122974434878,1.825));
#34223=CARTESIAN_POINT('',(-2.055,3.74122974434878,1.45));
#34224=CARTESIAN_POINT('',(-2.055,3.74122974434878,1.825));
#34225=CARTESIAN_POINT('Origin',(-2.16,3.74122974434878,1.45));
#34226=CARTESIAN_POINT('Origin',(-2.16,3.74122974434878,1.4));
#34227=CARTESIAN_POINT('',(-2.005,3.74122974434878,1.4));
#34228=CARTESIAN_POINT('',(-2.005,3.74122974434878,1.4));
#34229=CARTESIAN_POINT('Origin',(-2.16,3.74122974434878,1.4));
#34230=CARTESIAN_POINT('Origin',(2.16,3.74122974434878,2.23154518249895));
#34231=CARTESIAN_POINT('',(2.16,3.74122974434878,2.26309036499789));
#34232=CARTESIAN_POINT('',(2.265,3.74122974434878,2.2));
#34233=CARTESIAN_POINT('',(2.2125,3.74122974434878,2.23154518249895));
#34234=CARTESIAN_POINT('Origin',(2.16,3.74122974434878,2.2));
#34235=CARTESIAN_POINT('Origin',(2.16,3.74122974434878,1.825));
#34236=CARTESIAN_POINT('',(2.265,3.74122974434878,1.45));
#34237=CARTESIAN_POINT('',(2.265,3.74122974434878,1.825));
#34238=CARTESIAN_POINT('Origin',(2.16,3.74122974434878,1.45));
#34239=CARTESIAN_POINT('Origin',(2.16,3.74122974434878,1.4));
#34240=CARTESIAN_POINT('',(2.315,3.74122974434878,1.4));
#34241=CARTESIAN_POINT('',(2.315,3.74122974434878,1.4));
#34242=CARTESIAN_POINT('Origin',(2.16,3.74122974434878,1.4));
#34243=CARTESIAN_POINT('Origin',(4.32,0.,2.23154518249895));
#34244=CARTESIAN_POINT('',(4.32,0.,2.26309036499789));
#34245=CARTESIAN_POINT('',(4.425,-1.28587913910472E-17,2.2));
#34246=CARTESIAN_POINT('',(4.3725,-6.42939569552363E-18,2.23154518249895));
#34247=CARTESIAN_POINT('Origin',(4.32,0.,2.2));
#34248=CARTESIAN_POINT('Origin',(4.32,0.,1.825));
#34249=CARTESIAN_POINT('',(4.425,-1.28587913910472E-17,1.45));
#34250=CARTESIAN_POINT('',(4.425,-1.28587913910472E-17,1.825));
#34251=CARTESIAN_POINT('Origin',(4.32,0.,1.45));
#34252=CARTESIAN_POINT('Origin',(4.32,0.,1.4));
#34253=CARTESIAN_POINT('',(4.475,1.89820253867839E-17,1.4));
#34254=CARTESIAN_POINT('',(4.475,-1.89820253867839E-17,1.4));
#34255=CARTESIAN_POINT('Origin',(4.32,0.,1.4));
#34256=CARTESIAN_POINT('Origin',(4.17279956956878,-1.11809827484289,10.3684548175011));
#34257=CARTESIAN_POINT('',(4.17279956956878,-1.11809827484289,10.3369096350021));
#34258=CARTESIAN_POINT('',(4.06779956956878,-1.11809827484289,10.4));
#34259=CARTESIAN_POINT('',(4.12029956956878,-1.11809827484289,10.3684548175011));
#34260=CARTESIAN_POINT('Origin',(4.17279956956878,-1.11809827484289,10.4));
#34261=CARTESIAN_POINT('Origin',(4.17279956956878,-1.11809827484289,10.875));
#34262=CARTESIAN_POINT('',(4.06779956956878,-1.11809827484289,11.35));
#34263=CARTESIAN_POINT('',(4.06779956956878,-1.11809827484289,10.875));
#34264=CARTESIAN_POINT('Origin',(4.17279956956878,-1.11809827484289,11.35));
#34265=CARTESIAN_POINT('Origin',(4.17279956956878,-1.11809827484289,11.4));
#34266=CARTESIAN_POINT('',(4.01779956956878,-1.11809827484289,11.4));
#34267=CARTESIAN_POINT('',(4.01779956956878,-1.11809827484289,11.4));
#34268=CARTESIAN_POINT('Origin',(4.17279956956878,-1.11809827484289,11.4));
#34269=CARTESIAN_POINT('Origin',(3.05470129472588,-3.05470129472589,10.3684548175011));
#34270=CARTESIAN_POINT('',(3.05470129472588,-3.05470129472589,10.3369096350021));
#34271=CARTESIAN_POINT('',(2.94970129472588,-3.05470129472589,10.4));
#34272=CARTESIAN_POINT('',(3.00220129472588,-3.05470129472589,10.3684548175011));
#34273=CARTESIAN_POINT('Origin',(3.05470129472588,-3.05470129472589,10.4));
#34274=CARTESIAN_POINT('Origin',(3.05470129472588,-3.05470129472589,10.875));
#34275=CARTESIAN_POINT('',(2.94970129472588,-3.05470129472589,11.35));
#34276=CARTESIAN_POINT('',(2.94970129472588,-3.05470129472589,10.875));
#34277=CARTESIAN_POINT('Origin',(3.05470129472588,-3.05470129472589,11.35));
#34278=CARTESIAN_POINT('Origin',(3.05470129472588,-3.05470129472589,11.4));
#34279=CARTESIAN_POINT('',(2.89970129472588,-3.05470129472589,11.4));
#34280=CARTESIAN_POINT('',(2.89970129472588,-3.05470129472589,11.4));
#34281=CARTESIAN_POINT('Origin',(3.05470129472588,-3.05470129472589,11.4));
#34282=CARTESIAN_POINT('Origin',(1.11809827484289,-4.17279956956878,10.3684548175011));
#34283=CARTESIAN_POINT('',(1.11809827484289,-4.17279956956878,10.3369096350021));
#34284=CARTESIAN_POINT('',(1.01309827484289,-4.17279956956878,10.4));
#34285=CARTESIAN_POINT('',(1.06559827484289,-4.17279956956878,10.3684548175011));
#34286=CARTESIAN_POINT('Origin',(1.11809827484289,-4.17279956956878,10.4));
#34287=CARTESIAN_POINT('Origin',(1.11809827484289,-4.17279956956878,10.875));
#34288=CARTESIAN_POINT('',(1.01309827484289,-4.17279956956878,11.35));
#34289=CARTESIAN_POINT('',(1.01309827484289,-4.17279956956878,10.875));
#34290=CARTESIAN_POINT('Origin',(1.11809827484289,-4.17279956956878,11.35));
#34291=CARTESIAN_POINT('Origin',(1.11809827484289,-4.17279956956878,11.4));
#34292=CARTESIAN_POINT('',(0.963098274842888,-4.17279956956878,11.4));
#34293=CARTESIAN_POINT('',(0.963098274842888,-4.17279956956878,11.4));
#34294=CARTESIAN_POINT('Origin',(1.11809827484289,-4.17279956956878,11.4));
#34295=CARTESIAN_POINT('Origin',(-1.11809827484289,-4.17279956956878,10.3684548175011));
#34296=CARTESIAN_POINT('',(-1.11809827484289,-4.17279956956878,10.3369096350021));
#34297=CARTESIAN_POINT('',(-1.22309827484289,-4.17279956956878,10.4));
#34298=CARTESIAN_POINT('',(-1.17059827484289,-4.17279956956878,10.3684548175011));
#34299=CARTESIAN_POINT('Origin',(-1.11809827484289,-4.17279956956878,10.4));
#34300=CARTESIAN_POINT('Origin',(-1.11809827484289,-4.17279956956878,10.875));
#34301=CARTESIAN_POINT('',(-1.22309827484289,-4.17279956956878,11.35));
#34302=CARTESIAN_POINT('',(-1.22309827484289,-4.17279956956878,10.875));
#34303=CARTESIAN_POINT('Origin',(-1.11809827484289,-4.17279956956878,11.35));
#34304=CARTESIAN_POINT('Origin',(-1.11809827484289,-4.17279956956878,11.4));
#34305=CARTESIAN_POINT('',(-1.27309827484289,-4.17279956956878,11.4));
#34306=CARTESIAN_POINT('',(-1.27309827484289,-4.17279956956878,11.4));
#34307=CARTESIAN_POINT('Origin',(-1.11809827484289,-4.17279956956878,11.4));
#34308=CARTESIAN_POINT('Origin',(-3.05470129472589,-3.05470129472589,10.3684548175011));
#34309=CARTESIAN_POINT('',(-3.05470129472589,-3.05470129472589,10.3369096350021));
#34310=CARTESIAN_POINT('',(-3.15970129472589,-3.05470129472589,10.4));
#34311=CARTESIAN_POINT('',(-3.10720129472589,-3.05470129472589,10.3684548175011));
#34312=CARTESIAN_POINT('Origin',(-3.05470129472589,-3.05470129472589,10.4));
#34313=CARTESIAN_POINT('Origin',(-3.05470129472589,-3.05470129472589,10.875));
#34314=CARTESIAN_POINT('',(-3.15970129472589,-3.05470129472589,11.35));
#34315=CARTESIAN_POINT('',(-3.15970129472589,-3.05470129472589,10.875));
#34316=CARTESIAN_POINT('Origin',(-3.05470129472589,-3.05470129472589,11.35));
#34317=CARTESIAN_POINT('Origin',(-3.05470129472589,-3.05470129472589,11.4));
#34318=CARTESIAN_POINT('',(-3.20970129472589,-3.05470129472589,11.4));
#34319=CARTESIAN_POINT('',(-3.20970129472589,-3.05470129472589,11.4));
#34320=CARTESIAN_POINT('Origin',(-3.05470129472589,-3.05470129472589,11.4));
#34321=CARTESIAN_POINT('Origin',(-4.17279956956878,-1.11809827484289,10.3684548175011));
#34322=CARTESIAN_POINT('',(-4.17279956956878,-1.11809827484289,10.3369096350021));
#34323=CARTESIAN_POINT('',(-4.27779956956878,-1.11809827484289,10.4));
#34324=CARTESIAN_POINT('',(-4.22529956956878,-1.11809827484289,10.3684548175011));
#34325=CARTESIAN_POINT('Origin',(-4.17279956956878,-1.11809827484289,10.4));
#34326=CARTESIAN_POINT('Origin',(-4.17279956956878,-1.11809827484289,10.875));
#34327=CARTESIAN_POINT('',(-4.27779956956878,-1.11809827484289,11.35));
#34328=CARTESIAN_POINT('',(-4.27779956956878,-1.11809827484289,10.875));
#34329=CARTESIAN_POINT('Origin',(-4.17279956956878,-1.11809827484289,11.35));
#34330=CARTESIAN_POINT('Origin',(-4.17279956956878,-1.11809827484289,11.4));
#34331=CARTESIAN_POINT('',(-4.32779956956878,-1.11809827484289,11.4));
#34332=CARTESIAN_POINT('',(-4.32779956956878,-1.11809827484289,11.4));
#34333=CARTESIAN_POINT('Origin',(-4.17279956956878,-1.11809827484289,11.4));
#34334=CARTESIAN_POINT('Origin',(-4.17279956956877,1.11809827484289,10.3684548175011));
#34335=CARTESIAN_POINT('',(-4.17279956956877,1.11809827484289,10.3369096350021));
#34336=CARTESIAN_POINT('',(-4.27779956956877,1.11809827484289,10.4));
#34337=CARTESIAN_POINT('',(-4.22529956956877,1.11809827484289,10.3684548175011));
#34338=CARTESIAN_POINT('Origin',(-4.17279956956877,1.11809827484289,10.4));
#34339=CARTESIAN_POINT('Origin',(-4.17279956956877,1.11809827484289,10.875));
#34340=CARTESIAN_POINT('',(-4.27779956956877,1.11809827484289,11.35));
#34341=CARTESIAN_POINT('',(-4.27779956956877,1.11809827484289,10.875));
#34342=CARTESIAN_POINT('Origin',(-4.17279956956877,1.11809827484289,11.35));
#34343=CARTESIAN_POINT('Origin',(-4.17279956956877,1.11809827484289,11.4));
#34344=CARTESIAN_POINT('',(-4.32779956956877,1.11809827484289,11.4));
#34345=CARTESIAN_POINT('',(-4.32779956956877,1.11809827484289,11.4));
#34346=CARTESIAN_POINT('Origin',(-4.17279956956877,1.11809827484289,11.4));
#34347=CARTESIAN_POINT('Origin',(-3.05470129472589,3.05470129472589,10.3684548175011));
#34348=CARTESIAN_POINT('',(-3.05470129472589,3.05470129472589,10.3369096350021));
#34349=CARTESIAN_POINT('',(-3.15970129472589,3.05470129472589,10.4));
#34350=CARTESIAN_POINT('',(-3.10720129472589,3.05470129472589,10.3684548175011));
#34351=CARTESIAN_POINT('Origin',(-3.05470129472589,3.05470129472589,10.4));
#34352=CARTESIAN_POINT('Origin',(-3.05470129472589,3.05470129472589,10.875));
#34353=CARTESIAN_POINT('',(-3.15970129472589,3.05470129472589,11.35));
#34354=CARTESIAN_POINT('',(-3.15970129472589,3.05470129472589,10.875));
#34355=CARTESIAN_POINT('Origin',(-3.05470129472589,3.05470129472589,11.35));
#34356=CARTESIAN_POINT('Origin',(-3.05470129472589,3.05470129472589,11.4));
#34357=CARTESIAN_POINT('',(-3.20970129472589,3.05470129472589,11.4));
#34358=CARTESIAN_POINT('',(-3.20970129472589,3.05470129472589,11.4));
#34359=CARTESIAN_POINT('Origin',(-3.05470129472589,3.05470129472589,11.4));
#34360=CARTESIAN_POINT('Origin',(-1.11809827484289,4.17279956956878,10.3684548175011));
#34361=CARTESIAN_POINT('',(-1.11809827484289,4.17279956956878,10.3369096350021));
#34362=CARTESIAN_POINT('',(-1.22309827484289,4.17279956956878,10.4));
#34363=CARTESIAN_POINT('',(-1.17059827484289,4.17279956956878,10.3684548175011));
#34364=CARTESIAN_POINT('Origin',(-1.11809827484289,4.17279956956878,10.4));
#34365=CARTESIAN_POINT('Origin',(-1.11809827484289,4.17279956956878,10.875));
#34366=CARTESIAN_POINT('',(-1.22309827484289,4.17279956956878,11.35));
#34367=CARTESIAN_POINT('',(-1.22309827484289,4.17279956956878,10.875));
#34368=CARTESIAN_POINT('Origin',(-1.11809827484289,4.17279956956878,11.35));
#34369=CARTESIAN_POINT('Origin',(-1.11809827484289,4.17279956956878,11.4));
#34370=CARTESIAN_POINT('',(-1.27309827484289,4.17279956956878,11.4));
#34371=CARTESIAN_POINT('',(-1.27309827484289,4.17279956956878,11.4));
#34372=CARTESIAN_POINT('Origin',(-1.11809827484289,4.17279956956878,11.4));
#34373=CARTESIAN_POINT('Origin',(1.11809827484289,4.17279956956878,10.3684548175011));
#34374=CARTESIAN_POINT('',(1.11809827484289,4.17279956956878,10.3369096350021));
#34375=CARTESIAN_POINT('',(1.01309827484289,4.17279956956878,10.4));
#34376=CARTESIAN_POINT('',(1.06559827484289,4.17279956956878,10.3684548175011));
#34377=CARTESIAN_POINT('Origin',(1.11809827484289,4.17279956956878,10.4));
#34378=CARTESIAN_POINT('Origin',(1.11809827484289,4.17279956956878,10.875));
#34379=CARTESIAN_POINT('',(1.01309827484289,4.17279956956878,11.35));
#34380=CARTESIAN_POINT('',(1.01309827484289,4.17279956956878,10.875));
#34381=CARTESIAN_POINT('Origin',(1.11809827484289,4.17279956956878,11.35));
#34382=CARTESIAN_POINT('Origin',(1.11809827484289,4.17279956956878,11.4));
#34383=CARTESIAN_POINT('',(0.96309827484289,4.17279956956878,11.4));
#34384=CARTESIAN_POINT('',(0.96309827484289,4.17279956956878,11.4));
#34385=CARTESIAN_POINT('Origin',(1.11809827484289,4.17279956956878,11.4));
#34386=CARTESIAN_POINT('Origin',(3.05470129472589,3.05470129472589,10.3684548175011));
#34387=CARTESIAN_POINT('',(3.05470129472589,3.05470129472589,10.3369096350021));
#34388=CARTESIAN_POINT('',(2.94970129472589,3.05470129472589,10.4));
#34389=CARTESIAN_POINT('',(3.00220129472589,3.05470129472589,10.3684548175011));
#34390=CARTESIAN_POINT('Origin',(3.05470129472589,3.05470129472589,10.4));
#34391=CARTESIAN_POINT('Origin',(3.05470129472589,3.05470129472589,10.875));
#34392=CARTESIAN_POINT('',(2.94970129472589,3.05470129472589,11.35));
#34393=CARTESIAN_POINT('',(2.94970129472589,3.05470129472589,10.875));
#34394=CARTESIAN_POINT('Origin',(3.05470129472589,3.05470129472589,11.35));
#34395=CARTESIAN_POINT('Origin',(3.05470129472589,3.05470129472589,11.4));
#34396=CARTESIAN_POINT('',(2.89970129472589,3.05470129472589,11.4));
#34397=CARTESIAN_POINT('',(2.89970129472589,3.05470129472589,11.4));
#34398=CARTESIAN_POINT('Origin',(3.05470129472589,3.05470129472589,11.4));
#34399=CARTESIAN_POINT('Origin',(4.17279956956878,1.11809827484289,10.3684548175011));
#34400=CARTESIAN_POINT('',(4.17279956956878,1.11809827484289,10.3369096350021));
#34401=CARTESIAN_POINT('',(4.06779956956878,1.11809827484289,10.4));
#34402=CARTESIAN_POINT('',(4.12029956956878,1.11809827484289,10.3684548175011));
#34403=CARTESIAN_POINT('Origin',(4.17279956956878,1.11809827484289,10.4));
#34404=CARTESIAN_POINT('Origin',(4.17279956956878,1.11809827484289,10.875));
#34405=CARTESIAN_POINT('',(4.06779956956878,1.11809827484289,11.35));
#34406=CARTESIAN_POINT('',(4.06779956956878,1.11809827484289,10.875));
#34407=CARTESIAN_POINT('Origin',(4.17279956956878,1.11809827484289,11.35));
#34408=CARTESIAN_POINT('Origin',(4.17279956956878,1.11809827484289,11.4));
#34409=CARTESIAN_POINT('',(4.01779956956878,1.11809827484289,11.4));
#34410=CARTESIAN_POINT('',(4.01779956956878,1.11809827484289,11.4));
#34411=CARTESIAN_POINT('Origin',(4.17279956956878,1.11809827484289,11.4));
#34412=CARTESIAN_POINT('Origin',(0.,0.,1.415));
#34413=CARTESIAN_POINT('',(4.13,-5.05779128047857E-16,1.4));
#34414=CARTESIAN_POINT('Origin',(0.,0.,1.4));
#34415=CARTESIAN_POINT('',(4.1,5.02105187650415E-16,1.43));
#34416=CARTESIAN_POINT('',(4.115,-5.03942157849136E-16,1.415));
#34417=CARTESIAN_POINT('',(-4.1,-5.02105187650415E-16,1.43));
#34418=CARTESIAN_POINT('Origin',(0.,0.,1.43));
#34419=CARTESIAN_POINT('Origin',(0.,0.,1.43));
#34420=CARTESIAN_POINT('Origin',(0.,0.,6.4));
#34421=CARTESIAN_POINT('',(4.1,-5.02105187650415E-16,11.37));
#34422=CARTESIAN_POINT('',(-4.1,-5.02105187650415E-16,11.37));
#34423=CARTESIAN_POINT('Origin',(0.,0.,11.37));
#34424=CARTESIAN_POINT('Origin',(0.,0.,11.37));
#34425=CARTESIAN_POINT('',(-4.1,-5.02105187650415E-16,6.4));
#34426=CARTESIAN_POINT('Origin',(4.6,0.,1.4));
#34427=CARTESIAN_POINT('',(4.56,5.58438940411193E-16,1.4));
#34428=CARTESIAN_POINT('Origin',(0.,0.,1.4));
#34429=CARTESIAN_POINT('Origin',(0.,0.,11.385));
#34430=CARTESIAN_POINT('',(4.13,5.05779128047857E-16,11.4));
#34431=CARTESIAN_POINT('',(4.115,-5.03942157849136E-16,11.385));
#34432=CARTESIAN_POINT('Origin',(0.,0.,11.4));
#34433=CARTESIAN_POINT('Origin',(4.1,0.,11.4));
#34434=CARTESIAN_POINT('',(4.56,-5.58438940411193E-16,11.4));
#34435=CARTESIAN_POINT('Origin',(0.,0.,11.4));
#34436=CARTESIAN_POINT('Origin',(0.,0.,11.38));
#34437=CARTESIAN_POINT('',(4.6,5.63337527607782E-16,11.36));
#34438=CARTESIAN_POINT('',(4.58,5.60888234009488E-16,11.38));
#34439=CARTESIAN_POINT('',(-4.6,-5.63337527607782E-16,11.36));
#34440=CARTESIAN_POINT('Origin',(0.,0.,11.36));
#34441=CARTESIAN_POINT('Origin',(0.,0.,11.36));
#34442=CARTESIAN_POINT('Origin',(0.,0.,6.4));
#34443=CARTESIAN_POINT('',(-4.6,-5.63337527607782E-16,1.44));
#34444=CARTESIAN_POINT('',(-4.6,-5.63337527607782E-16,6.4));
#34445=CARTESIAN_POINT('',(4.6,-5.63337527607782E-16,1.44));
#34446=CARTESIAN_POINT('Origin',(0.,0.,1.44));
#34447=CARTESIAN_POINT('Origin',(0.,0.,1.44));
#34448=CARTESIAN_POINT('Origin',(0.,0.,1.42));
#34449=CARTESIAN_POINT('',(4.58,5.60888234009488E-16,1.42));
#34450=CARTESIAN_POINT('',(0.,0.,0.));
#34451=CARTESIAN_POINT('Origin',(0.,-1.28,12.0684548175011));
#34452=CARTESIAN_POINT('',(0.,-1.28,12.0369096350021));
#34453=CARTESIAN_POINT('',(-0.105,-1.28,12.1));
#34454=CARTESIAN_POINT('',(-0.0525,-1.28,12.0684548175011));
#34455=CARTESIAN_POINT('Origin',(0.,-1.28,12.1));
#34456=CARTESIAN_POINT('Origin',(0.,-1.28,12.325));
#34457=CARTESIAN_POINT('',(-0.105,-1.28,12.55));
#34458=CARTESIAN_POINT('',(-0.105,-1.28,12.325));
#34459=CARTESIAN_POINT('Origin',(0.,-1.28,12.55));
#34460=CARTESIAN_POINT('Origin',(0.,-1.28,12.6));
#34461=CARTESIAN_POINT('',(-0.155,-1.28,12.6));
#34462=CARTESIAN_POINT('',(-0.155,-1.28,12.6));
#34463=CARTESIAN_POINT('Origin',(0.,-1.28,12.6));
#34464=CARTESIAN_POINT('Origin',(0.,1.28,12.0684548175011));
#34465=CARTESIAN_POINT('',(0.,1.28,12.0369096350021));
#34466=CARTESIAN_POINT('',(-0.105,1.28,12.1));
#34467=CARTESIAN_POINT('',(-0.0525,1.28,12.0684548175011));
#34468=CARTESIAN_POINT('Origin',(0.,1.28,12.1));
#34469=CARTESIAN_POINT('Origin',(0.,1.28,12.325));
#34470=CARTESIAN_POINT('',(-0.105,1.28,12.55));
#34471=CARTESIAN_POINT('',(-0.105,1.28,12.325));
#34472=CARTESIAN_POINT('Origin',(0.,1.28,12.55));
#34473=CARTESIAN_POINT('Origin',(0.,1.28,12.6));
#34474=CARTESIAN_POINT('',(-0.155,1.28,12.6));
#34475=CARTESIAN_POINT('',(-0.155,1.28,12.6));
#34476=CARTESIAN_POINT('Origin',(0.,1.28,12.6));
#34477=CARTESIAN_POINT('Origin',(2.94448637286709,-1.7,11.8390559402368));
#34478=CARTESIAN_POINT('',(2.94448637286709,-1.7,11.8781118804736));
#34479=CARTESIAN_POINT('',(3.07448637286709,-1.7,11.8));
#34480=CARTESIAN_POINT('',(3.00948637286709,-1.7,11.8390559402368));
#34481=CARTESIAN_POINT('Origin',(2.94448637286709,-1.7,11.8));
#34482=CARTESIAN_POINT('Origin',(2.94448637286709,-1.7,11.625));
#34483=CARTESIAN_POINT('',(3.07448637286709,-1.7,11.45));
#34484=CARTESIAN_POINT('',(3.07448637286709,-1.7,11.625));
#34485=CARTESIAN_POINT('Origin',(2.94448637286709,-1.7,11.45));
#34486=CARTESIAN_POINT('Origin',(2.94448637286709,-1.7,11.4));
#34487=CARTESIAN_POINT('',(3.12448637286709,-1.7,11.4));
#34488=CARTESIAN_POINT('',(3.12448637286709,-1.7,11.4));
#34489=CARTESIAN_POINT('Origin',(2.94448637286709,-1.7,11.4));
#34490=CARTESIAN_POINT('Origin',(-2.94448637286709,-1.7,11.8390559402368));
#34491=CARTESIAN_POINT('',(-2.94448637286709,-1.7,11.8781118804736));
#34492=CARTESIAN_POINT('',(-2.81448637286709,-1.7,11.8));
#34493=CARTESIAN_POINT('',(-2.87948637286709,-1.7,11.8390559402368));
#34494=CARTESIAN_POINT('Origin',(-2.94448637286709,-1.7,11.8));
#34495=CARTESIAN_POINT('Origin',(-2.94448637286709,-1.7,11.625));
#34496=CARTESIAN_POINT('',(-2.81448637286709,-1.7,11.45));
#34497=CARTESIAN_POINT('',(-2.81448637286709,-1.7,11.625));
#34498=CARTESIAN_POINT('Origin',(-2.94448637286709,-1.7,11.45));
#34499=CARTESIAN_POINT('Origin',(-2.94448637286709,-1.7,11.4));
#34500=CARTESIAN_POINT('',(-2.76448637286709,-1.7,11.4));
#34501=CARTESIAN_POINT('',(-2.76448637286709,-1.7,11.4));
#34502=CARTESIAN_POINT('Origin',(-2.94448637286709,-1.7,11.4));
#34503=CARTESIAN_POINT('Origin',(2.0818995585505E-16,3.4,11.8390559402368));
#34504=CARTESIAN_POINT('',(2.0818995585505E-16,3.4,11.8781118804736));
#34505=CARTESIAN_POINT('',(0.13,3.4,11.8));
#34506=CARTESIAN_POINT('',(0.0650000000000002,3.4,11.8390559402368));
#34507=CARTESIAN_POINT('Origin',(2.0818995585505E-16,3.4,11.8));
#34508=CARTESIAN_POINT('Origin',(2.0818995585505E-16,3.4,11.625));
#34509=CARTESIAN_POINT('',(0.13,3.4,11.45));
#34510=CARTESIAN_POINT('',(0.13,3.4,11.625));
#34511=CARTESIAN_POINT('Origin',(2.0818995585505E-16,3.4,11.45));
#34512=CARTESIAN_POINT('Origin',(2.0818995585505E-16,3.4,11.4));
#34513=CARTESIAN_POINT('',(0.18,3.4,11.4));
#34514=CARTESIAN_POINT('',(0.18,3.4,11.4));
#34515=CARTESIAN_POINT('Origin',(2.0818995585505E-16,3.4,11.4));
#34516=CARTESIAN_POINT('Origin',(4.17279956956878,-1.11809827484289,11.3875));
#34517=CARTESIAN_POINT('',(4.04446623623544,-1.11809827484289,11.4));
#34518=CARTESIAN_POINT('Origin',(4.17279956956878,-1.11809827484289,11.4));
#34519=CARTESIAN_POINT('',(4.05279956956878,-1.11809827484289,11.425));
#34520=CARTESIAN_POINT('',(4.04029956956878,-1.11809827484289,11.3875));
#34521=CARTESIAN_POINT('Origin',(4.17279956956878,-1.11809827484289,11.425));
#34522=CARTESIAN_POINT('Origin',(4.17279956956878,-1.11809827484289,11.8));
#34523=CARTESIAN_POINT('',(4.05279956956878,-1.11809827484289,12.175));
#34524=CARTESIAN_POINT('',(4.05279956956878,-1.11809827484289,11.8));
#34525=CARTESIAN_POINT('Origin',(4.17279956956878,-1.11809827484289,12.175));
#34526=CARTESIAN_POINT('Origin',(4.17279956956878,-1.11809827484289,12.1875));
#34527=CARTESIAN_POINT('',(4.02779956956878,-1.11809827484289,12.2));
#34528=CARTESIAN_POINT('',(4.04029956956878,-1.11809827484289,12.1875));
#34529=CARTESIAN_POINT('Origin',(4.17279956956878,-1.11809827484289,12.2));
#34530=CARTESIAN_POINT('Origin',(4.38279956956878,-1.11809827484289,12.2));
#34531=CARTESIAN_POINT('',(3.96279956956878,-1.11809827484289,12.2));
#34532=CARTESIAN_POINT('Origin',(4.17279956956878,-1.11809827484289,12.2));
#34533=CARTESIAN_POINT('Origin',(4.17279956956878,-1.11809827484289,12.4));
#34534=CARTESIAN_POINT('',(3.96279956956878,-1.11809827484289,12.6));
#34535=CARTESIAN_POINT('',(3.96279956956878,-1.11809827484289,12.4));
#34536=CARTESIAN_POINT('Origin',(4.17279956956878,-1.11809827484289,12.6));
#34537=CARTESIAN_POINT('Origin',(3.05470129472588,-3.05470129472589,11.3875));
#34538=CARTESIAN_POINT('',(2.92636796139255,-3.05470129472589,11.4));
#34539=CARTESIAN_POINT('Origin',(3.05470129472588,-3.05470129472589,11.4));
#34540=CARTESIAN_POINT('',(2.93470129472589,-3.05470129472589,11.425));
#34541=CARTESIAN_POINT('',(2.92220129472588,-3.05470129472589,11.3875));
#34542=CARTESIAN_POINT('Origin',(3.05470129472588,-3.05470129472589,11.425));
#34543=CARTESIAN_POINT('Origin',(3.05470129472588,-3.05470129472589,11.8));
#34544=CARTESIAN_POINT('',(2.93470129472589,-3.05470129472589,12.175));
#34545=CARTESIAN_POINT('',(2.93470129472589,-3.05470129472589,11.8));
#34546=CARTESIAN_POINT('Origin',(3.05470129472588,-3.05470129472589,12.175));
#34547=CARTESIAN_POINT('Origin',(3.05470129472588,-3.05470129472589,12.1875));
#34548=CARTESIAN_POINT('',(2.90970129472588,-3.05470129472589,12.2));
#34549=CARTESIAN_POINT('',(2.92220129472588,-3.05470129472589,12.1875));
#34550=CARTESIAN_POINT('Origin',(3.05470129472588,-3.05470129472589,12.2));
#34551=CARTESIAN_POINT('Origin',(3.26470129472588,-3.05470129472589,12.2));
#34552=CARTESIAN_POINT('',(2.84470129472589,-3.05470129472589,12.2));
#34553=CARTESIAN_POINT('Origin',(3.05470129472588,-3.05470129472589,12.2));
#34554=CARTESIAN_POINT('Origin',(3.05470129472588,-3.05470129472589,12.4));
#34555=CARTESIAN_POINT('',(2.84470129472589,-3.05470129472589,12.6));
#34556=CARTESIAN_POINT('',(2.84470129472589,-3.05470129472589,12.4));
#34557=CARTESIAN_POINT('Origin',(3.05470129472588,-3.05470129472589,12.6));
#34558=CARTESIAN_POINT('Origin',(1.11809827484289,-4.17279956956878,11.3875));
#34559=CARTESIAN_POINT('',(0.989764941509555,-4.17279956956878,11.4));
#34560=CARTESIAN_POINT('Origin',(1.11809827484289,-4.17279956956878,11.4));
#34561=CARTESIAN_POINT('',(0.998098274842888,-4.17279956956878,11.425));
#34562=CARTESIAN_POINT('',(0.985598274842888,-4.17279956956878,11.3875));
#34563=CARTESIAN_POINT('Origin',(1.11809827484289,-4.17279956956878,11.425));
#34564=CARTESIAN_POINT('Origin',(1.11809827484289,-4.17279956956878,11.8));
#34565=CARTESIAN_POINT('',(0.998098274842888,-4.17279956956878,12.175));
#34566=CARTESIAN_POINT('',(0.998098274842888,-4.17279956956878,11.8));
#34567=CARTESIAN_POINT('Origin',(1.11809827484289,-4.17279956956878,12.175));
#34568=CARTESIAN_POINT('Origin',(1.11809827484289,-4.17279956956878,12.1875));
#34569=CARTESIAN_POINT('',(0.973098274842888,-4.17279956956878,12.2));
#34570=CARTESIAN_POINT('',(0.985598274842888,-4.17279956956878,12.1875));
#34571=CARTESIAN_POINT('Origin',(1.11809827484289,-4.17279956956878,12.2));
#34572=CARTESIAN_POINT('Origin',(1.32809827484289,-4.17279956956878,12.2));
#34573=CARTESIAN_POINT('',(0.908098274842888,-4.17279956956878,12.2));
#34574=CARTESIAN_POINT('Origin',(1.11809827484289,-4.17279956956878,12.2));
#34575=CARTESIAN_POINT('Origin',(1.11809827484289,-4.17279956956878,12.4));
#34576=CARTESIAN_POINT('',(0.908098274842888,-4.17279956956878,12.6));
#34577=CARTESIAN_POINT('',(0.908098274842888,-4.17279956956878,12.4));
#34578=CARTESIAN_POINT('Origin',(1.11809827484289,-4.17279956956878,12.6));
#34579=CARTESIAN_POINT('Origin',(-1.11809827484289,-4.17279956956878,11.3875));
#34580=CARTESIAN_POINT('',(-1.24643160817622,-4.17279956956878,11.4));
#34581=CARTESIAN_POINT('Origin',(-1.11809827484289,-4.17279956956878,11.4));
#34582=CARTESIAN_POINT('',(-1.23809827484289,-4.17279956956878,11.425));
#34583=CARTESIAN_POINT('',(-1.25059827484289,-4.17279956956878,11.3875));
#34584=CARTESIAN_POINT('Origin',(-1.11809827484289,-4.17279956956878,11.425));
#34585=CARTESIAN_POINT('Origin',(-1.11809827484289,-4.17279956956878,11.8));
#34586=CARTESIAN_POINT('',(-1.23809827484289,-4.17279956956878,12.175));
#34587=CARTESIAN_POINT('',(-1.23809827484289,-4.17279956956878,11.8));
#34588=CARTESIAN_POINT('Origin',(-1.11809827484289,-4.17279956956878,12.175));
#34589=CARTESIAN_POINT('Origin',(-1.11809827484289,-4.17279956956878,12.1875));
#34590=CARTESIAN_POINT('',(-1.26309827484289,-4.17279956956878,12.2));
#34591=CARTESIAN_POINT('',(-1.25059827484289,-4.17279956956878,12.1875));
#34592=CARTESIAN_POINT('Origin',(-1.11809827484289,-4.17279956956878,12.2));
#34593=CARTESIAN_POINT('Origin',(-0.908098274842889,-4.17279956956878,12.2));
#34594=CARTESIAN_POINT('',(-1.32809827484289,-4.17279956956878,12.2));
#34595=CARTESIAN_POINT('Origin',(-1.11809827484289,-4.17279956956878,12.2));
#34596=CARTESIAN_POINT('Origin',(-1.11809827484289,-4.17279956956878,12.4));
#34597=CARTESIAN_POINT('',(-1.32809827484289,-4.17279956956878,12.6));
#34598=CARTESIAN_POINT('',(-1.32809827484289,-4.17279956956878,12.4));
#34599=CARTESIAN_POINT('Origin',(-1.11809827484289,-4.17279956956878,12.6));
#34600=CARTESIAN_POINT('Origin',(-3.05470129472589,-3.05470129472589,11.3875));
#34601=CARTESIAN_POINT('',(-3.18303462805922,-3.05470129472589,11.4));
#34602=CARTESIAN_POINT('Origin',(-3.05470129472589,-3.05470129472589,11.4));
#34603=CARTESIAN_POINT('',(-3.17470129472589,-3.05470129472589,11.425));
#34604=CARTESIAN_POINT('',(-3.18720129472589,-3.05470129472589,11.3875));
#34605=CARTESIAN_POINT('Origin',(-3.05470129472589,-3.05470129472589,11.425));
#34606=CARTESIAN_POINT('Origin',(-3.05470129472589,-3.05470129472589,11.8));
#34607=CARTESIAN_POINT('',(-3.17470129472589,-3.05470129472589,12.175));
#34608=CARTESIAN_POINT('',(-3.17470129472589,-3.05470129472589,11.8));
#34609=CARTESIAN_POINT('Origin',(-3.05470129472589,-3.05470129472589,12.175));
#34610=CARTESIAN_POINT('Origin',(-3.05470129472589,-3.05470129472589,12.1875));
#34611=CARTESIAN_POINT('',(-3.19970129472589,-3.05470129472589,12.2));
#34612=CARTESIAN_POINT('',(-3.18720129472589,-3.05470129472589,12.1875));
#34613=CARTESIAN_POINT('Origin',(-3.05470129472589,-3.05470129472589,12.2));
#34614=CARTESIAN_POINT('Origin',(-2.84470129472589,-3.05470129472589,12.2));
#34615=CARTESIAN_POINT('',(-3.26470129472589,-3.05470129472589,12.2));
#34616=CARTESIAN_POINT('Origin',(-3.05470129472589,-3.05470129472589,12.2));
#34617=CARTESIAN_POINT('Origin',(-3.05470129472589,-3.05470129472589,12.4));
#34618=CARTESIAN_POINT('',(-3.26470129472589,-3.05470129472589,12.6));
#34619=CARTESIAN_POINT('',(-3.26470129472589,-3.05470129472589,12.4));
#34620=CARTESIAN_POINT('Origin',(-3.05470129472589,-3.05470129472589,12.6));
#34621=CARTESIAN_POINT('Origin',(-4.17279956956878,-1.11809827484289,11.3875));
#34622=CARTESIAN_POINT('',(-4.30113290290211,-1.11809827484289,11.4));
#34623=CARTESIAN_POINT('Origin',(-4.17279956956878,-1.11809827484289,11.4));
#34624=CARTESIAN_POINT('',(-4.29279956956878,-1.11809827484289,11.425));
#34625=CARTESIAN_POINT('',(-4.30529956956878,-1.11809827484289,11.3875));
#34626=CARTESIAN_POINT('Origin',(-4.17279956956878,-1.11809827484289,11.425));
#34627=CARTESIAN_POINT('Origin',(-4.17279956956878,-1.11809827484289,11.8));
#34628=CARTESIAN_POINT('',(-4.29279956956878,-1.11809827484289,12.175));
#34629=CARTESIAN_POINT('',(-4.29279956956878,-1.11809827484289,11.8));
#34630=CARTESIAN_POINT('Origin',(-4.17279956956878,-1.11809827484289,12.175));
#34631=CARTESIAN_POINT('Origin',(-4.17279956956878,-1.11809827484289,12.1875));
#34632=CARTESIAN_POINT('',(-4.31779956956878,-1.11809827484289,12.2));
#34633=CARTESIAN_POINT('',(-4.30529956956878,-1.11809827484289,12.1875));
#34634=CARTESIAN_POINT('Origin',(-4.17279956956878,-1.11809827484289,12.2));
#34635=CARTESIAN_POINT('Origin',(-3.96279956956878,-1.11809827484289,12.2));
#34636=CARTESIAN_POINT('',(-4.38279956956878,-1.11809827484289,12.2));
#34637=CARTESIAN_POINT('Origin',(-4.17279956956878,-1.11809827484289,12.2));
#34638=CARTESIAN_POINT('Origin',(-4.17279956956878,-1.11809827484289,12.4));
#34639=CARTESIAN_POINT('',(-4.38279956956878,-1.11809827484289,12.6));
#34640=CARTESIAN_POINT('',(-4.38279956956878,-1.11809827484289,12.4));
#34641=CARTESIAN_POINT('Origin',(-4.17279956956878,-1.11809827484289,12.6));
#34642=CARTESIAN_POINT('Origin',(-4.17279956956877,1.11809827484289,11.3875));
#34643=CARTESIAN_POINT('',(-4.30113290290211,1.11809827484289,11.4));
#34644=CARTESIAN_POINT('Origin',(-4.17279956956877,1.11809827484289,11.4));
#34645=CARTESIAN_POINT('',(-4.29279956956877,1.11809827484289,11.425));
#34646=CARTESIAN_POINT('',(-4.30529956956878,1.11809827484289,11.3875));
#34647=CARTESIAN_POINT('Origin',(-4.17279956956877,1.11809827484289,11.425));
#34648=CARTESIAN_POINT('Origin',(-4.17279956956877,1.11809827484289,11.8));
#34649=CARTESIAN_POINT('',(-4.29279956956877,1.11809827484289,12.175));
#34650=CARTESIAN_POINT('',(-4.29279956956877,1.11809827484289,11.8));
#34651=CARTESIAN_POINT('Origin',(-4.17279956956877,1.11809827484289,12.175));
#34652=CARTESIAN_POINT('Origin',(-4.17279956956877,1.11809827484289,12.1875));
#34653=CARTESIAN_POINT('',(-4.31779956956878,1.11809827484289,12.2));
#34654=CARTESIAN_POINT('',(-4.30529956956878,1.11809827484289,12.1875));
#34655=CARTESIAN_POINT('Origin',(-4.17279956956877,1.11809827484289,12.2));
#34656=CARTESIAN_POINT('Origin',(-3.96279956956877,1.11809827484289,12.2));
#34657=CARTESIAN_POINT('',(-4.38279956956877,1.11809827484289,12.2));
#34658=CARTESIAN_POINT('Origin',(-4.17279956956877,1.11809827484289,12.2));
#34659=CARTESIAN_POINT('Origin',(-4.17279956956877,1.11809827484289,12.4));
#34660=CARTESIAN_POINT('',(-4.38279956956877,1.11809827484289,12.6));
#34661=CARTESIAN_POINT('',(-4.38279956956877,1.11809827484289,12.4));
#34662=CARTESIAN_POINT('Origin',(-4.17279956956877,1.11809827484289,12.6));
#34663=CARTESIAN_POINT('Origin',(-3.05470129472589,3.05470129472589,11.3875));
#34664=CARTESIAN_POINT('',(-3.18303462805922,3.05470129472589,11.4));
#34665=CARTESIAN_POINT('Origin',(-3.05470129472589,3.05470129472589,11.4));
#34666=CARTESIAN_POINT('',(-3.17470129472588,3.05470129472589,11.425));
#34667=CARTESIAN_POINT('',(-3.18720129472588,3.05470129472589,11.3875));
#34668=CARTESIAN_POINT('Origin',(-3.05470129472589,3.05470129472589,11.425));
#34669=CARTESIAN_POINT('Origin',(-3.05470129472589,3.05470129472589,11.8));
#34670=CARTESIAN_POINT('',(-3.17470129472588,3.05470129472589,12.175));
#34671=CARTESIAN_POINT('',(-3.17470129472588,3.05470129472589,11.8));
#34672=CARTESIAN_POINT('Origin',(-3.05470129472589,3.05470129472589,12.175));
#34673=CARTESIAN_POINT('Origin',(-3.05470129472589,3.05470129472589,12.1875));
#34674=CARTESIAN_POINT('',(-3.19970129472588,3.05470129472589,12.2));
#34675=CARTESIAN_POINT('',(-3.18720129472588,3.05470129472589,12.1875));
#34676=CARTESIAN_POINT('Origin',(-3.05470129472589,3.05470129472589,12.2));
#34677=CARTESIAN_POINT('Origin',(-2.84470129472589,3.05470129472589,12.2));
#34678=CARTESIAN_POINT('',(-3.26470129472589,3.05470129472589,12.2));
#34679=CARTESIAN_POINT('Origin',(-3.05470129472589,3.05470129472589,12.2));
#34680=CARTESIAN_POINT('Origin',(-3.05470129472589,3.05470129472589,12.4));
#34681=CARTESIAN_POINT('',(-3.26470129472589,3.05470129472589,12.6));
#34682=CARTESIAN_POINT('',(-3.26470129472589,3.05470129472589,12.4));
#34683=CARTESIAN_POINT('Origin',(-3.05470129472589,3.05470129472589,12.6));
#34684=CARTESIAN_POINT('Origin',(-1.11809827484289,4.17279956956878,11.3875));
#34685=CARTESIAN_POINT('',(-1.24643160817622,4.17279956956878,11.4));
#34686=CARTESIAN_POINT('Origin',(-1.11809827484289,4.17279956956878,11.4));
#34687=CARTESIAN_POINT('',(-1.23809827484289,4.17279956956878,11.425));
#34688=CARTESIAN_POINT('',(-1.25059827484289,4.17279956956878,11.3875));
#34689=CARTESIAN_POINT('Origin',(-1.11809827484289,4.17279956956878,11.425));
#34690=CARTESIAN_POINT('Origin',(-1.11809827484289,4.17279956956878,11.8));
#34691=CARTESIAN_POINT('',(-1.23809827484289,4.17279956956878,12.175));
#34692=CARTESIAN_POINT('',(-1.23809827484289,4.17279956956878,11.8));
#34693=CARTESIAN_POINT('Origin',(-1.11809827484289,4.17279956956878,12.175));
#34694=CARTESIAN_POINT('Origin',(-1.11809827484289,4.17279956956878,12.1875));
#34695=CARTESIAN_POINT('',(-1.26309827484289,4.17279956956878,12.2));
#34696=CARTESIAN_POINT('',(-1.25059827484289,4.17279956956878,12.1875));
#34697=CARTESIAN_POINT('Origin',(-1.11809827484289,4.17279956956878,12.2));
#34698=CARTESIAN_POINT('Origin',(-0.90809827484289,4.17279956956878,12.2));
#34699=CARTESIAN_POINT('',(-1.32809827484289,4.17279956956878,12.2));
#34700=CARTESIAN_POINT('Origin',(-1.11809827484289,4.17279956956878,12.2));
#34701=CARTESIAN_POINT('Origin',(-1.11809827484289,4.17279956956878,12.4));
#34702=CARTESIAN_POINT('',(-1.32809827484289,4.17279956956878,12.6));
#34703=CARTESIAN_POINT('',(-1.32809827484289,4.17279956956878,12.4));
#34704=CARTESIAN_POINT('Origin',(-1.11809827484289,4.17279956956878,12.6));
#34705=CARTESIAN_POINT('Origin',(1.11809827484289,4.17279956956878,11.3875));
#34706=CARTESIAN_POINT('',(0.989764941509557,4.17279956956878,11.4));
#34707=CARTESIAN_POINT('Origin',(1.11809827484289,4.17279956956878,11.4));
#34708=CARTESIAN_POINT('',(0.99809827484289,4.17279956956878,11.425));
#34709=CARTESIAN_POINT('',(0.98559827484289,4.17279956956878,11.3875));
#34710=CARTESIAN_POINT('Origin',(1.11809827484289,4.17279956956878,11.425));
#34711=CARTESIAN_POINT('Origin',(1.11809827484289,4.17279956956878,11.8));
#34712=CARTESIAN_POINT('',(0.99809827484289,4.17279956956878,12.175));
#34713=CARTESIAN_POINT('',(0.99809827484289,4.17279956956878,11.8));
#34714=CARTESIAN_POINT('Origin',(1.11809827484289,4.17279956956878,12.175));
#34715=CARTESIAN_POINT('Origin',(1.11809827484289,4.17279956956878,12.1875));
#34716=CARTESIAN_POINT('',(0.97309827484289,4.17279956956878,12.2));
#34717=CARTESIAN_POINT('',(0.98559827484289,4.17279956956878,12.1875));
#34718=CARTESIAN_POINT('Origin',(1.11809827484289,4.17279956956878,12.2));
#34719=CARTESIAN_POINT('Origin',(1.32809827484289,4.17279956956878,12.2));
#34720=CARTESIAN_POINT('',(0.90809827484289,4.17279956956878,12.2));
#34721=CARTESIAN_POINT('Origin',(1.11809827484289,4.17279956956878,12.2));
#34722=CARTESIAN_POINT('Origin',(1.11809827484289,4.17279956956878,12.4));
#34723=CARTESIAN_POINT('',(0.90809827484289,4.17279956956878,12.6));
#34724=CARTESIAN_POINT('',(0.90809827484289,4.17279956956878,12.4));
#34725=CARTESIAN_POINT('Origin',(1.11809827484289,4.17279956956878,12.6));
#34726=CARTESIAN_POINT('Origin',(3.05470129472589,3.05470129472589,11.3875));
#34727=CARTESIAN_POINT('',(2.92636796139255,3.05470129472589,11.4));
#34728=CARTESIAN_POINT('Origin',(3.05470129472589,3.05470129472589,11.4));
#34729=CARTESIAN_POINT('',(2.93470129472589,3.05470129472589,11.425));
#34730=CARTESIAN_POINT('',(2.92220129472589,3.05470129472589,11.3875));
#34731=CARTESIAN_POINT('Origin',(3.05470129472589,3.05470129472589,11.425));
#34732=CARTESIAN_POINT('Origin',(3.05470129472589,3.05470129472589,11.8));
#34733=CARTESIAN_POINT('',(2.93470129472589,3.05470129472589,12.175));
#34734=CARTESIAN_POINT('',(2.93470129472589,3.05470129472589,11.8));
#34735=CARTESIAN_POINT('Origin',(3.05470129472589,3.05470129472589,12.175));
#34736=CARTESIAN_POINT('Origin',(3.05470129472589,3.05470129472589,12.1875));
#34737=CARTESIAN_POINT('',(2.90970129472589,3.05470129472589,12.2));
#34738=CARTESIAN_POINT('',(2.92220129472589,3.05470129472589,12.1875));
#34739=CARTESIAN_POINT('Origin',(3.05470129472589,3.05470129472589,12.2));
#34740=CARTESIAN_POINT('Origin',(3.26470129472589,3.05470129472589,12.2));
#34741=CARTESIAN_POINT('',(2.84470129472589,3.05470129472589,12.2));
#34742=CARTESIAN_POINT('Origin',(3.05470129472589,3.05470129472589,12.2));
#34743=CARTESIAN_POINT('Origin',(3.05470129472589,3.05470129472589,12.4));
#34744=CARTESIAN_POINT('',(2.84470129472589,3.05470129472589,12.6));
#34745=CARTESIAN_POINT('',(2.84470129472589,3.05470129472589,12.4));
#34746=CARTESIAN_POINT('Origin',(3.05470129472589,3.05470129472589,12.6));
#34747=CARTESIAN_POINT('Origin',(4.17279956956878,1.11809827484289,11.3875));
#34748=CARTESIAN_POINT('',(4.04446623623544,1.11809827484289,11.4));
#34749=CARTESIAN_POINT('Origin',(4.17279956956878,1.11809827484289,11.4));
#34750=CARTESIAN_POINT('',(4.05279956956878,1.11809827484289,11.425));
#34751=CARTESIAN_POINT('',(4.04029956956878,1.11809827484289,11.3875));
#34752=CARTESIAN_POINT('Origin',(4.17279956956878,1.11809827484289,11.425));
#34753=CARTESIAN_POINT('Origin',(4.17279956956878,1.11809827484289,11.8));
#34754=CARTESIAN_POINT('',(4.05279956956878,1.11809827484289,12.175));
#34755=CARTESIAN_POINT('',(4.05279956956878,1.11809827484289,11.8));
#34756=CARTESIAN_POINT('Origin',(4.17279956956878,1.11809827484289,12.175));
#34757=CARTESIAN_POINT('Origin',(4.17279956956878,1.11809827484289,12.1875));
#34758=CARTESIAN_POINT('',(4.02779956956878,1.11809827484289,12.2));
#34759=CARTESIAN_POINT('',(4.04029956956878,1.11809827484289,12.1875));
#34760=CARTESIAN_POINT('Origin',(4.17279956956878,1.11809827484289,12.2));
#34761=CARTESIAN_POINT('Origin',(4.38279956956878,1.11809827484289,12.2));
#34762=CARTESIAN_POINT('',(3.96279956956878,1.11809827484289,12.2));
#34763=CARTESIAN_POINT('Origin',(4.17279956956878,1.11809827484289,12.2));
#34764=CARTESIAN_POINT('Origin',(4.17279956956878,1.11809827484289,12.4));
#34765=CARTESIAN_POINT('',(3.96279956956878,1.11809827484289,12.6));
#34766=CARTESIAN_POINT('',(3.96279956956878,1.11809827484289,12.4));
#34767=CARTESIAN_POINT('Origin',(4.17279956956878,1.11809827484289,12.6));
#34768=CARTESIAN_POINT('Origin',(0.,0.,11.42));
#34769=CARTESIAN_POINT('',(0.74,-9.06238631369041E-17,11.4));
#34770=CARTESIAN_POINT('Origin',(0.,0.,11.4));
#34771=CARTESIAN_POINT('',(0.7,8.57252759403147E-17,11.44));
#34772=CARTESIAN_POINT('',(0.72,-8.81745695386094E-17,11.42));
#34773=CARTESIAN_POINT('',(-0.7,-8.57252759403147E-17,11.44));
#34774=CARTESIAN_POINT('Origin',(0.,0.,11.44));
#34775=CARTESIAN_POINT('Origin',(0.,0.,11.44));
#34776=CARTESIAN_POINT('Origin',(0.,0.,11.6));
#34777=CARTESIAN_POINT('',(0.7,-8.57252759403147E-17,11.76));
#34778=CARTESIAN_POINT('',(-0.7,-8.57252759403147E-17,11.76));
#34779=CARTESIAN_POINT('Origin',(0.,0.,11.76));
#34780=CARTESIAN_POINT('Origin',(0.,0.,11.76));
#34781=CARTESIAN_POINT('',(-0.7,-8.57252759403147E-17,11.6));
#34782=CARTESIAN_POINT('Origin',(3.8,0.,11.4));
#34783=CARTESIAN_POINT('',(-3.8,-4.65365783675994E-16,11.4));
#34784=CARTESIAN_POINT('Origin',(0.,0.,11.4));
#34785=CARTESIAN_POINT('Origin',(0.,0.,11.78));
#34786=CARTESIAN_POINT('',(0.74,9.06238631369041E-17,11.8));
#34787=CARTESIAN_POINT('',(0.72,-8.81745695386094E-17,11.78));
#34788=CARTESIAN_POINT('Origin',(0.,0.,11.8));
#34789=CARTESIAN_POINT('Origin',(0.7,0.,11.8));
#34790=CARTESIAN_POINT('',(-0.9025,-1.10524373623049E-16,11.8));
#34791=CARTESIAN_POINT('Origin',(0.,0.,11.8));
#34792=CARTESIAN_POINT('Origin',(0.,0.,11.415));
#34793=CARTESIAN_POINT('',(4.6,-5.63337527607782E-16,11.43));
#34794=CARTESIAN_POINT('',(-4.6,-5.63337527607782E-16,11.43));
#34795=CARTESIAN_POINT('Origin',(0.,0.,11.43));
#34796=CARTESIAN_POINT('Origin',(0.,0.,11.43));
#34797=CARTESIAN_POINT('',(4.57,5.5966358721034E-16,11.4));
#34798=CARTESIAN_POINT('',(4.585,5.61500557409061E-16,11.415));
#34799=CARTESIAN_POINT('Origin',(0.,0.,11.4));
#34800=CARTESIAN_POINT('Origin',(0.,0.,12.));
#34801=CARTESIAN_POINT('',(4.6,5.63337527607782E-16,12.57));
#34802=CARTESIAN_POINT('',(-4.6,-5.63337527607782E-16,12.57));
#34803=CARTESIAN_POINT('Origin',(0.,0.,12.57));
#34804=CARTESIAN_POINT('Origin',(0.,0.,12.57));
#34805=CARTESIAN_POINT('',(-4.6,-5.63337527607782E-16,12.));
#34806=CARTESIAN_POINT('Origin',(4.6,0.,11.4));
#34807=CARTESIAN_POINT('',(-4.095,-5.01492864250841E-16,11.4));
#34808=CARTESIAN_POINT('Origin',(0.,0.,11.4));
#34809=CARTESIAN_POINT('Origin',(0.,0.,12.585));
#34810=CARTESIAN_POINT('',(4.57,-5.5966358721034E-16,12.6));
#34811=CARTESIAN_POINT('Origin',(0.,0.,12.6));
#34812=CARTESIAN_POINT('',(4.585,5.61500557409061E-16,12.585));
#34813=CARTESIAN_POINT('Origin',(0.9025,0.,12.6));
#34814=CARTESIAN_POINT('',(-3.83444475923175,-0.338546858194397,12.6));
#34815=CARTESIAN_POINT('',(-3.20429399400242,-1.43,12.6));
#34816=CARTESIAN_POINT('',(-3.36139274484857,-1.15789698172886,12.6));
#34817=CARTESIAN_POINT('',(-3.30821704245656,-1.61,12.6));
#34818=CARTESIAN_POINT('Origin',(-3.30821704245656,-1.49,12.6));
#34819=CARTESIAN_POINT('',(-3.66167994232156,-1.61,12.6));
#34820=CARTESIAN_POINT('',(-1.09893547277415,-1.61,12.6));
#34821=CARTESIAN_POINT('',(-3.989475518093,-0.289974292889239,12.6));
#34822=CARTESIAN_POINT('Origin',(0.,0.,12.6));
#34823=CARTESIAN_POINT('Origin',(-3.93836780768588,-0.398546858194397,12.6));
#34824=CARTESIAN_POINT('',(-3.66167994232156,1.61,12.6));
#34825=CARTESIAN_POINT('',(-3.989475518093,0.289974292889239,12.6));
#34826=CARTESIAN_POINT('Origin',(0.,0.,12.6));
#34827=CARTESIAN_POINT('',(-3.30821704245656,1.61,12.6));
#34828=CARTESIAN_POINT('',(-1.92454635771531,1.61,12.6));
#34829=CARTESIAN_POINT('',(-3.20429399400242,1.43,12.6));
#34830=CARTESIAN_POINT('Origin',(-3.30821704245656,1.49,12.6));
#34831=CARTESIAN_POINT('',(-3.83444475923175,0.338546858194397,12.6));
#34832=CARTESIAN_POINT('',(-2.94858730237799,1.87289698172886,12.6));
#34833=CARTESIAN_POINT('Origin',(-3.93836780768588,0.398546858194397,12.6));
#34834=CARTESIAN_POINT('',(-3.22514087125372,-2.36610785057841,12.6));
#34835=CARTESIAN_POINT('',(-3.04840942132122,-2.06,12.6));
#34836=CARTESIAN_POINT('',(-2.4693865789506,-1.05710301827114,12.6));
#34837=CARTESIAN_POINT('',(-2.84056332441296,-2.06,12.6));
#34838=CARTESIAN_POINT('Origin',(-2.94448637286709,-2.12,12.6));
#34839=CARTESIAN_POINT('',(-2.21041255918363,-3.1514531418056,12.6));
#34840=CARTESIAN_POINT('',(-2.87064501603739,-2.00789698172886,12.6));
#34841=CARTESIAN_POINT('',(-2.24586286313301,-3.31,12.6));
#34842=CARTESIAN_POINT('Origin',(-2.31433560763776,-3.2114531418056,12.6));
#34843=CARTESIAN_POINT('Origin',(0.,0.,12.6));
#34844=CARTESIAN_POINT('',(-2.24586286313301,3.31,12.6));
#34845=CARTESIAN_POINT('',(-3.22514087125372,2.36610785057841,12.6));
#34846=CARTESIAN_POINT('Origin',(0.,0.,12.6));
#34847=CARTESIAN_POINT('',(-2.21041255918363,3.1514531418056,12.6));
#34848=CARTESIAN_POINT('Origin',(-2.31433560763776,3.2114531418056,12.6));
#34849=CARTESIAN_POINT('',(-2.84056332441296,2.06,12.6));
#34850=CARTESIAN_POINT('',(-2.45783957356681,2.72289698172886,12.6));
#34851=CARTESIAN_POINT('',(-3.04840942132122,2.06,12.6));
#34852=CARTESIAN_POINT('Origin',(-2.94448637286709,2.12,12.6));
#34853=CARTESIAN_POINT('',(-2.05658113648002,0.342103018271136,12.6));
#34854=CARTESIAN_POINT('',(-1.62403220004812,-3.49,12.6));
#34855=CARTESIAN_POINT('',(-0.363730669589464,-3.49,12.6));
#34856=CARTESIAN_POINT('',(-0.452303171281764,-3.49,12.6));
#34857=CARTESIAN_POINT('',(-0.259807621135332,-3.67,12.6));
#34858=CARTESIAN_POINT('Origin',(-0.363730669589464,-3.61,12.6));
#34859=CARTESIAN_POINT('',(-0.436539071067832,-3.97610785057841,12.6));
#34860=CARTESIAN_POINT('',(0.732020663705873,-1.95210301827114,12.6));
#34861=CARTESIAN_POINT('',(-1.74361265495999,-3.59997429288924,12.6));
#34862=CARTESIAN_POINT('Origin',(0.,0.,12.6));
#34863=CARTESIAN_POINT('Origin',(-1.62403220004812,-3.61,12.6));
#34864=CARTESIAN_POINT('',(-0.436539071067833,3.97610785057841,12.6));
#34865=CARTESIAN_POINT('',(-1.74361265495999,3.59997429288924,12.6));
#34866=CARTESIAN_POINT('Origin',(0.,0.,12.6));
#34867=CARTESIAN_POINT('',(-0.259807621135332,3.67,12.6));
#34868=CARTESIAN_POINT('',(0.319215221235291,2.66710301827114,12.6));
#34869=CARTESIAN_POINT('',(-0.363730669589465,3.49,12.6));
#34870=CARTESIAN_POINT('Origin',(-0.363730669589464,3.61,12.6));
#34871=CARTESIAN_POINT('',(-1.62403220004812,3.49,12.6));
#34872=CARTESIAN_POINT('',(0.3733077136594,3.49,12.6));
#34873=CARTESIAN_POINT('Origin',(-1.62403220004812,3.61,12.6));
#34874=CARTESIAN_POINT('',(0.436539071067833,-3.97610785057841,12.6));
#34875=CARTESIAN_POINT('',(0.259807621135332,-3.67,12.6));
#34876=CARTESIAN_POINT('',(-0.0935902212352913,-3.05789698172886,12.6));
#34877=CARTESIAN_POINT('',(0.363730669589464,-3.49,12.6));
#34878=CARTESIAN_POINT('Origin',(0.363730669589464,-3.61,12.6));
#34879=CARTESIAN_POINT('',(1.62403220004812,-3.49,12.6));
#34880=CARTESIAN_POINT('',(0.529192286340599,-3.49,12.6));
#34881=CARTESIAN_POINT('',(1.74361265495999,-3.59997429288924,12.6));
#34882=CARTESIAN_POINT('Origin',(1.62403220004812,-3.61,12.6));
#34883=CARTESIAN_POINT('Origin',(0.,0.,12.6));
#34884=CARTESIAN_POINT('',(1.74361265495999,3.59997429288924,12.6));
#34885=CARTESIAN_POINT('',(0.436539071067832,3.97610785057841,12.6));
#34886=CARTESIAN_POINT('Origin',(0.,0.,12.6));
#34887=CARTESIAN_POINT('',(1.62403220004812,3.49,12.6));
#34888=CARTESIAN_POINT('Origin',(1.62403220004812,3.61,12.6));
#34889=CARTESIAN_POINT('',(0.363730669589464,3.49,12.6));
#34890=CARTESIAN_POINT('',(1.35480317128176,3.49,12.6));
#34891=CARTESIAN_POINT('',(0.259807621135332,3.67,12.6));
#34892=CARTESIAN_POINT('Origin',(0.363730669589464,3.61,12.6));
#34893=CARTESIAN_POINT('',(-0.506395663705874,2.34289698172886,12.6));
#34894=CARTESIAN_POINT('',(2.21041255918363,-3.1514531418056,12.6));
#34895=CARTESIAN_POINT('',(2.84056332441296,-2.06,12.6));
#34896=CARTESIAN_POINT('',(2.68346457356681,-2.33210301827114,12.6));
#34897=CARTESIAN_POINT('',(3.04840942132122,-2.06,12.6));
#34898=CARTESIAN_POINT('Origin',(2.94448637286709,-2.12,12.6));
#34899=CARTESIAN_POINT('',(3.22514087125372,-2.36610785057841,12.6));
#34900=CARTESIAN_POINT('',(2.28220613648002,-0.732896981728864,12.6));
#34901=CARTESIAN_POINT('',(2.24586286313301,-3.31,12.6));
#34902=CARTESIAN_POINT('Origin',(0.,0.,12.6));
#34903=CARTESIAN_POINT('Origin',(2.31433560763776,-3.2114531418056,12.6));
#34904=CARTESIAN_POINT('',(3.22514087125372,2.36610785057841,12.6));
#34905=CARTESIAN_POINT('',(2.24586286313301,3.31,12.6));
#34906=CARTESIAN_POINT('Origin',(0.,0.,12.6));
#34907=CARTESIAN_POINT('',(3.04840942132122,2.06,12.6));
#34908=CARTESIAN_POINT('',(2.6950115789506,1.44789698172886,12.6));
#34909=CARTESIAN_POINT('',(2.84056332441296,2.06,12.6));
#34910=CARTESIAN_POINT('Origin',(2.94448637286709,2.12,12.6));
#34911=CARTESIAN_POINT('',(2.21041255918363,3.1514531418056,12.6));
#34912=CARTESIAN_POINT('',(3.09627001603739,1.61710301827114,12.6));
#34913=CARTESIAN_POINT('Origin',(2.31433560763776,3.2114531418056,12.6));
#34914=CARTESIAN_POINT('',(3.66167994232156,-1.61,12.6));
#34915=CARTESIAN_POINT('',(3.30821704245656,-1.61,12.6));
#34916=CARTESIAN_POINT('',(2.82704635771531,-1.61,12.6));
#34917=CARTESIAN_POINT('',(3.20429399400242,-1.43,12.6));
#34918=CARTESIAN_POINT('Origin',(3.30821704245656,-1.49,12.6));
#34919=CARTESIAN_POINT('',(3.83444475923175,-0.338546858194397,12.6));
#34920=CARTESIAN_POINT('',(3.17421230237799,-1.48210301827114,12.6));
#34921=CARTESIAN_POINT('',(3.989475518093,-0.289974292889239,12.6));
#34922=CARTESIAN_POINT('Origin',(3.93836780768588,-0.398546858194397,12.6));
#34923=CARTESIAN_POINT('Origin',(0.,0.,12.6));
#34924=CARTESIAN_POINT('',(3.989475518093,0.289974292889239,12.6));
#34925=CARTESIAN_POINT('',(3.66167994232156,1.61,12.6));
#34926=CARTESIAN_POINT('Origin',(0.,0.,12.6));
#34927=CARTESIAN_POINT('',(3.83444475923175,0.338546858194397,12.6));
#34928=CARTESIAN_POINT('Origin',(3.93836780768588,0.398546858194397,12.6));
#34929=CARTESIAN_POINT('',(3.20429399400242,1.43,12.6));
#34930=CARTESIAN_POINT('',(3.58701774484857,0.767103018271136,12.6));
#34931=CARTESIAN_POINT('',(3.30821704245656,1.61,12.6));
#34932=CARTESIAN_POINT('Origin',(3.30821704245656,1.49,12.6));
#34933=CARTESIAN_POINT('',(2.00143547277415,1.61,12.6));
#34934=CARTESIAN_POINT('',(3.56225116089999,0.09,12.6));
#34935=CARTESIAN_POINT('',(2.32672158483419,0.09,12.6));
#34936=CARTESIAN_POINT('',(2.33629862890413,0.09,12.6));
#34937=CARTESIAN_POINT('',(2.22279853638006,0.27,12.6));
#34938=CARTESIAN_POINT('Origin',(2.32672158483419,0.21,12.6));
#34939=CARTESIAN_POINT('',(2.84056332441296,1.34,12.6));
#34940=CARTESIAN_POINT('',(1.94734298035004,-0.207103018271136,12.6));
#34941=CARTESIAN_POINT('',(3.04840942132122,1.34,12.6));
#34942=CARTESIAN_POINT('Origin',(2.94448637286709,1.28,12.6));
#34943=CARTESIAN_POINT('',(3.66617420935412,0.27,12.6));
#34944=CARTESIAN_POINT('',(3.01832772969679,1.39210301827114,12.6));
#34945=CARTESIAN_POINT('Origin',(3.56225116089999,0.21,12.6));
#34946=CARTESIAN_POINT('',(2.58075570327763,-1.61,12.6));
#34947=CARTESIAN_POINT('',(1.34522612721183,-1.61,12.6));
#34948=CARTESIAN_POINT('',(1.84555090009295,-1.61,12.6));
#34949=CARTESIAN_POINT('',(1.2413030787577,-1.43,12.6));
#34950=CARTESIAN_POINT('Origin',(1.34522612721183,-1.49,12.6));
#34951=CARTESIAN_POINT('',(1.85906786679059,-0.36,12.6));
#34952=CARTESIAN_POINT('',(1.45659525153885,-1.05710301827114,12.6));
#34953=CARTESIAN_POINT('',(2.06691396369886,-0.36,12.6));
#34954=CARTESIAN_POINT('Origin',(1.96299091524473,-0.420000000000001,12.6));
#34955=CARTESIAN_POINT('',(2.68467875173176,-1.43,12.6));
#34956=CARTESIAN_POINT('',(1.79145840766884,0.117103018271136,12.6));
#34957=CARTESIAN_POINT('Origin',(2.58075570327763,-1.49,12.6));
#34958=CARTESIAN_POINT('',(1.59926024565526,-3.31,12.6));
#34959=CARTESIAN_POINT('',(0.363730669589464,-3.31,12.6));
#34960=CARTESIAN_POINT('',(1.35480317128176,-3.31,12.6));
#34961=CARTESIAN_POINT('',(0.259807621135332,-3.13,12.6));
#34962=CARTESIAN_POINT('Origin',(0.363730669589464,-3.19,12.6));
#34963=CARTESIAN_POINT('',(0.877572409168231,-2.06,12.6));
#34964=CARTESIAN_POINT('',(0.965847522727672,-1.90710301827114,12.6));
#34965=CARTESIAN_POINT('',(1.0854185060765,-2.06,12.6));
#34966=CARTESIAN_POINT('Origin',(0.981495457622364,-2.12,12.6));
#34967=CARTESIAN_POINT('',(1.7031832941094,-3.13,12.6));
#34968=CARTESIAN_POINT('',(0.564589085640882,-1.15789698172886,12.6));
#34969=CARTESIAN_POINT('Origin',(1.59926024565526,-3.19,12.6));
#34970=CARTESIAN_POINT('',(2.68467875173176,1.43,12.6));
#34971=CARTESIAN_POINT('',(2.06691396369886,0.36,12.6));
#34972=CARTESIAN_POINT('',(2.20426385013942,0.597896981728864,12.6));
#34973=CARTESIAN_POINT('',(1.85906786679059,0.360000000000001,12.6));
#34974=CARTESIAN_POINT('Origin',(1.96299091524473,0.420000000000001,12.6));
#34975=CARTESIAN_POINT('',(1.2413030787577,1.43,12.6));
#34976=CARTESIAN_POINT('',(1.86940069400944,0.342103018271136,12.6));
#34977=CARTESIAN_POINT('',(1.34522612721183,1.61,12.6));
#34978=CARTESIAN_POINT('Origin',(1.34522612721183,1.49,12.6));
#34979=CARTESIAN_POINT('',(2.58075570327763,1.61,12.6));
#34980=CARTESIAN_POINT('',(1.01994001515178,1.61,12.6));
#34981=CARTESIAN_POINT('Origin',(2.58075570327763,1.49,12.6));
#34982=CARTESIAN_POINT('',(-0.363730669589465,-3.31,12.6));
#34983=CARTESIAN_POINT('',(-1.59926024565526,-3.31,12.6));
#34984=CARTESIAN_POINT('',(0.3733077136594,-3.31,12.6));
#34985=CARTESIAN_POINT('',(-1.7031832941094,-3.13,12.6));
#34986=CARTESIAN_POINT('Origin',(-1.59926024565526,-3.19,12.6));
#34987=CARTESIAN_POINT('',(-1.0854185060765,-2.06,12.6));
#34988=CARTESIAN_POINT('',(-0.751769528111464,-1.48210301827114,12.6));
#34989=CARTESIAN_POINT('',(-0.877572409168231,-2.06,12.6));
#34990=CARTESIAN_POINT('Origin',(-0.981495457622364,-2.12,12.6));
#34991=CARTESIAN_POINT('',(-0.259807621135332,-3.13,12.6));
#34992=CARTESIAN_POINT('',(-1.15302796519825,-1.58289698172886,12.6));
#34993=CARTESIAN_POINT('Origin',(-0.363730669589464,-3.19,12.6));
#34994=CARTESIAN_POINT('',(1.7031832941094,3.13,12.6));
#34995=CARTESIAN_POINT('',(1.0854185060765,2.06,12.6));
#34996=CARTESIAN_POINT('',(0.977394528111464,1.87289698172886,12.6));
#34997=CARTESIAN_POINT('',(0.877572409168231,2.06,12.6));
#34998=CARTESIAN_POINT('Origin',(0.981495457622364,2.12,12.6));
#34999=CARTESIAN_POINT('',(0.259807621135332,3.13,12.6));
#35000=CARTESIAN_POINT('',(1.37865296519825,1.19210301827114,12.6));
#35001=CARTESIAN_POINT('',(0.363730669589464,3.31,12.6));
#35002=CARTESIAN_POINT('Origin',(0.363730669589464,3.19,12.6));
#35003=CARTESIAN_POINT('',(1.59926024565526,3.31,12.6));
#35004=CARTESIAN_POINT('',(0.529192286340599,3.31,12.6));
#35005=CARTESIAN_POINT('Origin',(1.59926024565526,3.19,12.6));
#35006=CARTESIAN_POINT('',(-1.34522612721183,-1.61,12.6));
#35007=CARTESIAN_POINT('',(-2.58075570327763,-1.61,12.6));
#35008=CARTESIAN_POINT('',(-0.117440015151781,-1.61,12.6));
#35009=CARTESIAN_POINT('',(-2.68467875173176,-1.43,12.6));
#35010=CARTESIAN_POINT('Origin',(-2.58075570327763,-1.49,12.6));
#35011=CARTESIAN_POINT('',(-2.06691396369886,-0.360000000000001,12.6));
#35012=CARTESIAN_POINT('',(-1.97863885013942,-0.207103018271136,12.6));
#35013=CARTESIAN_POINT('',(-1.85906786679059,-0.36,12.6));
#35014=CARTESIAN_POINT('Origin',(-1.96299091524473,-0.420000000000001,12.6));
#35015=CARTESIAN_POINT('',(-1.2413030787577,-1.43,12.6));
#35016=CARTESIAN_POINT('',(-1.64377569400944,-0.732896981728864,12.6));
#35017=CARTESIAN_POINT('Origin',(-1.34522612721183,-1.49,12.6));
#35018=CARTESIAN_POINT('',(-0.259807621135332,3.13,12.6));
#35019=CARTESIAN_POINT('',(-0.877572409168231,2.06,12.6));
#35020=CARTESIAN_POINT('',(-0.740222522727672,2.29789698172886,12.6));
#35021=CARTESIAN_POINT('',(-1.0854185060765,2.06,12.6));
#35022=CARTESIAN_POINT('Origin',(-0.981495457622364,2.12,12.6));
#35023=CARTESIAN_POINT('',(-1.7031832941094,3.13,12.6));
#35024=CARTESIAN_POINT('',(-0.338964085640882,0.767103018271136,12.6));
#35025=CARTESIAN_POINT('',(-1.59926024565526,3.31,12.6));
#35026=CARTESIAN_POINT('Origin',(-1.59926024565526,3.19,12.6));
#35027=CARTESIAN_POINT('',(-0.363730669589464,3.31,12.6));
#35028=CARTESIAN_POINT('',(-0.452303171281764,3.31,12.6));
#35029=CARTESIAN_POINT('Origin',(-0.363730669589464,3.19,12.6));
#35030=CARTESIAN_POINT('',(-1.2413030787577,1.43,12.6));
#35031=CARTESIAN_POINT('',(-1.85906786679059,0.360000000000001,12.6));
#35032=CARTESIAN_POINT('',(-1.23097025153885,1.44789698172886,12.6));
#35033=CARTESIAN_POINT('',(-2.06691396369886,0.36,12.6));
#35034=CARTESIAN_POINT('Origin',(-1.96299091524473,0.420000000000001,12.6));
#35035=CARTESIAN_POINT('',(-2.68467875173176,1.43,12.6));
#35036=CARTESIAN_POINT('',(-1.56583340766884,-0.507896981728864,12.6));
#35037=CARTESIAN_POINT('',(-2.58075570327763,1.61,12.6));
#35038=CARTESIAN_POINT('Origin',(-2.58075570327763,1.49,12.6));
#35039=CARTESIAN_POINT('',(-1.34522612721183,1.61,12.6));
#35040=CARTESIAN_POINT('',(-0.943050900092946,1.61,12.6));
#35041=CARTESIAN_POINT('Origin',(-1.34522612721183,1.49,12.6));
#35042=CARTESIAN_POINT('',(-2.22279853638006,-0.27,12.6));
#35043=CARTESIAN_POINT('',(-2.84056332441296,-1.34,12.6));
#35044=CARTESIAN_POINT('',(-1.72171798035004,0.597896981728864,12.6));
#35045=CARTESIAN_POINT('',(-3.04840942132122,-1.34,12.6));
#35046=CARTESIAN_POINT('Origin',(-2.94448637286709,-1.28,12.6));
#35047=CARTESIAN_POINT('',(-3.66617420935412,-0.27,12.6));
#35048=CARTESIAN_POINT('',(-2.79270272969679,-1.78289698172886,12.6));
#35049=CARTESIAN_POINT('',(-3.56225116089999,-0.09,12.6));
#35050=CARTESIAN_POINT('Origin',(-3.56225116089999,-0.21,12.6));
#35051=CARTESIAN_POINT('',(-2.32672158483419,-0.09,12.6));
#35052=CARTESIAN_POINT('',(-1.43379862890413,-0.09,12.6));
#35053=CARTESIAN_POINT('Origin',(-2.32672158483419,-0.21,12.6));
#35054=CARTESIAN_POINT('',(-2.32672158483419,0.09,12.6));
#35055=CARTESIAN_POINT('',(-3.56225116089999,0.09,12.6));
#35056=CARTESIAN_POINT('',(-0.608187743962963,0.09,12.6));
#35057=CARTESIAN_POINT('',(-3.66617420935412,0.27,12.6));
#35058=CARTESIAN_POINT('Origin',(-3.56225116089999,0.21,12.6));
#35059=CARTESIAN_POINT('',(-3.04840942132122,1.34,12.6));
#35060=CARTESIAN_POINT('',(-3.20550817216737,1.06789698172886,12.6));
#35061=CARTESIAN_POINT('',(-2.84056332441296,1.34,12.6));
#35062=CARTESIAN_POINT('Origin',(-2.94448637286709,1.28,12.6));
#35063=CARTESIAN_POINT('',(-2.22279853638006,0.27,12.6));
#35064=CARTESIAN_POINT('',(-2.13452342282062,0.117103018271136,12.6));
#35065=CARTESIAN_POINT('Origin',(-2.32672158483419,0.21,12.6));
#35066=CARTESIAN_POINT('',(-1.34522612721183,1.79,12.6));
#35067=CARTESIAN_POINT('',(-2.58075570327763,1.79,12.6));
#35068=CARTESIAN_POINT('',(-0.117440015151781,1.79,12.6));
#35069=CARTESIAN_POINT('',(-2.68467875173176,1.97,12.6));
#35070=CARTESIAN_POINT('Origin',(-2.58075570327763,1.91,12.6));
#35071=CARTESIAN_POINT('',(-2.06691396369886,3.04,12.6));
#35072=CARTESIAN_POINT('',(-2.71476044335619,1.91789698172886,12.6));
#35073=CARTESIAN_POINT('',(-1.85906786679059,3.04,12.6));
#35074=CARTESIAN_POINT('Origin',(-1.96299091524473,2.98,12.6));
#35075=CARTESIAN_POINT('',(-1.2413030787577,1.97,12.6));
#35076=CARTESIAN_POINT('',(-0.907654100792664,1.39210301827114,12.6));
#35077=CARTESIAN_POINT('Origin',(-1.34522612721183,1.91,12.6));
#35078=CARTESIAN_POINT('',(-1.2413030787577,-1.97,12.6));
#35079=CARTESIAN_POINT('',(-1.85906786679059,-3.04,12.6));
#35080=CARTESIAN_POINT('',(-0.494848658322081,-0.677103018271136,12.6));
#35081=CARTESIAN_POINT('',(-2.06691396369886,-3.04,12.6));
#35082=CARTESIAN_POINT('Origin',(-1.96299091524473,-2.98,12.6));
#35083=CARTESIAN_POINT('',(-2.68467875173176,-1.97,12.6));
#35084=CARTESIAN_POINT('',(-2.30195500088561,-2.63289698172886,12.6));
#35085=CARTESIAN_POINT('',(-2.58075570327763,-1.79,12.6));
#35086=CARTESIAN_POINT('Origin',(-2.58075570327763,-1.91,12.6));
#35087=CARTESIAN_POINT('',(-1.34522612721183,-1.79,12.6));
#35088=CARTESIAN_POINT('',(-0.943050900092946,-1.79,12.6));
#35089=CARTESIAN_POINT('Origin',(-1.34522612721183,-1.91,12.6));
#35090=CARTESIAN_POINT('',(0.617764788032899,1.79,12.6));
#35091=CARTESIAN_POINT('',(-0.6177647880329,1.79,12.6));
#35092=CARTESIAN_POINT('',(0.864055442470582,1.79,12.6));
#35093=CARTESIAN_POINT('',(-0.721687836487032,1.97,12.6));
#35094=CARTESIAN_POINT('Origin',(-0.6177647880329,1.91,12.6));
#35095=CARTESIAN_POINT('',(-0.103923048454133,3.04,12.6));
#35096=CARTESIAN_POINT('',(-0.997143392517056,1.49289698172886,12.6));
#35097=CARTESIAN_POINT('',(0.103923048454133,3.04,12.6));
#35098=CARTESIAN_POINT('Origin',(8.32667268468867E-17,2.98,12.6));
#35099=CARTESIAN_POINT('',(0.721687836487032,1.97,12.6));
#35100=CARTESIAN_POINT('',(0.809962950046473,1.81710301827114,12.6));
#35101=CARTESIAN_POINT('Origin',(0.617764788032899,1.91,12.6));
#35102=CARTESIAN_POINT('',(0.721687836487032,-1.97,12.6));
#35103=CARTESIAN_POINT('',(0.103923048454133,-3.04,12.6));
#35104=CARTESIAN_POINT('',(1.22276839251706,-1.10210301827114,12.6));
#35105=CARTESIAN_POINT('',(-0.103923048454133,-3.04,12.6));
#35106=CARTESIAN_POINT('Origin',(-8.32667268468867E-17,-2.98,12.6));
#35107=CARTESIAN_POINT('',(-0.721687836487032,-1.97,12.6));
#35108=CARTESIAN_POINT('',(-0.584337950046473,-2.20789698172886,12.6));
#35109=CARTESIAN_POINT('',(-0.617764788032899,-1.79,12.6));
#35110=CARTESIAN_POINT('Origin',(-0.617764788032899,-1.91,12.6));
#35111=CARTESIAN_POINT('',(0.6177647880329,-1.79,12.6));
#35112=CARTESIAN_POINT('',(0.0384445575294176,-1.79,12.6));
#35113=CARTESIAN_POINT('Origin',(0.6177647880329,-1.91,12.6));
#35114=CARTESIAN_POINT('',(2.58075570327763,1.79,12.6));
#35115=CARTESIAN_POINT('',(1.34522612721183,1.79,12.6));
#35116=CARTESIAN_POINT('',(1.84555090009295,1.79,12.6));
#35117=CARTESIAN_POINT('',(1.2413030787577,1.97,12.6));
#35118=CARTESIAN_POINT('Origin',(1.34522612721183,1.91,12.6));
#35119=CARTESIAN_POINT('',(1.85906786679059,3.04,12.6));
#35120=CARTESIAN_POINT('',(0.720473658322081,1.06789698172886,12.6));
#35121=CARTESIAN_POINT('',(2.06691396369886,3.04,12.6));
#35122=CARTESIAN_POINT('Origin',(1.96299091524473,2.98,12.6));
#35123=CARTESIAN_POINT('',(2.68467875173176,1.97,12.6));
#35124=CARTESIAN_POINT('',(2.52758000088561,2.24210301827114,12.6));
#35125=CARTESIAN_POINT('Origin',(2.58075570327763,1.91,12.6));
#35126=CARTESIAN_POINT('',(2.68467875173176,-1.97,12.6));
#35127=CARTESIAN_POINT('',(2.06691396369886,-3.04,12.6));
#35128=CARTESIAN_POINT('',(2.94038544335619,-1.52710301827114,12.6));
#35129=CARTESIAN_POINT('',(1.85906786679059,-3.04,12.6));
#35130=CARTESIAN_POINT('Origin',(1.96299091524473,-2.98,12.6));
#35131=CARTESIAN_POINT('',(1.2413030787577,-1.97,12.6));
#35132=CARTESIAN_POINT('',(1.13327910079266,-1.78289698172886,12.6));
#35133=CARTESIAN_POINT('',(1.34522612721183,-1.79,12.6));
#35134=CARTESIAN_POINT('Origin',(1.34522612721183,-1.91,12.6));
#35135=CARTESIAN_POINT('',(2.58075570327763,-1.79,12.6));
#35136=CARTESIAN_POINT('',(1.01994001515178,-1.79,12.6));
#35137=CARTESIAN_POINT('Origin',(2.58075570327763,-1.91,12.6));
#35138=CARTESIAN_POINT('',(3.66617420935412,-0.27,12.6));
#35139=CARTESIAN_POINT('',(3.04840942132122,-1.34,12.6));
#35140=CARTESIAN_POINT('',(3.43113317216737,-0.677103018271136,12.6));
#35141=CARTESIAN_POINT('',(2.84056332441296,-1.34,12.6));
#35142=CARTESIAN_POINT('Origin',(2.94448637286709,-1.28,12.6));
#35143=CARTESIAN_POINT('',(2.22279853638006,-0.27,12.6));
#35144=CARTESIAN_POINT('',(2.36014842282062,-0.507896981728864,12.6));
#35145=CARTESIAN_POINT('',(2.32672158483419,-0.09,12.6));
#35146=CARTESIAN_POINT('Origin',(2.32672158483419,-0.21,12.6));
#35147=CARTESIAN_POINT('',(3.56225116089999,-0.09,12.6));
#35148=CARTESIAN_POINT('',(1.51068774396296,-0.09,12.6));
#35149=CARTESIAN_POINT('Origin',(3.56225116089999,-0.21,12.6));
#35150=CARTESIAN_POINT('',(-0.9025,-1.10524373623049E-16,12.6));
#35151=CARTESIAN_POINT('Origin',(0.,0.,12.6));
#35152=CARTESIAN_POINT('Origin',(3.93836780768588,-0.398546858194397,12.25));
#35153=CARTESIAN_POINT('',(3.83444475923175,-0.338546858194397,11.9));
#35154=CARTESIAN_POINT('',(3.83444475923175,-0.338546858194397,12.25));
#35155=CARTESIAN_POINT('',(3.989475518093,-0.289974292889239,11.9));
#35156=CARTESIAN_POINT('Origin',(3.93836780768588,-0.398546858194397,11.9));
#35157=CARTESIAN_POINT('',(3.989475518093,-0.289974292889239,12.25));
#35158=CARTESIAN_POINT('Origin',(3.30821704245656,1.49,12.6));
#35159=CARTESIAN_POINT('',(3.30821704245656,1.61,11.9));
#35160=CARTESIAN_POINT('',(3.20429399400242,1.43,11.9));
#35161=CARTESIAN_POINT('Origin',(3.30821704245656,1.49,11.9));
#35162=CARTESIAN_POINT('',(3.30821704245656,1.61,12.6));
#35163=CARTESIAN_POINT('',(3.20429399400242,1.43,12.6));
#35164=CARTESIAN_POINT('Origin',(3.10037094554829,1.61,12.6));
#35165=CARTESIAN_POINT('',(3.66167994232156,1.61,11.9));
#35166=CARTESIAN_POINT('',(4.75159271543062,1.61,11.9));
#35167=CARTESIAN_POINT('',(3.66167994232156,1.61,12.25));
#35168=CARTESIAN_POINT('Origin',(3.93836780768588,0.398546858194397,12.25));
#35169=CARTESIAN_POINT('',(3.83444475923175,0.338546858194397,11.9));
#35170=CARTESIAN_POINT('',(3.989475518093,0.289974292889239,11.9));
#35171=CARTESIAN_POINT('Origin',(3.93836780768588,0.398546858194397,11.9));
#35172=CARTESIAN_POINT('',(3.83444475923175,0.338546858194397,12.25));
#35173=CARTESIAN_POINT('',(3.989475518093,0.289974292889239,12.25));
#35174=CARTESIAN_POINT('Origin',(3.92598183048946,0.895,11.9));
#35175=CARTESIAN_POINT('',(3.10037094554829,1.61,11.9));
#35176=CARTESIAN_POINT('Origin',(0.,0.,11.9));
#35177=CARTESIAN_POINT('Origin',(2.32672158483419,-0.21,12.6));
#35178=CARTESIAN_POINT('',(2.32672158483419,-0.09,11.9));
#35179=CARTESIAN_POINT('',(2.22279853638006,-0.27,11.9));
#35180=CARTESIAN_POINT('Origin',(2.32672158483419,-0.21,11.9));
#35181=CARTESIAN_POINT('',(2.32672158483419,-0.09,12.6));
#35182=CARTESIAN_POINT('',(2.22279853638006,-0.27,12.6));
#35183=CARTESIAN_POINT('Origin',(2.11887548792593,-0.09,12.6));
#35184=CARTESIAN_POINT('',(3.56225116089999,-0.09,11.9));
#35185=CARTESIAN_POINT('',(3.77009725780826,-0.09,11.9));
#35186=CARTESIAN_POINT('',(3.56225116089999,-0.09,12.6));
#35187=CARTESIAN_POINT('Origin',(2.94448637286709,-1.28,12.6));
#35188=CARTESIAN_POINT('',(2.84056332441296,-1.34,11.9));
#35189=CARTESIAN_POINT('',(3.04840942132122,-1.34,11.9));
#35190=CARTESIAN_POINT('Origin',(2.94448637286709,-1.28,11.9));
#35191=CARTESIAN_POINT('',(2.84056332441296,-1.34,12.6));
#35192=CARTESIAN_POINT('',(3.04840942132122,-1.34,12.6));
#35193=CARTESIAN_POINT('Origin',(2.94448637286709,-0.805,11.9));
#35194=CARTESIAN_POINT('',(2.11887548792593,-0.09,11.9));
#35195=CARTESIAN_POINT('',(3.66617420935412,-0.27,11.9));
#35196=CARTESIAN_POINT('',(2.94448637286709,-1.52,11.9));
#35197=CARTESIAN_POINT('Origin',(3.56225116089999,-0.21,11.9));
#35198=CARTESIAN_POINT('Origin',(3.77009725780826,-0.0900000000000001,12.6));
#35199=CARTESIAN_POINT('',(3.66617420935412,-0.27,12.6));
#35200=CARTESIAN_POINT('Origin',(3.56225116089999,-0.21,12.6));
#35201=CARTESIAN_POINT('Origin',(1.34522612721183,-1.91,12.6));
#35202=CARTESIAN_POINT('',(1.34522612721183,-1.79,11.9));
#35203=CARTESIAN_POINT('',(1.2413030787577,-1.97,11.9));
#35204=CARTESIAN_POINT('Origin',(1.34522612721183,-1.91,11.9));
#35205=CARTESIAN_POINT('',(1.34522612721183,-1.79,12.6));
#35206=CARTESIAN_POINT('',(1.2413030787577,-1.97,12.6));
#35207=CARTESIAN_POINT('Origin',(1.13738003030356,-1.79,12.6));
#35208=CARTESIAN_POINT('',(2.58075570327763,-1.79,11.9));
#35209=CARTESIAN_POINT('',(2.78860180018589,-1.79,11.9));
#35210=CARTESIAN_POINT('',(2.58075570327763,-1.79,12.6));
#35211=CARTESIAN_POINT('Origin',(1.96299091524473,-2.98,12.6));
#35212=CARTESIAN_POINT('',(1.85906786679059,-3.04,11.9));
#35213=CARTESIAN_POINT('',(2.06691396369886,-3.04,11.9));
#35214=CARTESIAN_POINT('Origin',(1.96299091524473,-2.98,11.9));
#35215=CARTESIAN_POINT('',(1.85906786679059,-3.04,12.6));
#35216=CARTESIAN_POINT('',(2.06691396369886,-3.04,12.6));
#35217=CARTESIAN_POINT('Origin',(1.96299091524473,-2.505,11.9));
#35218=CARTESIAN_POINT('',(1.13738003030356,-1.79,11.9));
#35219=CARTESIAN_POINT('',(2.68467875173176,-1.97,11.9));
#35220=CARTESIAN_POINT('',(1.96299091524473,-3.22,11.9));
#35221=CARTESIAN_POINT('Origin',(2.58075570327763,-1.91,11.9));
#35222=CARTESIAN_POINT('Origin',(2.78860180018589,-1.79,12.6));
#35223=CARTESIAN_POINT('',(2.68467875173176,-1.97,12.6));
#35224=CARTESIAN_POINT('Origin',(2.58075570327763,-1.91,12.6));
#35225=CARTESIAN_POINT('Origin',(1.62403220004812,-3.61,12.25));
#35226=CARTESIAN_POINT('',(1.62403220004812,-3.49,11.9));
#35227=CARTESIAN_POINT('',(1.62403220004812,-3.49,12.25));
#35228=CARTESIAN_POINT('',(1.74361265495999,-3.59997429288924,11.9));
#35229=CARTESIAN_POINT('Origin',(1.62403220004812,-3.61,11.9));
#35230=CARTESIAN_POINT('',(1.74361265495999,-3.59997429288924,12.25));
#35231=CARTESIAN_POINT('Origin',(1.96299091524473,2.98,12.6));
#35232=CARTESIAN_POINT('',(2.06691396369886,3.04,11.9));
#35233=CARTESIAN_POINT('',(1.85906786679059,3.04,11.9));
#35234=CARTESIAN_POINT('Origin',(1.96299091524473,2.98,11.9));
#35235=CARTESIAN_POINT('',(2.06691396369886,3.04,12.6));
#35236=CARTESIAN_POINT('',(1.85906786679059,3.04,12.6));
#35237=CARTESIAN_POINT('Origin',(1.96299091524473,3.22,12.6));
#35238=CARTESIAN_POINT('',(2.68467875173176,1.97,11.9));
#35239=CARTESIAN_POINT('',(2.78860180018589,1.79,11.9));
#35240=CARTESIAN_POINT('',(2.68467875173176,1.97,12.6));
#35241=CARTESIAN_POINT('Origin',(1.34522612721183,1.91,12.6));
#35242=CARTESIAN_POINT('',(1.2413030787577,1.97,11.9));
#35243=CARTESIAN_POINT('',(1.34522612721183,1.79,11.9));
#35244=CARTESIAN_POINT('Origin',(1.34522612721183,1.91,11.9));
#35245=CARTESIAN_POINT('',(1.2413030787577,1.97,12.6));
#35246=CARTESIAN_POINT('',(1.34522612721183,1.79,12.6));
#35247=CARTESIAN_POINT('Origin',(1.96299091524473,2.505,11.9));
#35248=CARTESIAN_POINT('',(1.96299091524473,3.22,11.9));
#35249=CARTESIAN_POINT('',(2.58075570327763,1.79,11.9));
#35250=CARTESIAN_POINT('',(1.13738003030356,1.79,11.9));
#35251=CARTESIAN_POINT('Origin',(2.58075570327763,1.91,11.9));
#35252=CARTESIAN_POINT('Origin',(2.78860180018589,1.79,12.6));
#35253=CARTESIAN_POINT('',(2.58075570327763,1.79,12.6));
#35254=CARTESIAN_POINT('Origin',(2.58075570327763,1.91,12.6));
#35255=CARTESIAN_POINT('Origin',(-0.617764788032899,-1.91,12.6));
#35256=CARTESIAN_POINT('',(-0.617764788032899,-1.79,11.9));
#35257=CARTESIAN_POINT('',(-0.721687836487032,-1.97,11.9));
#35258=CARTESIAN_POINT('Origin',(-0.617764788032899,-1.91,11.9));
#35259=CARTESIAN_POINT('',(-0.617764788032899,-1.79,12.6));
#35260=CARTESIAN_POINT('',(-0.721687836487032,-1.97,12.6));
#35261=CARTESIAN_POINT('Origin',(-0.825610884941165,-1.79,12.6));
#35262=CARTESIAN_POINT('',(0.6177647880329,-1.79,11.9));
#35263=CARTESIAN_POINT('',(0.825610884941165,-1.79,11.9));
#35264=CARTESIAN_POINT('',(0.6177647880329,-1.79,12.6));
#35265=CARTESIAN_POINT('Origin',(-8.32667268468867E-17,-2.98,12.6));
#35266=CARTESIAN_POINT('',(-0.103923048454133,-3.04,11.9));
#35267=CARTESIAN_POINT('',(0.103923048454133,-3.04,11.9));
#35268=CARTESIAN_POINT('Origin',(-8.32667268468867E-17,-2.98,11.9));
#35269=CARTESIAN_POINT('',(-0.103923048454133,-3.04,12.6));
#35270=CARTESIAN_POINT('',(0.103923048454133,-3.04,12.6));
#35271=CARTESIAN_POINT('Origin',(0.,-2.505,11.9));
#35272=CARTESIAN_POINT('',(-0.825610884941165,-1.79,11.9));
#35273=CARTESIAN_POINT('',(0.721687836487032,-1.97,11.9));
#35274=CARTESIAN_POINT('',(0.,-3.22,11.9));
#35275=CARTESIAN_POINT('Origin',(0.6177647880329,-1.91,11.9));
#35276=CARTESIAN_POINT('Origin',(0.825610884941165,-1.79,12.6));
#35277=CARTESIAN_POINT('',(0.721687836487032,-1.97,12.6));
#35278=CARTESIAN_POINT('Origin',(0.6177647880329,-1.91,12.6));
#35279=CARTESIAN_POINT('Origin',(-0.363730669589464,-3.61,12.6));
#35280=CARTESIAN_POINT('',(-0.259807621135332,-3.67,11.9));
#35281=CARTESIAN_POINT('',(-0.363730669589464,-3.49,11.9));
#35282=CARTESIAN_POINT('Origin',(-0.363730669589464,-3.61,11.9));
#35283=CARTESIAN_POINT('',(-0.259807621135332,-3.67,12.6));
#35284=CARTESIAN_POINT('',(-0.363730669589464,-3.49,12.6));
#35285=CARTESIAN_POINT('Origin',(-0.155884572681199,-3.49,12.6));
#35286=CARTESIAN_POINT('',(-0.436539071067832,-3.97610785057841,11.9));
#35287=CARTESIAN_POINT('',(-0.981495457622364,-4.92,11.9));
#35288=CARTESIAN_POINT('',(-0.436539071067832,-3.97610785057841,12.25));
#35289=CARTESIAN_POINT('Origin',(0.363730669589464,3.61,12.6));
#35290=CARTESIAN_POINT('',(0.259807621135332,3.67,11.9));
#35291=CARTESIAN_POINT('',(0.363730669589464,3.49,11.9));
#35292=CARTESIAN_POINT('Origin',(0.363730669589464,3.61,11.9));
#35293=CARTESIAN_POINT('',(0.259807621135332,3.67,12.6));
#35294=CARTESIAN_POINT('',(0.363730669589464,3.49,12.6));
#35295=CARTESIAN_POINT('Origin',(0.981495457622364,4.205,11.9));
#35296=CARTESIAN_POINT('',(1.62403220004812,3.49,11.9));
#35297=CARTESIAN_POINT('',(0.155884572681199,3.49,11.9));
#35298=CARTESIAN_POINT('',(1.74361265495999,3.59997429288924,11.9));
#35299=CARTESIAN_POINT('Origin',(1.62403220004812,3.61,11.9));
#35300=CARTESIAN_POINT('',(0.436539071067832,3.97610785057841,11.9));
#35301=CARTESIAN_POINT('Origin',(0.,0.,11.9));
#35302=CARTESIAN_POINT('',(0.981495457622364,4.92,11.9));
#35303=CARTESIAN_POINT('Origin',(1.80710634256353,3.49,12.6));
#35304=CARTESIAN_POINT('',(1.62403220004812,3.49,12.25));
#35305=CARTESIAN_POINT('Origin',(1.62403220004812,3.61,12.25));
#35306=CARTESIAN_POINT('',(1.74361265495999,3.59997429288924,12.25));
#35307=CARTESIAN_POINT('Origin',(8.32667268468867E-17,2.98,12.6));
#35308=CARTESIAN_POINT('',(0.103923048454133,3.04,11.9));
#35309=CARTESIAN_POINT('',(-0.103923048454133,3.04,11.9));
#35310=CARTESIAN_POINT('Origin',(8.32667268468867E-17,2.98,11.9));
#35311=CARTESIAN_POINT('',(0.103923048454133,3.04,12.6));
#35312=CARTESIAN_POINT('',(-0.103923048454133,3.04,12.6));
#35313=CARTESIAN_POINT('Origin',(0.,3.22,12.6));
#35314=CARTESIAN_POINT('',(0.721687836487032,1.97,11.9));
#35315=CARTESIAN_POINT('',(0.825610884941165,1.79,11.9));
#35316=CARTESIAN_POINT('',(0.721687836487032,1.97,12.6));
#35317=CARTESIAN_POINT('Origin',(-0.6177647880329,1.91,12.6));
#35318=CARTESIAN_POINT('',(-0.721687836487032,1.97,11.9));
#35319=CARTESIAN_POINT('',(-0.6177647880329,1.79,11.9));
#35320=CARTESIAN_POINT('Origin',(-0.6177647880329,1.91,11.9));
#35321=CARTESIAN_POINT('',(-0.721687836487032,1.97,12.6));
#35322=CARTESIAN_POINT('',(-0.6177647880329,1.79,12.6));
#35323=CARTESIAN_POINT('Origin',(0.,2.505,11.9));
#35324=CARTESIAN_POINT('',(0.,3.22,11.9));
#35325=CARTESIAN_POINT('',(0.617764788032899,1.79,11.9));
#35326=CARTESIAN_POINT('',(-0.825610884941165,1.79,11.9));
#35327=CARTESIAN_POINT('Origin',(0.617764788032899,1.91,11.9));
#35328=CARTESIAN_POINT('Origin',(0.825610884941165,1.79,12.6));
#35329=CARTESIAN_POINT('',(0.617764788032899,1.79,12.6));
#35330=CARTESIAN_POINT('Origin',(0.617764788032899,1.91,12.6));
#35331=CARTESIAN_POINT('Origin',(-2.58075570327763,-1.91,12.6));
#35332=CARTESIAN_POINT('',(-2.58075570327763,-1.79,11.9));
#35333=CARTESIAN_POINT('',(-2.68467875173176,-1.97,11.9));
#35334=CARTESIAN_POINT('Origin',(-2.58075570327763,-1.91,11.9));
#35335=CARTESIAN_POINT('',(-2.58075570327763,-1.79,12.6));
#35336=CARTESIAN_POINT('',(-2.68467875173176,-1.97,12.6));
#35337=CARTESIAN_POINT('Origin',(-2.78860180018589,-1.79,12.6));
#35338=CARTESIAN_POINT('',(-1.34522612721183,-1.79,11.9));
#35339=CARTESIAN_POINT('',(-1.13738003030356,-1.79,11.9));
#35340=CARTESIAN_POINT('',(-1.34522612721183,-1.79,12.6));
#35341=CARTESIAN_POINT('Origin',(-1.96299091524473,-2.98,12.6));
#35342=CARTESIAN_POINT('',(-2.06691396369886,-3.04,11.9));
#35343=CARTESIAN_POINT('',(-1.85906786679059,-3.04,11.9));
#35344=CARTESIAN_POINT('Origin',(-1.96299091524473,-2.98,11.9));
#35345=CARTESIAN_POINT('',(-2.06691396369886,-3.04,12.6));
#35346=CARTESIAN_POINT('',(-1.85906786679059,-3.04,12.6));
#35347=CARTESIAN_POINT('Origin',(-1.96299091524473,-2.505,11.9));
#35348=CARTESIAN_POINT('',(-2.78860180018589,-1.79,11.9));
#35349=CARTESIAN_POINT('',(-1.2413030787577,-1.97,11.9));
#35350=CARTESIAN_POINT('',(-1.96299091524473,-3.22,11.9));
#35351=CARTESIAN_POINT('Origin',(-1.34522612721183,-1.91,11.9));
#35352=CARTESIAN_POINT('Origin',(-1.13738003030356,-1.79,12.6));
#35353=CARTESIAN_POINT('',(-1.2413030787577,-1.97,12.6));
#35354=CARTESIAN_POINT('Origin',(-1.34522612721183,-1.91,12.6));
#35355=CARTESIAN_POINT('Origin',(-1.62403220004812,3.61,12.25));
#35356=CARTESIAN_POINT('',(-1.62403220004812,3.49,11.9));
#35357=CARTESIAN_POINT('',(-1.62403220004812,3.49,12.25));
#35358=CARTESIAN_POINT('',(-1.74361265495999,3.59997429288924,11.9));
#35359=CARTESIAN_POINT('Origin',(-1.62403220004812,3.61,11.9));
#35360=CARTESIAN_POINT('',(-1.74361265495999,3.59997429288924,12.25));
#35361=CARTESIAN_POINT('Origin',(-0.981495457622364,4.205,11.9));
#35362=CARTESIAN_POINT('',(-0.363730669589464,3.49,11.9));
#35363=CARTESIAN_POINT('',(-1.80710634256353,3.49,11.9));
#35364=CARTESIAN_POINT('',(-0.259807621135332,3.67,11.9));
#35365=CARTESIAN_POINT('Origin',(-0.363730669589464,3.61,11.9));
#35366=CARTESIAN_POINT('',(-0.436539071067833,3.97610785057841,11.9));
#35367=CARTESIAN_POINT('',(-0.155884572681199,3.49,11.9));
#35368=CARTESIAN_POINT('Origin',(0.,0.,11.9));
#35369=CARTESIAN_POINT('Origin',(-0.155884572681199,3.49,12.6));
#35370=CARTESIAN_POINT('',(-0.363730669589464,3.49,12.6));
#35371=CARTESIAN_POINT('Origin',(-0.363730669589464,3.61,12.6));
#35372=CARTESIAN_POINT('',(-0.259807621135332,3.67,12.6));
#35373=CARTESIAN_POINT('Origin',(-0.981495457622364,4.92,12.6));
#35374=CARTESIAN_POINT('',(-0.436539071067833,3.97610785057841,12.25));
#35375=CARTESIAN_POINT('Origin',(-1.96299091524473,2.98,12.6));
#35376=CARTESIAN_POINT('',(-1.85906786679059,3.04,11.9));
#35377=CARTESIAN_POINT('',(-2.06691396369886,3.04,11.9));
#35378=CARTESIAN_POINT('Origin',(-1.96299091524473,2.98,11.9));
#35379=CARTESIAN_POINT('',(-1.85906786679059,3.04,12.6));
#35380=CARTESIAN_POINT('',(-2.06691396369886,3.04,12.6));
#35381=CARTESIAN_POINT('Origin',(-1.96299091524473,3.22,12.6));
#35382=CARTESIAN_POINT('',(-1.2413030787577,1.97,11.9));
#35383=CARTESIAN_POINT('',(-1.13738003030356,1.79,11.9));
#35384=CARTESIAN_POINT('',(-1.2413030787577,1.97,12.6));
#35385=CARTESIAN_POINT('Origin',(-2.58075570327763,1.91,12.6));
#35386=CARTESIAN_POINT('',(-2.68467875173176,1.97,11.9));
#35387=CARTESIAN_POINT('',(-2.58075570327763,1.79,11.9));
#35388=CARTESIAN_POINT('Origin',(-2.58075570327763,1.91,11.9));
#35389=CARTESIAN_POINT('',(-2.68467875173176,1.97,12.6));
#35390=CARTESIAN_POINT('',(-2.58075570327763,1.79,12.6));
#35391=CARTESIAN_POINT('Origin',(-1.96299091524473,2.505,11.9));
#35392=CARTESIAN_POINT('',(-1.96299091524473,3.22,11.9));
#35393=CARTESIAN_POINT('',(-1.34522612721183,1.79,11.9));
#35394=CARTESIAN_POINT('',(-2.78860180018589,1.79,11.9));
#35395=CARTESIAN_POINT('Origin',(-1.34522612721183,1.91,11.9));
#35396=CARTESIAN_POINT('Origin',(-1.13738003030356,1.79,12.6));
#35397=CARTESIAN_POINT('',(-1.34522612721183,1.79,12.6));
#35398=CARTESIAN_POINT('Origin',(-1.34522612721183,1.91,12.6));
#35399=CARTESIAN_POINT('Origin',(-2.94448637286709,1.28,12.6));
#35400=CARTESIAN_POINT('',(-2.84056332441296,1.34,11.9));
#35401=CARTESIAN_POINT('',(-3.04840942132122,1.34,11.9));
#35402=CARTESIAN_POINT('Origin',(-2.94448637286709,1.28,11.9));
#35403=CARTESIAN_POINT('',(-2.84056332441296,1.34,12.6));
#35404=CARTESIAN_POINT('',(-3.04840942132122,1.34,12.6));
#35405=CARTESIAN_POINT('Origin',(-2.94448637286709,1.52,12.6));
#35406=CARTESIAN_POINT('',(-2.22279853638006,0.27,11.9));
#35407=CARTESIAN_POINT('',(-2.11887548792593,0.09,11.9));
#35408=CARTESIAN_POINT('',(-2.22279853638006,0.27,12.6));
#35409=CARTESIAN_POINT('Origin',(-3.56225116089999,0.21,12.6));
#35410=CARTESIAN_POINT('',(-3.66617420935412,0.27,11.9));
#35411=CARTESIAN_POINT('',(-3.56225116089999,0.09,11.9));
#35412=CARTESIAN_POINT('Origin',(-3.56225116089999,0.21,11.9));
#35413=CARTESIAN_POINT('',(-3.66617420935412,0.27,12.6));
#35414=CARTESIAN_POINT('',(-3.56225116089999,0.09,12.6));
#35415=CARTESIAN_POINT('Origin',(-2.94448637286709,0.805,11.9));
#35416=CARTESIAN_POINT('',(-2.94448637286709,1.52,11.9));
#35417=CARTESIAN_POINT('',(-2.32672158483419,0.09,11.9));
#35418=CARTESIAN_POINT('',(-3.77009725780826,0.09,11.9));
#35419=CARTESIAN_POINT('Origin',(-2.32672158483419,0.21,11.9));
#35420=CARTESIAN_POINT('Origin',(-2.11887548792593,0.09,12.6));
#35421=CARTESIAN_POINT('',(-2.32672158483419,0.09,12.6));
#35422=CARTESIAN_POINT('Origin',(-2.32672158483419,0.21,12.6));
#35423=CARTESIAN_POINT('Origin',(-3.30821704245656,-1.49,12.6));
#35424=CARTESIAN_POINT('',(-3.30821704245656,-1.61,11.9));
#35425=CARTESIAN_POINT('',(-3.20429399400242,-1.43,11.9));
#35426=CARTESIAN_POINT('Origin',(-3.30821704245656,-1.49,11.9));
#35427=CARTESIAN_POINT('',(-3.30821704245656,-1.61,12.6));
#35428=CARTESIAN_POINT('',(-3.20429399400242,-1.43,12.6));
#35429=CARTESIAN_POINT('Origin',(-3.10037094554829,-1.61,12.6));
#35430=CARTESIAN_POINT('',(-3.66167994232156,-1.61,11.9));
#35431=CARTESIAN_POINT('',(-4.75159271543062,-1.61,11.9));
#35432=CARTESIAN_POINT('',(-3.66167994232156,-1.61,12.25));
#35433=CARTESIAN_POINT('Origin',(-2.94448637286709,2.12,12.6));
#35434=CARTESIAN_POINT('',(-3.04840942132122,2.06,11.9));
#35435=CARTESIAN_POINT('',(-2.84056332441296,2.06,11.9));
#35436=CARTESIAN_POINT('Origin',(-2.94448637286709,2.12,11.9));
#35437=CARTESIAN_POINT('',(-3.04840942132122,2.06,12.6));
#35438=CARTESIAN_POINT('',(-2.84056332441296,2.06,12.6));
#35439=CARTESIAN_POINT('Origin',(-2.94448637286709,2.595,11.9));
#35440=CARTESIAN_POINT('',(-2.21041255918363,3.1514531418056,11.9));
#35441=CARTESIAN_POINT('',(-2.94448637286709,1.88,11.9));
#35442=CARTESIAN_POINT('',(-2.24586286313301,3.31,11.9));
#35443=CARTESIAN_POINT('Origin',(-2.31433560763776,3.2114531418056,11.9));
#35444=CARTESIAN_POINT('',(-3.22514087125372,2.36610785057841,11.9));
#35445=CARTESIAN_POINT('Origin',(0.,0.,11.9));
#35446=CARTESIAN_POINT('',(-3.77009725780826,3.31,11.9));
#35447=CARTESIAN_POINT('Origin',(-2.11887548792593,3.31,12.6));
#35448=CARTESIAN_POINT('',(-2.21041255918363,3.1514531418056,12.25));
#35449=CARTESIAN_POINT('Origin',(-2.31433560763776,3.2114531418056,12.25));
#35450=CARTESIAN_POINT('',(-2.24586286313301,3.31,12.25));
#35451=CARTESIAN_POINT('Origin',(-3.56225116089999,-0.21,12.6));
#35452=CARTESIAN_POINT('',(-3.56225116089999,-0.09,11.9));
#35453=CARTESIAN_POINT('',(-3.66617420935412,-0.27,11.9));
#35454=CARTESIAN_POINT('Origin',(-3.56225116089999,-0.21,11.9));
#35455=CARTESIAN_POINT('',(-3.56225116089999,-0.09,12.6));
#35456=CARTESIAN_POINT('',(-3.66617420935412,-0.27,12.6));
#35457=CARTESIAN_POINT('Origin',(-3.77009725780826,-0.09,12.6));
#35458=CARTESIAN_POINT('',(-2.32672158483419,-0.09,11.9));
#35459=CARTESIAN_POINT('',(-2.11887548792593,-0.09,11.9));
#35460=CARTESIAN_POINT('',(-2.32672158483419,-0.09,12.6));
#35461=CARTESIAN_POINT('Origin',(-2.94448637286709,-1.28,12.6));
#35462=CARTESIAN_POINT('',(-3.04840942132122,-1.34,11.9));
#35463=CARTESIAN_POINT('',(-2.84056332441296,-1.34,11.9));
#35464=CARTESIAN_POINT('Origin',(-2.94448637286709,-1.28,11.9));
#35465=CARTESIAN_POINT('',(-3.04840942132122,-1.34,12.6));
#35466=CARTESIAN_POINT('',(-2.84056332441296,-1.34,12.6));
#35467=CARTESIAN_POINT('Origin',(-2.94448637286709,-0.805,11.9));
#35468=CARTESIAN_POINT('',(-3.77009725780826,-0.09,11.9));
#35469=CARTESIAN_POINT('',(-2.22279853638006,-0.27,11.9));
#35470=CARTESIAN_POINT('',(-2.94448637286709,-1.52,11.9));
#35471=CARTESIAN_POINT('Origin',(-2.32672158483419,-0.21,11.9));
#35472=CARTESIAN_POINT('Origin',(-2.11887548792593,-0.0900000000000001,
12.6));
#35473=CARTESIAN_POINT('',(-2.22279853638006,-0.27,12.6));
#35474=CARTESIAN_POINT('Origin',(-2.32672158483419,-0.21,12.6));
#35475=CARTESIAN_POINT('Origin',(-2.58075570327763,1.49,12.6));
#35476=CARTESIAN_POINT('',(-2.58075570327763,1.61,11.9));
#35477=CARTESIAN_POINT('',(-2.68467875173176,1.43,11.9));
#35478=CARTESIAN_POINT('Origin',(-2.58075570327763,1.49,11.9));
#35479=CARTESIAN_POINT('',(-2.58075570327763,1.61,12.6));
#35480=CARTESIAN_POINT('',(-2.68467875173176,1.43,12.6));
#35481=CARTESIAN_POINT('Origin',(-2.78860180018589,1.61,12.6));
#35482=CARTESIAN_POINT('',(-1.34522612721183,1.61,11.9));
#35483=CARTESIAN_POINT('',(-1.13738003030356,1.61,11.9));
#35484=CARTESIAN_POINT('',(-1.34522612721183,1.61,12.6));
#35485=CARTESIAN_POINT('Origin',(-1.96299091524473,0.420000000000001,12.6));
#35486=CARTESIAN_POINT('',(-2.06691396369886,0.360000000000001,11.9));
#35487=CARTESIAN_POINT('',(-1.85906786679059,0.360000000000001,11.9));
#35488=CARTESIAN_POINT('Origin',(-1.96299091524473,0.420000000000001,11.9));
#35489=CARTESIAN_POINT('',(-2.06691396369886,0.36,12.6));
#35490=CARTESIAN_POINT('',(-1.85906786679059,0.360000000000001,12.6));
#35491=CARTESIAN_POINT('Origin',(-1.96299091524473,0.895,11.9));
#35492=CARTESIAN_POINT('',(-2.78860180018589,1.61,11.9));
#35493=CARTESIAN_POINT('',(-1.2413030787577,1.43,11.9));
#35494=CARTESIAN_POINT('',(-1.96299091524473,0.18,11.9));
#35495=CARTESIAN_POINT('Origin',(-1.34522612721183,1.49,11.9));
#35496=CARTESIAN_POINT('Origin',(-1.13738003030356,1.61,12.6));
#35497=CARTESIAN_POINT('',(-1.2413030787577,1.43,12.6));
#35498=CARTESIAN_POINT('Origin',(-1.34522612721183,1.49,12.6));
#35499=CARTESIAN_POINT('Origin',(-1.59926024565526,3.19,12.6));
#35500=CARTESIAN_POINT('',(-1.59926024565526,3.31,11.9));
#35501=CARTESIAN_POINT('',(-1.7031832941094,3.13,11.9));
#35502=CARTESIAN_POINT('Origin',(-1.59926024565526,3.19,11.9));
#35503=CARTESIAN_POINT('',(-1.59926024565526,3.31,12.6));
#35504=CARTESIAN_POINT('',(-1.7031832941094,3.13,12.6));
#35505=CARTESIAN_POINT('Origin',(-1.80710634256353,3.31,12.6));
#35506=CARTESIAN_POINT('',(-0.363730669589464,3.31,11.9));
#35507=CARTESIAN_POINT('',(-0.155884572681199,3.31,11.9));
#35508=CARTESIAN_POINT('',(-0.363730669589464,3.31,12.6));
#35509=CARTESIAN_POINT('Origin',(-0.981495457622364,2.12,12.6));
#35510=CARTESIAN_POINT('',(-1.0854185060765,2.06,11.9));
#35511=CARTESIAN_POINT('',(-0.877572409168231,2.06,11.9));
#35512=CARTESIAN_POINT('Origin',(-0.981495457622364,2.12,11.9));
#35513=CARTESIAN_POINT('',(-1.0854185060765,2.06,12.6));
#35514=CARTESIAN_POINT('',(-0.877572409168231,2.06,12.6));
#35515=CARTESIAN_POINT('Origin',(-0.981495457622364,2.595,11.9));
#35516=CARTESIAN_POINT('',(-1.80710634256353,3.31,11.9));
#35517=CARTESIAN_POINT('',(-0.259807621135332,3.13,11.9));
#35518=CARTESIAN_POINT('',(-0.981495457622364,1.88,11.9));
#35519=CARTESIAN_POINT('Origin',(-0.363730669589464,3.19,11.9));
#35520=CARTESIAN_POINT('Origin',(-0.155884572681199,3.31,12.6));
#35521=CARTESIAN_POINT('',(-0.259807621135332,3.13,12.6));
#35522=CARTESIAN_POINT('Origin',(-0.363730669589464,3.19,12.6));
#35523=CARTESIAN_POINT('Origin',(-2.31433560763776,-3.2114531418056,12.25));
#35524=CARTESIAN_POINT('',(-2.21041255918363,-3.1514531418056,11.9));
#35525=CARTESIAN_POINT('',(-2.21041255918363,-3.1514531418056,12.25));
#35526=CARTESIAN_POINT('',(-2.24586286313301,-3.31,11.9));
#35527=CARTESIAN_POINT('Origin',(-2.31433560763776,-3.2114531418056,11.9));
#35528=CARTESIAN_POINT('',(-2.24586286313301,-3.31,12.25));
#35529=CARTESIAN_POINT('Origin',(-1.96299091524473,-0.420000000000001,12.6));
#35530=CARTESIAN_POINT('',(-1.85906786679059,-0.360000000000001,11.9));
#35531=CARTESIAN_POINT('',(-2.06691396369886,-0.360000000000001,11.9));
#35532=CARTESIAN_POINT('Origin',(-1.96299091524473,-0.420000000000001,11.9));
#35533=CARTESIAN_POINT('',(-1.85906786679059,-0.360000000000001,12.6));
#35534=CARTESIAN_POINT('',(-2.06691396369886,-0.360000000000001,12.6));
#35535=CARTESIAN_POINT('Origin',(-1.96299091524473,-0.18,12.6));
#35536=CARTESIAN_POINT('',(-1.2413030787577,-1.43,11.9));
#35537=CARTESIAN_POINT('',(-1.13738003030356,-1.61,11.9));
#35538=CARTESIAN_POINT('',(-1.2413030787577,-1.43,12.6));
#35539=CARTESIAN_POINT('Origin',(-2.58075570327763,-1.49,12.6));
#35540=CARTESIAN_POINT('',(-2.68467875173176,-1.43,11.9));
#35541=CARTESIAN_POINT('',(-2.58075570327763,-1.61,11.9));
#35542=CARTESIAN_POINT('Origin',(-2.58075570327763,-1.49,11.9));
#35543=CARTESIAN_POINT('',(-2.68467875173176,-1.43,12.6));
#35544=CARTESIAN_POINT('',(-2.58075570327763,-1.61,12.6));
#35545=CARTESIAN_POINT('Origin',(-1.96299091524473,-0.895,11.9));
#35546=CARTESIAN_POINT('',(-1.96299091524473,-0.18,11.9));
#35547=CARTESIAN_POINT('',(-1.34522612721183,-1.61,11.9));
#35548=CARTESIAN_POINT('',(-2.78860180018589,-1.61,11.9));
#35549=CARTESIAN_POINT('Origin',(-1.34522612721183,-1.49,11.9));
#35550=CARTESIAN_POINT('Origin',(-1.13738003030356,-1.61,12.6));
#35551=CARTESIAN_POINT('',(-1.34522612721183,-1.61,12.6));
#35552=CARTESIAN_POINT('Origin',(-1.34522612721183,-1.49,12.6));
#35553=CARTESIAN_POINT('Origin',(0.363730669589464,3.19,12.6));
#35554=CARTESIAN_POINT('',(0.363730669589464,3.31,11.9));
#35555=CARTESIAN_POINT('',(0.259807621135332,3.13,11.9));
#35556=CARTESIAN_POINT('Origin',(0.363730669589464,3.19,11.9));
#35557=CARTESIAN_POINT('',(0.363730669589464,3.31,12.6));
#35558=CARTESIAN_POINT('',(0.259807621135332,3.13,12.6));
#35559=CARTESIAN_POINT('Origin',(0.155884572681199,3.31,12.6));
#35560=CARTESIAN_POINT('',(1.59926024565526,3.31,11.9));
#35561=CARTESIAN_POINT('',(1.80710634256353,3.31,11.9));
#35562=CARTESIAN_POINT('',(1.59926024565526,3.31,12.6));
#35563=CARTESIAN_POINT('Origin',(0.981495457622364,2.12,12.6));
#35564=CARTESIAN_POINT('',(0.877572409168231,2.06,11.9));
#35565=CARTESIAN_POINT('',(1.0854185060765,2.06,11.9));
#35566=CARTESIAN_POINT('Origin',(0.981495457622364,2.12,11.9));
#35567=CARTESIAN_POINT('',(0.877572409168231,2.06,12.6));
#35568=CARTESIAN_POINT('',(1.0854185060765,2.06,12.6));
#35569=CARTESIAN_POINT('Origin',(0.981495457622364,2.595,11.9));
#35570=CARTESIAN_POINT('',(0.155884572681199,3.31,11.9));
#35571=CARTESIAN_POINT('',(1.7031832941094,3.13,11.9));
#35572=CARTESIAN_POINT('',(0.981495457622364,1.88,11.9));
#35573=CARTESIAN_POINT('Origin',(1.59926024565526,3.19,11.9));
#35574=CARTESIAN_POINT('Origin',(1.80710634256353,3.31,12.6));
#35575=CARTESIAN_POINT('',(1.7031832941094,3.13,12.6));
#35576=CARTESIAN_POINT('Origin',(1.59926024565526,3.19,12.6));
#35577=CARTESIAN_POINT('Origin',(-3.93836780768588,0.398546858194397,12.25));
#35578=CARTESIAN_POINT('',(-3.83444475923175,0.338546858194397,11.9));
#35579=CARTESIAN_POINT('',(-3.83444475923175,0.338546858194397,12.25));
#35580=CARTESIAN_POINT('',(-3.989475518093,0.289974292889239,11.9));
#35581=CARTESIAN_POINT('Origin',(-3.93836780768588,0.398546858194397,11.9));
#35582=CARTESIAN_POINT('',(-3.989475518093,0.289974292889239,12.25));
#35583=CARTESIAN_POINT('Origin',(-3.92598183048946,0.895,11.9));
#35584=CARTESIAN_POINT('',(-3.20429399400242,1.43,11.9));
#35585=CARTESIAN_POINT('',(-3.92598183048946,0.18,11.9));
#35586=CARTESIAN_POINT('',(-3.30821704245656,1.61,11.9));
#35587=CARTESIAN_POINT('Origin',(-3.30821704245656,1.49,11.9));
#35588=CARTESIAN_POINT('',(-3.66167994232156,1.61,11.9));
#35589=CARTESIAN_POINT('',(-3.10037094554829,1.61,11.9));
#35590=CARTESIAN_POINT('Origin',(0.,0.,11.9));
#35591=CARTESIAN_POINT('Origin',(-3.10037094554829,1.61,12.6));
#35592=CARTESIAN_POINT('',(-3.20429399400242,1.43,12.6));
#35593=CARTESIAN_POINT('Origin',(-3.30821704245656,1.49,12.6));
#35594=CARTESIAN_POINT('',(-3.30821704245656,1.61,12.6));
#35595=CARTESIAN_POINT('Origin',(-4.75159271543062,1.61,12.6));
#35596=CARTESIAN_POINT('',(-3.66167994232156,1.61,12.25));
#35597=CARTESIAN_POINT('Origin',(-0.981495457622364,-2.12,12.6));
#35598=CARTESIAN_POINT('',(-0.877572409168231,-2.06,11.9));
#35599=CARTESIAN_POINT('',(-1.0854185060765,-2.06,11.9));
#35600=CARTESIAN_POINT('Origin',(-0.981495457622364,-2.12,11.9));
#35601=CARTESIAN_POINT('',(-0.877572409168231,-2.06,12.6));
#35602=CARTESIAN_POINT('',(-1.0854185060765,-2.06,12.6));
#35603=CARTESIAN_POINT('Origin',(-0.981495457622364,-1.88,12.6));
#35604=CARTESIAN_POINT('',(-0.259807621135332,-3.13,11.9));
#35605=CARTESIAN_POINT('',(-0.155884572681199,-3.31,11.9));
#35606=CARTESIAN_POINT('',(-0.259807621135332,-3.13,12.6));
#35607=CARTESIAN_POINT('Origin',(-1.59926024565526,-3.19,12.6));
#35608=CARTESIAN_POINT('',(-1.7031832941094,-3.13,11.9));
#35609=CARTESIAN_POINT('',(-1.59926024565526,-3.31,11.9));
#35610=CARTESIAN_POINT('Origin',(-1.59926024565526,-3.19,11.9));
#35611=CARTESIAN_POINT('',(-1.7031832941094,-3.13,12.6));
#35612=CARTESIAN_POINT('',(-1.59926024565526,-3.31,12.6));
#35613=CARTESIAN_POINT('Origin',(-0.981495457622364,-2.595,11.9));
#35614=CARTESIAN_POINT('',(-0.981495457622364,-1.88,11.9));
#35615=CARTESIAN_POINT('',(-0.363730669589464,-3.31,11.9));
#35616=CARTESIAN_POINT('',(-1.80710634256353,-3.31,11.9));
#35617=CARTESIAN_POINT('Origin',(-0.363730669589464,-3.19,11.9));
#35618=CARTESIAN_POINT('Origin',(-0.155884572681199,-3.31,12.6));
#35619=CARTESIAN_POINT('',(-0.363730669589464,-3.31,12.6));
#35620=CARTESIAN_POINT('Origin',(-0.363730669589464,-3.19,12.6));
#35621=CARTESIAN_POINT('Origin',(1.34522612721183,1.49,12.6));
#35622=CARTESIAN_POINT('',(1.34522612721183,1.61,11.9));
#35623=CARTESIAN_POINT('',(1.2413030787577,1.43,11.9));
#35624=CARTESIAN_POINT('Origin',(1.34522612721183,1.49,11.9));
#35625=CARTESIAN_POINT('',(1.34522612721183,1.61,12.6));
#35626=CARTESIAN_POINT('',(1.2413030787577,1.43,12.6));
#35627=CARTESIAN_POINT('Origin',(1.13738003030356,1.61,12.6));
#35628=CARTESIAN_POINT('',(2.58075570327763,1.61,11.9));
#35629=CARTESIAN_POINT('',(2.78860180018589,1.61,11.9));
#35630=CARTESIAN_POINT('',(2.58075570327763,1.61,12.6));
#35631=CARTESIAN_POINT('Origin',(1.96299091524473,0.420000000000001,12.6));
#35632=CARTESIAN_POINT('',(1.85906786679059,0.360000000000001,11.9));
#35633=CARTESIAN_POINT('',(2.06691396369886,0.360000000000001,11.9));
#35634=CARTESIAN_POINT('Origin',(1.96299091524473,0.420000000000001,11.9));
#35635=CARTESIAN_POINT('',(1.85906786679059,0.360000000000001,12.6));
#35636=CARTESIAN_POINT('',(2.06691396369886,0.360000000000001,12.6));
#35637=CARTESIAN_POINT('Origin',(1.96299091524473,0.895,11.9));
#35638=CARTESIAN_POINT('',(1.13738003030356,1.61,11.9));
#35639=CARTESIAN_POINT('',(2.68467875173176,1.43,11.9));
#35640=CARTESIAN_POINT('',(1.96299091524473,0.18,11.9));
#35641=CARTESIAN_POINT('Origin',(2.58075570327763,1.49,11.9));
#35642=CARTESIAN_POINT('Origin',(2.78860180018589,1.61,12.6));
#35643=CARTESIAN_POINT('',(2.68467875173176,1.43,12.6));
#35644=CARTESIAN_POINT('Origin',(2.58075570327763,1.49,12.6));
#35645=CARTESIAN_POINT('Origin',(2.31433560763776,3.2114531418056,12.25));
#35646=CARTESIAN_POINT('',(2.21041255918363,3.1514531418056,11.9));
#35647=CARTESIAN_POINT('',(2.21041255918363,3.1514531418056,12.25));
#35648=CARTESIAN_POINT('',(2.24586286313301,3.31,11.9));
#35649=CARTESIAN_POINT('Origin',(2.31433560763776,3.2114531418056,11.9));
#35650=CARTESIAN_POINT('',(2.24586286313301,3.31,12.25));
#35651=CARTESIAN_POINT('Origin',(2.94448637286709,2.12,12.6));
#35652=CARTESIAN_POINT('',(2.84056332441296,2.06,11.9));
#35653=CARTESIAN_POINT('',(3.04840942132122,2.06,11.9));
#35654=CARTESIAN_POINT('Origin',(2.94448637286709,2.12,11.9));
#35655=CARTESIAN_POINT('',(2.84056332441296,2.06,12.6));
#35656=CARTESIAN_POINT('',(3.04840942132122,2.06,12.6));
#35657=CARTESIAN_POINT('Origin',(2.94448637286709,2.595,11.9));
#35658=CARTESIAN_POINT('',(2.11887548792593,3.31,11.9));
#35659=CARTESIAN_POINT('',(3.22514087125372,2.36610785057841,11.9));
#35660=CARTESIAN_POINT('',(2.94448637286709,1.88,11.9));
#35661=CARTESIAN_POINT('Origin',(0.,0.,11.9));
#35662=CARTESIAN_POINT('Origin',(3.77009725780826,3.31,12.6));
#35663=CARTESIAN_POINT('',(3.22514087125372,2.36610785057841,12.25));
#35664=CARTESIAN_POINT('Origin',(0.981495457622364,-2.12,12.6));
#35665=CARTESIAN_POINT('',(1.0854185060765,-2.06,11.9));
#35666=CARTESIAN_POINT('',(0.877572409168231,-2.06,11.9));
#35667=CARTESIAN_POINT('Origin',(0.981495457622364,-2.12,11.9));
#35668=CARTESIAN_POINT('',(1.0854185060765,-2.06,12.6));
#35669=CARTESIAN_POINT('',(0.877572409168231,-2.06,12.6));
#35670=CARTESIAN_POINT('Origin',(0.981495457622364,-1.88,12.6));
#35671=CARTESIAN_POINT('',(1.7031832941094,-3.13,11.9));
#35672=CARTESIAN_POINT('',(1.80710634256353,-3.31,11.9));
#35673=CARTESIAN_POINT('',(1.7031832941094,-3.13,12.6));
#35674=CARTESIAN_POINT('Origin',(0.363730669589464,-3.19,12.6));
#35675=CARTESIAN_POINT('',(0.259807621135332,-3.13,11.9));
#35676=CARTESIAN_POINT('',(0.363730669589464,-3.31,11.9));
#35677=CARTESIAN_POINT('Origin',(0.363730669589464,-3.19,11.9));
#35678=CARTESIAN_POINT('',(0.259807621135332,-3.13,12.6));
#35679=CARTESIAN_POINT('',(0.363730669589464,-3.31,12.6));
#35680=CARTESIAN_POINT('Origin',(0.981495457622364,-2.595,11.9));
#35681=CARTESIAN_POINT('',(0.981495457622364,-1.88,11.9));
#35682=CARTESIAN_POINT('',(1.59926024565526,-3.31,11.9));
#35683=CARTESIAN_POINT('',(0.155884572681199,-3.31,11.9));
#35684=CARTESIAN_POINT('Origin',(1.59926024565526,-3.19,11.9));
#35685=CARTESIAN_POINT('Origin',(1.80710634256353,-3.31,12.6));
#35686=CARTESIAN_POINT('',(1.59926024565526,-3.31,12.6));
#35687=CARTESIAN_POINT('Origin',(1.59926024565526,-3.19,12.6));
#35688=CARTESIAN_POINT('Origin',(1.96299091524473,-0.420000000000001,12.6));
#35689=CARTESIAN_POINT('',(2.06691396369886,-0.360000000000001,11.9));
#35690=CARTESIAN_POINT('',(1.85906786679059,-0.360000000000001,11.9));
#35691=CARTESIAN_POINT('Origin',(1.96299091524473,-0.420000000000001,11.9));
#35692=CARTESIAN_POINT('',(2.06691396369886,-0.36,12.6));
#35693=CARTESIAN_POINT('',(1.85906786679059,-0.360000000000001,12.6));
#35694=CARTESIAN_POINT('Origin',(1.96299091524473,-0.18,12.6));
#35695=CARTESIAN_POINT('',(2.68467875173176,-1.43,11.9));
#35696=CARTESIAN_POINT('',(2.78860180018589,-1.61,11.9));
#35697=CARTESIAN_POINT('',(2.68467875173176,-1.43,12.6));
#35698=CARTESIAN_POINT('Origin',(1.34522612721183,-1.49,12.6));
#35699=CARTESIAN_POINT('',(1.2413030787577,-1.43,11.9));
#35700=CARTESIAN_POINT('',(1.34522612721183,-1.61,11.9));
#35701=CARTESIAN_POINT('Origin',(1.34522612721183,-1.49,11.9));
#35702=CARTESIAN_POINT('',(1.2413030787577,-1.43,12.6));
#35703=CARTESIAN_POINT('',(1.34522612721183,-1.61,12.6));
#35704=CARTESIAN_POINT('Origin',(1.96299091524473,-0.895,11.9));
#35705=CARTESIAN_POINT('',(1.96299091524473,-0.18,11.9));
#35706=CARTESIAN_POINT('',(2.58075570327763,-1.61,11.9));
#35707=CARTESIAN_POINT('',(1.13738003030356,-1.61,11.9));
#35708=CARTESIAN_POINT('Origin',(2.58075570327763,-1.49,11.9));
#35709=CARTESIAN_POINT('Origin',(2.78860180018589,-1.61,12.6));
#35710=CARTESIAN_POINT('',(2.58075570327763,-1.61,12.6));
#35711=CARTESIAN_POINT('Origin',(2.58075570327763,-1.49,12.6));
#35712=CARTESIAN_POINT('Origin',(2.94448637286709,1.28,12.6));
#35713=CARTESIAN_POINT('',(3.04840942132122,1.34,11.9));
#35714=CARTESIAN_POINT('',(2.84056332441296,1.34,11.9));
#35715=CARTESIAN_POINT('Origin',(2.94448637286709,1.28,11.9));
#35716=CARTESIAN_POINT('',(3.04840942132122,1.34,12.6));
#35717=CARTESIAN_POINT('',(2.84056332441296,1.34,12.6));
#35718=CARTESIAN_POINT('Origin',(2.94448637286709,1.52,12.6));
#35719=CARTESIAN_POINT('',(3.66617420935412,0.27,11.9));
#35720=CARTESIAN_POINT('',(3.77009725780826,0.09,11.9));
#35721=CARTESIAN_POINT('',(3.66617420935412,0.27,12.6));
#35722=CARTESIAN_POINT('Origin',(2.32672158483419,0.21,12.6));
#35723=CARTESIAN_POINT('',(2.22279853638006,0.27,11.9));
#35724=CARTESIAN_POINT('',(2.32672158483419,0.09,11.9));
#35725=CARTESIAN_POINT('Origin',(2.32672158483419,0.21,11.9));
#35726=CARTESIAN_POINT('',(2.22279853638006,0.27,12.6));
#35727=CARTESIAN_POINT('',(2.32672158483419,0.09,12.6));
#35728=CARTESIAN_POINT('Origin',(2.94448637286709,0.805,11.9));
#35729=CARTESIAN_POINT('',(2.94448637286709,1.52,11.9));
#35730=CARTESIAN_POINT('',(3.56225116089999,0.09,11.9));
#35731=CARTESIAN_POINT('',(2.11887548792593,0.09,11.9));
#35732=CARTESIAN_POINT('Origin',(3.56225116089999,0.21,11.9));
#35733=CARTESIAN_POINT('Origin',(3.77009725780826,0.09,12.6));
#35734=CARTESIAN_POINT('',(3.56225116089999,0.09,12.6));
#35735=CARTESIAN_POINT('Origin',(3.56225116089999,0.21,12.6));
#35736=CARTESIAN_POINT('Origin',(3.30821704245656,-1.49,12.6));
#35737=CARTESIAN_POINT('',(3.20429399400242,-1.43,11.9));
#35738=CARTESIAN_POINT('',(3.30821704245656,-1.61,11.9));
#35739=CARTESIAN_POINT('Origin',(3.30821704245656,-1.49,11.9));
#35740=CARTESIAN_POINT('',(3.20429399400242,-1.43,12.6));
#35741=CARTESIAN_POINT('',(3.30821704245656,-1.61,12.6));
#35742=CARTESIAN_POINT('Origin',(3.92598183048946,-0.895,11.9));
#35743=CARTESIAN_POINT('',(3.92598183048946,-0.18,11.9));
#35744=CARTESIAN_POINT('',(3.66167994232156,-1.61,11.9));
#35745=CARTESIAN_POINT('',(3.10037094554829,-1.61,11.9));
#35746=CARTESIAN_POINT('Origin',(0.,0.,11.9));
#35747=CARTESIAN_POINT('Origin',(4.75159271543062,-1.61,12.6));
#35748=CARTESIAN_POINT('',(3.66167994232156,-1.61,12.25));
#35749=CARTESIAN_POINT('Origin',(2.94448637286709,-2.12,12.6));
#35750=CARTESIAN_POINT('',(3.04840942132122,-2.06,11.9));
#35751=CARTESIAN_POINT('',(2.84056332441296,-2.06,11.9));
#35752=CARTESIAN_POINT('Origin',(2.94448637286709,-2.12,11.9));
#35753=CARTESIAN_POINT('',(3.04840942132122,-2.06,12.6));
#35754=CARTESIAN_POINT('',(2.84056332441296,-2.06,12.6));
#35755=CARTESIAN_POINT('Origin',(2.94448637286709,-1.88,12.6));
#35756=CARTESIAN_POINT('',(3.22514087125372,-2.36610785057841,11.9));
#35757=CARTESIAN_POINT('',(3.77009725780826,-3.31,11.9));
#35758=CARTESIAN_POINT('',(3.22514087125372,-2.36610785057841,12.25));
#35759=CARTESIAN_POINT('Origin',(2.31433560763776,-3.2114531418056,12.25));
#35760=CARTESIAN_POINT('',(2.21041255918363,-3.1514531418056,11.9));
#35761=CARTESIAN_POINT('',(2.24586286313301,-3.31,11.9));
#35762=CARTESIAN_POINT('Origin',(2.31433560763776,-3.2114531418056,11.9));
#35763=CARTESIAN_POINT('',(2.21041255918363,-3.1514531418056,12.25));
#35764=CARTESIAN_POINT('',(2.24586286313301,-3.31,12.25));
#35765=CARTESIAN_POINT('Origin',(2.94448637286709,-2.595,11.9));
#35766=CARTESIAN_POINT('',(2.94448637286709,-1.88,11.9));
#35767=CARTESIAN_POINT('Origin',(0.,0.,11.9));
#35768=CARTESIAN_POINT('Origin',(0.363730669589464,-3.61,12.6));
#35769=CARTESIAN_POINT('',(0.363730669589464,-3.49,11.9));
#35770=CARTESIAN_POINT('',(0.259807621135332,-3.67,11.9));
#35771=CARTESIAN_POINT('Origin',(0.363730669589464,-3.61,11.9));
#35772=CARTESIAN_POINT('',(0.363730669589464,-3.49,12.6));
#35773=CARTESIAN_POINT('',(0.259807621135332,-3.67,12.6));
#35774=CARTESIAN_POINT('Origin',(0.981495457622364,-4.205,11.9));
#35775=CARTESIAN_POINT('',(1.80710634256353,-3.49,11.9));
#35776=CARTESIAN_POINT('',(0.436539071067832,-3.97610785057841,11.9));
#35777=CARTESIAN_POINT('',(0.155884572681199,-3.49,11.9));
#35778=CARTESIAN_POINT('Origin',(0.,0.,11.9));
#35779=CARTESIAN_POINT('Origin',(0.981495457622364,-4.92,12.6));
#35780=CARTESIAN_POINT('',(0.436539071067833,-3.97610785057841,12.25));
#35781=CARTESIAN_POINT('Origin',(-1.62403220004812,-3.61,12.25));
#35782=CARTESIAN_POINT('',(-1.62403220004812,-3.49,11.9));
#35783=CARTESIAN_POINT('',(-1.74361265495999,-3.59997429288924,11.9));
#35784=CARTESIAN_POINT('Origin',(-1.62403220004812,-3.61,11.9));
#35785=CARTESIAN_POINT('',(-1.62403220004812,-3.49,12.25));
#35786=CARTESIAN_POINT('',(-1.74361265495999,-3.59997429288924,12.25));
#35787=CARTESIAN_POINT('Origin',(-0.981495457622364,-4.205,11.9));
#35788=CARTESIAN_POINT('',(-0.155884572681199,-3.49,11.9));
#35789=CARTESIAN_POINT('Origin',(0.,0.,11.9));
#35790=CARTESIAN_POINT('Origin',(-2.94448637286709,-2.12,12.6));
#35791=CARTESIAN_POINT('',(-2.84056332441296,-2.06,11.9));
#35792=CARTESIAN_POINT('',(-3.04840942132122,-2.06,11.9));
#35793=CARTESIAN_POINT('Origin',(-2.94448637286709,-2.12,11.9));
#35794=CARTESIAN_POINT('',(-2.84056332441296,-2.06,12.6));
#35795=CARTESIAN_POINT('',(-3.04840942132122,-2.06,12.6));
#35796=CARTESIAN_POINT('Origin',(-2.94448637286709,-2.595,11.9));
#35797=CARTESIAN_POINT('',(-2.11887548792593,-3.31,11.9));
#35798=CARTESIAN_POINT('',(-3.22514087125372,-2.36610785057841,11.9));
#35799=CARTESIAN_POINT('',(-2.94448637286709,-1.88,11.9));
#35800=CARTESIAN_POINT('Origin',(0.,0.,11.9));
#35801=CARTESIAN_POINT('Origin',(-3.77009725780826,-3.31,12.6));
#35802=CARTESIAN_POINT('',(-3.22514087125372,-2.36610785057841,12.25));
#35803=CARTESIAN_POINT('Origin',(-3.93836780768588,-0.398546858194397,12.25));
#35804=CARTESIAN_POINT('',(-3.83444475923175,-0.338546858194397,11.9));
#35805=CARTESIAN_POINT('',(-3.989475518093,-0.289974292889239,11.9));
#35806=CARTESIAN_POINT('Origin',(-3.93836780768588,-0.398546858194397,11.9));
#35807=CARTESIAN_POINT('',(-3.83444475923175,-0.338546858194397,12.25));
#35808=CARTESIAN_POINT('',(-3.989475518093,-0.289974292889239,12.25));
#35809=CARTESIAN_POINT('Origin',(-3.92598183048946,-0.895,11.9));
#35810=CARTESIAN_POINT('',(-3.10037094554829,-1.61,11.9));
#35811=CARTESIAN_POINT('Origin',(0.,0.,11.9));
#35812=CARTESIAN_POINT('Origin',(0.,0.,12.25));
#35813=CARTESIAN_POINT('Origin',(0.,0.,12.25));
#35814=CARTESIAN_POINT('Origin',(0.,0.,12.25));
#35815=CARTESIAN_POINT('Origin',(0.,0.,12.25));
#35816=CARTESIAN_POINT('Origin',(0.,0.,12.25));
#35817=CARTESIAN_POINT('Origin',(0.,0.,12.25));
#35818=CARTESIAN_POINT('',(0.436539071067832,3.97610785057841,12.25));
#35819=CARTESIAN_POINT('Origin',(0.,0.,12.25));
#35820=CARTESIAN_POINT('Origin',(0.,0.,12.25));
#35821=CARTESIAN_POINT('Origin',(0.,0.,12.25));
#35822=CARTESIAN_POINT('Origin',(0.,0.,12.25));
#35823=CARTESIAN_POINT('',(-3.22514087125372,2.36610785057841,12.25));
#35824=CARTESIAN_POINT('Origin',(0.,0.,12.25));
#35825=CARTESIAN_POINT('Origin',(0.,0.,12.25));
#35826=CARTESIAN_POINT('Origin',(2.11887548792593,-3.31,12.6));
#35827=CARTESIAN_POINT('Origin',(2.11887548792593,0.0900000000000001,12.6));
#35828=CARTESIAN_POINT('Origin',(1.13738003030356,-1.61,12.6));
#35829=CARTESIAN_POINT('Origin',(0.155884572681199,-3.31,12.6));
#35830=CARTESIAN_POINT('Origin',(2.94448637286709,1.88,12.6));
#35831=CARTESIAN_POINT('Origin',(1.96299091524473,0.18,12.6));
#35832=CARTESIAN_POINT('Origin',(-1.80710634256353,-3.31,12.6));
#35833=CARTESIAN_POINT('Origin',(0.981495457622364,1.88,12.6));
#35834=CARTESIAN_POINT('Origin',(-2.78860180018589,-1.61,12.6));
#35835=CARTESIAN_POINT('Origin',(-2.94448637286709,-1.88,12.6));
#35836=CARTESIAN_POINT('Origin',(-0.981495457622364,1.88,12.6));
#35837=CARTESIAN_POINT('Origin',(-1.96299091524473,0.18,12.6));
#35838=CARTESIAN_POINT('Origin',(-2.94448637286709,-1.52,12.6));
#35839=CARTESIAN_POINT('Origin',(-2.94448637286709,1.88,12.6));
#35840=CARTESIAN_POINT('Origin',(-3.92598183048946,-0.18,12.6));
#35841=CARTESIAN_POINT('Origin',(-3.77009725780826,0.0900000000000001,12.6));
#35842=CARTESIAN_POINT('Origin',(-2.78860180018589,1.79,12.6));
#35843=CARTESIAN_POINT('Origin',(-1.96299091524473,-3.22,12.6));
#35844=CARTESIAN_POINT('Origin',(-0.825610884941165,1.79,12.6));
#35845=CARTESIAN_POINT('Origin',(0.155884572681199,3.49,12.6));
#35846=CARTESIAN_POINT('Origin',(-1.80710634256353,-3.49,12.6));
#35847=CARTESIAN_POINT('Origin',(0.,-3.22,12.6));
#35848=CARTESIAN_POINT('Origin',(1.13738003030356,1.79,12.6));
#35849=CARTESIAN_POINT('Origin',(0.155884572681199,-3.49,12.6));
#35850=CARTESIAN_POINT('Origin',(1.96299091524473,-3.22,12.6));
#35851=CARTESIAN_POINT('Origin',(2.94448637286709,-1.52,12.6));
#35852=CARTESIAN_POINT('Origin',(3.92598183048946,0.18,12.6));
#35853=CARTESIAN_POINT('Origin',(3.10037094554829,-1.61,12.6));
#35854=CARTESIAN_POINT('Origin',(0.,0.,11.3));
#35855=CARTESIAN_POINT('',(-3.8,-4.65365783675994E-16,11.2));
#35856=CARTESIAN_POINT('',(-3.8,-4.65365783675994E-16,11.3));
#35857=CARTESIAN_POINT('Origin',(0.,0.,11.2));
#35858=CARTESIAN_POINT('Origin',(4.095,0.,11.2));
#35859=CARTESIAN_POINT('',(-4.095,-5.01492864250841E-16,11.2));
#35860=CARTESIAN_POINT('Origin',(0.,0.,11.2));
#35861=CARTESIAN_POINT('Origin',(0.,0.,11.3));
#35862=CARTESIAN_POINT('',(-4.095,-5.01492864250841E-16,11.3));
#35863=CARTESIAN_POINT('Origin',(0.,0.,12.2));
#35864=CARTESIAN_POINT('',(-0.9025,-1.10524373623049E-16,12.2));
#35865=CARTESIAN_POINT('',(0.,0.,0.));
#35866=CARTESIAN_POINT('Origin',(0.,0.,12.785));
#35867=CARTESIAN_POINT('',(1.02,-1.2491397351303E-16,12.8));
#35868=CARTESIAN_POINT('Origin',(0.,0.,12.8));
#35869=CARTESIAN_POINT('',(1.05,1.28587913910472E-16,12.77));
#35870=CARTESIAN_POINT('',(1.035,1.26750943711751E-16,12.785));
#35871=CARTESIAN_POINT('',(-1.05,-1.28587913910472E-16,12.77));
#35872=CARTESIAN_POINT('Origin',(0.,0.,12.77));
#35873=CARTESIAN_POINT('Origin',(0.,0.,12.77));
#35874=CARTESIAN_POINT('Origin',(0.,0.,12.7));
#35875=CARTESIAN_POINT('',(-1.05,-1.28587913910472E-16,12.63));
#35876=CARTESIAN_POINT('',(-1.05,-1.28587913910472E-16,12.7));
#35877=CARTESIAN_POINT('',(1.05,-1.28587913910472E-16,12.63));
#35878=CARTESIAN_POINT('Origin',(0.,0.,12.63));
#35879=CARTESIAN_POINT('Origin',(0.,0.,12.63));
#35880=CARTESIAN_POINT('Origin',(0.9,0.,12.8));
#35881=CARTESIAN_POINT('',(-0.9,-1.10218211923262E-16,12.8));
#35882=CARTESIAN_POINT('Origin',(0.,0.,12.8));
#35883=CARTESIAN_POINT('Origin',(0.,0.,12.615));
#35884=CARTESIAN_POINT('',(1.02,1.2491397351303E-16,12.6));
#35885=CARTESIAN_POINT('',(1.035,1.26750943711751E-16,12.615));
#35886=CARTESIAN_POINT('Origin',(0.,0.,12.6));
#35887=CARTESIAN_POINT('Origin',(1.05,0.,12.6));
#35888=CARTESIAN_POINT('',(-0.9,-1.10218211923262E-16,12.6));
#35889=CARTESIAN_POINT('Origin',(0.,0.,12.6));
#35890=CARTESIAN_POINT('Origin',(0.,-1.92510434439678E-17,17.9893933982822));
#35891=CARTESIAN_POINT('',(0.628786796564401,-1.54008347551742E-16,17.9787867965644));
#35892=CARTESIAN_POINT('Origin',(0.,-3.85020868879356E-17,17.9787867965644));
#35893=CARTESIAN_POINT('',(0.679999999999998,8.32759823420198E-17,18.));
#35894=CARTESIAN_POINT('',(0.6543933982822,-1.18642164946881E-16,17.9893933982822));
#35895=CARTESIAN_POINT('Origin',(0.,0.,18.));
#35896=CARTESIAN_POINT('Origin',(0.,0.,17.975));
#35897=CARTESIAN_POINT('',(0.621213203435595,0.,17.9712132034356));
#35898=CARTESIAN_POINT('Origin',(0.,-3.80383380587737E-17,17.9712132034356));
#35899=CARTESIAN_POINT('',(0.625,-7.65404249467096E-17,17.975));
#35900=CARTESIAN_POINT('Origin',(0.6,0.,18.));
#35901=CARTESIAN_POINT('',(-1.1,-1.34711147906209E-16,18.));
#35902=CARTESIAN_POINT('Origin',(0.,0.,18.));
#35903=CARTESIAN_POINT('Origin',(0.,-1.90191690293869E-17,17.9456066017178));
#35904=CARTESIAN_POINT('',(0.6,-7.34788079488412E-17,17.92));
#35905=CARTESIAN_POINT('',(0.610606601717797,3.67394039744206E-17,17.9456066017178));
#35906=CARTESIAN_POINT('',(-0.6,-7.34788079488412E-17,17.92));
#35907=CARTESIAN_POINT('Origin',(0.,0.,17.92));
#35908=CARTESIAN_POINT('Origin',(0.,0.,17.92));
#35909=CARTESIAN_POINT('Origin',(0.,0.,14.9));
#35910=CARTESIAN_POINT('',(-0.6,-7.34788079488412E-17,11.88));
#35911=CARTESIAN_POINT('',(-0.6,-7.34788079488412E-17,14.9));
#35912=CARTESIAN_POINT('',(0.6,7.34788079488412E-17,11.88));
#35913=CARTESIAN_POINT('Origin',(0.,0.,11.88));
#35914=CARTESIAN_POINT('Origin',(0.,0.,11.88));
#35915=CARTESIAN_POINT('Origin',(0.,-1.90191690293869E-17,11.8543933982822));
#35916=CARTESIAN_POINT('',(0.621213203435596,-1.52153352235095E-16,11.8287867965644));
#35917=CARTESIAN_POINT('Origin',(0.,-3.80383380587738E-17,11.8287867965644));
#35918=CARTESIAN_POINT('',(0.610606601717798,-1.12816080091968E-16,11.8543933982822));
#35919=CARTESIAN_POINT('Origin',(0.,0.,11.825));
#35920=CARTESIAN_POINT('',(0.628786796564403,0.,11.8212132034356));
#35921=CARTESIAN_POINT('Origin',(0.,-3.85020868879357E-17,11.8212132034356));
#35922=CARTESIAN_POINT('',(0.625,-7.65404249467096E-17,11.825));
#35923=CARTESIAN_POINT('Origin',(0.,-1.92510434439679E-17,11.8106066017178));
#35924=CARTESIAN_POINT('',(0.68,-8.327598234202E-17,11.8));
#35925=CARTESIAN_POINT('',(0.654393398282201,4.163799117101E-17,11.8106066017178));
#35926=CARTESIAN_POINT('Origin',(0.,0.,11.8));
#35927=CARTESIAN_POINT('Origin',(0.9,0.,11.8));
#35928=CARTESIAN_POINT('',(0.86,1.05319624726672E-16,11.8));
#35929=CARTESIAN_POINT('Origin',(0.,0.,11.8));
#35930=CARTESIAN_POINT('Origin',(0.,0.,11.82));
#35931=CARTESIAN_POINT('',(0.9,-1.10218211923262E-16,11.84));
#35932=CARTESIAN_POINT('',(-0.9,-1.10218211923262E-16,11.84));
#35933=CARTESIAN_POINT('Origin',(0.,0.,11.84));
#35934=CARTESIAN_POINT('Origin',(0.,0.,11.84));
#35935=CARTESIAN_POINT('',(0.88,1.07768918324967E-16,11.82));
#35936=CARTESIAN_POINT('Origin',(0.,0.,12.2));
#35937=CARTESIAN_POINT('',(-0.9,-1.10218211923262E-16,12.2));
#35938=CARTESIAN_POINT('Origin',(0.,0.,17.9));
#35939=CARTESIAN_POINT('',(-1.2,-1.46957615897682E-16,17.9));
#35940=CARTESIAN_POINT('Origin',(-1.1,-1.34711147906209E-16,17.9));
#35941=CARTESIAN_POINT('Origin',(0.,0.,17.9));
#35942=CARTESIAN_POINT('Origin',(0.,0.,17.5));
#35943=CARTESIAN_POINT('',(-1.2,-1.46957615897682E-16,17.0333333333333));
#35944=CARTESIAN_POINT('',(-1.2,-1.46957615897682E-16,17.5));
#35945=CARTESIAN_POINT('Origin',(0.,0.,17.0333333333333));
#35946=CARTESIAN_POINT('Origin',(0.,0.,17.0333333333333));
#35947=CARTESIAN_POINT('',(-1.18,-1.44508322299388E-16,16.9733333333333));
#35948=CARTESIAN_POINT('Origin',(-1.1,-1.34711147906209E-16,17.0333333333333));
#35949=CARTESIAN_POINT('Origin',(0.,-1.44508322299388E-16,16.9733333333333));
#35950=CARTESIAN_POINT('Origin',(0.,0.,16.8));
#35951=CARTESIAN_POINT('',(-0.9,-1.10218211923262E-16,16.6));
#35952=CARTESIAN_POINT('',(-1.05,-1.28587913910472E-16,16.8));
#35953=CARTESIAN_POINT('Origin',(0.,0.,16.6));
#35954=CARTESIAN_POINT('Origin',(0.,0.,14.7));
#35955=CARTESIAN_POINT('',(-0.9,-1.10218211923262E-16,14.7));
#35956=CARTESIAN_POINT('',(0.,0.,0.));
#35957=CARTESIAN_POINT('Origin',(0.,0.,12.615));
#35958=CARTESIAN_POINT('',(1.095,-1.34098824506635E-16,12.6));
#35959=CARTESIAN_POINT('Origin',(0.,0.,12.6));
#35960=CARTESIAN_POINT('',(1.065,1.30424884109193E-16,12.63));
#35961=CARTESIAN_POINT('',(1.08,-1.32261854307914E-16,12.615));
#35962=CARTESIAN_POINT('',(-1.065,-1.30424884109193E-16,12.63));
#35963=CARTESIAN_POINT('Origin',(0.,0.,12.63));
#35964=CARTESIAN_POINT('Origin',(0.,0.,12.63));
#35965=CARTESIAN_POINT('Origin',(1.55,0.,12.6));
#35966=CARTESIAN_POINT('',(1.47,1.80023079474661E-16,12.6));
#35967=CARTESIAN_POINT('Origin',(0.,0.,12.6));
#35968=CARTESIAN_POINT('',(-0.128333333333334,-1.28,12.6));
#35969=CARTESIAN_POINT('Origin',(0.,-1.28,12.6));
#35970=CARTESIAN_POINT('',(-0.128333333333334,1.28,12.6));
#35971=CARTESIAN_POINT('Origin',(0.,1.28,12.6));
#35972=CARTESIAN_POINT('Origin',(0.,0.,12.7));
#35973=CARTESIAN_POINT('',(-1.065,-1.30424884109193E-16,12.8));
#35974=CARTESIAN_POINT('Origin',(0.,0.,12.8));
#35975=CARTESIAN_POINT('',(-1.065,-1.30424884109193E-16,12.7));
#35976=CARTESIAN_POINT('Origin',(0.,4.65737220102024E-17,12.6106066017178));
#35977=CARTESIAN_POINT('',(1.5212132034356,0.,12.6212132034356));
#35978=CARTESIAN_POINT('Origin',(0.,9.31474440204048E-17,12.6212132034356));
#35979=CARTESIAN_POINT('',(1.4956066017178,2.7630642777814E-16,12.6106066017178));
#35980=CARTESIAN_POINT('Origin',(0.,0.,12.625));
#35981=CARTESIAN_POINT('',(1.5287867965644,3.74444771398267E-16,12.6287867965644));
#35982=CARTESIAN_POINT('Origin',(0.,9.36111928495666E-17,12.6287867965644));
#35983=CARTESIAN_POINT('',(1.525,1.86758636869971E-16,12.625));
#35984=CARTESIAN_POINT('Origin',(0.,4.68055964247833E-17,12.6543933982822));
#35985=CARTESIAN_POINT('',(1.55,-1.8982025386784E-16,12.68));
#35986=CARTESIAN_POINT('',(1.5393933982822,-9.49101269339199E-17,12.6543933982822));
#35987=CARTESIAN_POINT('',(-1.55,-1.8982025386784E-16,12.68));
#35988=CARTESIAN_POINT('Origin',(0.,0.,12.68));
#35989=CARTESIAN_POINT('Origin',(0.,0.,12.68));
#35990=CARTESIAN_POINT('Origin',(0.,0.,13.));
#35991=CARTESIAN_POINT('',(1.55,1.8982025386784E-16,13.32));
#35992=CARTESIAN_POINT('',(-1.55,-1.8982025386784E-16,13.32));
#35993=CARTESIAN_POINT('Origin',(0.,0.,13.32));
#35994=CARTESIAN_POINT('Origin',(0.,0.,13.32));
#35995=CARTESIAN_POINT('',(-1.55,-1.8982025386784E-16,13.));
#35996=CARTESIAN_POINT('Origin',(0.,4.68055964247833E-17,13.3456066017178));
#35997=CARTESIAN_POINT('',(1.5287867965644,0.,13.3712132034356));
#35998=CARTESIAN_POINT('Origin',(0.,9.36111928495666E-17,13.3712132034356));
#35999=CARTESIAN_POINT('',(1.5393933982822,2.82132512633053E-16,13.3456066017178));
#36000=CARTESIAN_POINT('Origin',(0.,0.,13.375));
#36001=CARTESIAN_POINT('',(1.5212132034356,3.72589776081619E-16,13.3787867965644));
#36002=CARTESIAN_POINT('Origin',(0.,9.31474440204048E-17,13.3787867965644));
#36003=CARTESIAN_POINT('',(1.525,1.86758636869971E-16,13.375));
#36004=CARTESIAN_POINT('Origin',(0.,0.,12.815));
#36005=CARTESIAN_POINT('',(0.94,-1.15116799119851E-16,12.8));
#36006=CARTESIAN_POINT('Origin',(0.,0.,12.8));
#36007=CARTESIAN_POINT('',(0.91,1.11442858722409E-16,12.83));
#36008=CARTESIAN_POINT('',(0.925,-1.1327982892113E-16,12.815));
#36009=CARTESIAN_POINT('',(-0.91,-1.11442858722409E-16,12.83));
#36010=CARTESIAN_POINT('Origin',(0.,0.,12.83));
#36011=CARTESIAN_POINT('Origin',(0.,0.,12.83));
#36012=CARTESIAN_POINT('Origin',(0.,0.,13.1));
#36013=CARTESIAN_POINT('',(0.91,-1.11442858722409E-16,13.36));
#36014=CARTESIAN_POINT('',(-0.91,-1.11442858722409E-16,13.36));
#36015=CARTESIAN_POINT('Origin',(0.,0.,13.36));
#36016=CARTESIAN_POINT('Origin',(0.,0.,13.36));
#36017=CARTESIAN_POINT('',(-0.91,-1.11442858722409E-16,13.1));
#36018=CARTESIAN_POINT('Origin',(1.065,0.,12.8));
#36019=CARTESIAN_POINT('Origin',(0.,4.65737220102024E-17,13.3893933982822));
#36020=CARTESIAN_POINT('',(1.46999999999999,-1.34246756157856E-16,13.4));
#36021=CARTESIAN_POINT('',(1.4956066017178,-9.00115397373305E-17,13.3893933982822));
#36022=CARTESIAN_POINT('',(0.156910396397301,-1.4616015625,13.4));
#36023=CARTESIAN_POINT('Origin',(0.,0.,13.4));
#36024=CARTESIAN_POINT('',(-0.156910396397301,-1.4616015625,13.4));
#36025=CARTESIAN_POINT('Ctrl Pts',(-0.156910396397299,-1.4616015625,13.4));
#36026=CARTESIAN_POINT('Ctrl Pts',(-0.149656402785207,-1.46593468366903,
13.3985361440069));
#36027=CARTESIAN_POINT('Ctrl Pts',(-0.142213279389795,-1.4699883651202,
13.3971707806262));
#36028=CARTESIAN_POINT('Ctrl Pts',(-0.0924978887707845,-1.49450064049362,
13.3889327354826));
#36029=CARTESIAN_POINT('Ctrl Pts',(-0.0452361545939354,-1.50535533905932,
13.3853553390593));
#36030=CARTESIAN_POINT('Ctrl Pts',(0.0452361545939354,-1.50535533905932,
13.3853553390593));
#36031=CARTESIAN_POINT('Ctrl Pts',(0.0924978887707845,-1.49450064049362,
13.3889327354826));
#36032=CARTESIAN_POINT('Ctrl Pts',(0.142213279389795,-1.4699883651202,13.3971707806262));
#36033=CARTESIAN_POINT('Ctrl Pts',(0.149656402785207,-1.46593468366903,
13.3985361440069));
#36034=CARTESIAN_POINT('Ctrl Pts',(0.156910396397299,-1.4616015625,13.4));
#36035=CARTESIAN_POINT('',(-0.156910396397301,1.4616015625,13.4));
#36036=CARTESIAN_POINT('Origin',(0.,0.,13.4));
#36037=CARTESIAN_POINT('',(0.156910396397301,1.4616015625,13.4));
#36038=CARTESIAN_POINT('Ctrl Pts',(0.156910396397303,1.4616015625,13.4));
#36039=CARTESIAN_POINT('Ctrl Pts',(0.149656402785211,1.46593468366904,13.3985361440069));
#36040=CARTESIAN_POINT('Ctrl Pts',(0.1422132793898,1.46998836512021,13.3971707806262));
#36041=CARTESIAN_POINT('Ctrl Pts',(0.0924978887707876,1.49450064049363,
13.3889327354826));
#36042=CARTESIAN_POINT('Ctrl Pts',(0.0452361545939373,1.50535533905933,
13.3853553390593));
#36043=CARTESIAN_POINT('Ctrl Pts',(-0.0452361545939372,1.50535533905933,
13.3853553390593));
#36044=CARTESIAN_POINT('Ctrl Pts',(-0.0924978887707876,1.49450064049363,
13.3889327354826));
#36045=CARTESIAN_POINT('Ctrl Pts',(-0.1422132793898,1.46998836512021,13.3971707806262));
#36046=CARTESIAN_POINT('Ctrl Pts',(-0.149656402785211,1.46593468366904,
13.3985361440069));
#36047=CARTESIAN_POINT('Ctrl Pts',(-0.156910396397303,1.4616015625,13.4));
#36048=CARTESIAN_POINT('Origin',(0.,0.,13.4));
#36049=CARTESIAN_POINT('Origin',(0.,1.28,13.385));
#36050=CARTESIAN_POINT('',(0.240000000000004,1.28,13.4));
#36051=CARTESIAN_POINT('Origin',(0.,1.28,13.4));
#36052=CARTESIAN_POINT('',(0.21,1.28,13.37));
#36053=CARTESIAN_POINT('',(0.225,1.28,13.385));
#36054=CARTESIAN_POINT('',(-0.21,1.28,13.37));
#36055=CARTESIAN_POINT('Origin',(0.,1.28,13.37));
#36056=CARTESIAN_POINT('Origin',(0.,1.28,13.37));
#36057=CARTESIAN_POINT('Origin',(0.,1.28,13.4));
#36058=CARTESIAN_POINT('Origin',(0.,1.28,13.29));
#36059=CARTESIAN_POINT('',(-0.21,1.28,13.18));
#36060=CARTESIAN_POINT('Origin',(0.,1.28,13.18));
#36061=CARTESIAN_POINT('',(-0.21,1.28,13.29));
#36062=CARTESIAN_POINT('Origin',(0.,-1.28,13.385));
#36063=CARTESIAN_POINT('',(0.24,-1.28,13.4));
#36064=CARTESIAN_POINT('Origin',(0.,-1.28,13.4));
#36065=CARTESIAN_POINT('',(0.21,-1.28,13.37));
#36066=CARTESIAN_POINT('',(0.225,-1.28,13.385));
#36067=CARTESIAN_POINT('',(-0.21,-1.28,13.37));
#36068=CARTESIAN_POINT('Origin',(0.,-1.28,13.37));
#36069=CARTESIAN_POINT('Origin',(0.,-1.28,13.37));
#36070=CARTESIAN_POINT('Origin',(0.,-1.28,13.4));
#36071=CARTESIAN_POINT('Origin',(0.,-1.28,13.29));
#36072=CARTESIAN_POINT('',(-0.21,-1.28,13.18));
#36073=CARTESIAN_POINT('Origin',(0.,-1.28,13.18));
#36074=CARTESIAN_POINT('',(-0.21,-1.28,13.29));
#36075=CARTESIAN_POINT('Origin',(0.,-1.28,12.5875));
#36076=CARTESIAN_POINT('',(-0.12,-1.28,12.625));
#36077=CARTESIAN_POINT('',(-0.1325,-1.28,12.5875));
#36078=CARTESIAN_POINT('Origin',(0.,-1.28,12.625));
#36079=CARTESIAN_POINT('Origin',(0.,-1.28,12.89));
#36080=CARTESIAN_POINT('',(-0.12,-1.28,13.155));
#36081=CARTESIAN_POINT('',(-0.12,-1.28,12.89));
#36082=CARTESIAN_POINT('Origin',(0.,-1.28,13.155));
#36083=CARTESIAN_POINT('Origin',(0.,-1.28,13.1675));
#36084=CARTESIAN_POINT('',(-0.145,-1.28,13.18));
#36085=CARTESIAN_POINT('',(-0.1325,-1.28,13.1675));
#36086=CARTESIAN_POINT('Origin',(0.,-1.28,13.18));
#36087=CARTESIAN_POINT('Origin',(0.21,-1.28,13.18));
#36088=CARTESIAN_POINT('Origin',(0.,1.28,12.5875));
#36089=CARTESIAN_POINT('',(-0.12,1.28,12.625));
#36090=CARTESIAN_POINT('',(-0.1325,1.28,12.5875));
#36091=CARTESIAN_POINT('Origin',(0.,1.28,12.625));
#36092=CARTESIAN_POINT('Origin',(0.,1.28,12.89));
#36093=CARTESIAN_POINT('',(-0.12,1.28,13.155));
#36094=CARTESIAN_POINT('',(-0.12,1.28,12.89));
#36095=CARTESIAN_POINT('Origin',(0.,1.28,13.155));
#36096=CARTESIAN_POINT('Origin',(0.,1.28,13.1675));
#36097=CARTESIAN_POINT('',(-0.145,1.28,13.18));
#36098=CARTESIAN_POINT('',(-0.1325,1.28,13.1675));
#36099=CARTESIAN_POINT('Origin',(0.,1.28,13.18));
#36100=CARTESIAN_POINT('Origin',(0.21,1.28,13.18));
#36101=CARTESIAN_POINT('Origin',(0.,0.,13.38));
#36102=CARTESIAN_POINT('',(0.95,1.16341445918999E-16,13.4));
#36103=CARTESIAN_POINT('',(0.93,-1.13892152320704E-16,13.38));
#36104=CARTESIAN_POINT('Origin',(0.,0.,13.4));
#36105=CARTESIAN_POINT('Origin',(0.91,0.,13.4));
#36106=CARTESIAN_POINT('',(0.,0.,0.));
#36107=CARTESIAN_POINT('Origin',(-2.25166604983954,1.3,10.25));
#36108=CARTESIAN_POINT('',(-2.70166604983954,1.3,10.1));
#36109=CARTESIAN_POINT('Origin',(-2.25166604983954,1.3,10.1));
#36110=CARTESIAN_POINT('',(-2.70166604983954,1.3,10.4));
#36111=CARTESIAN_POINT('',(-2.70166604983954,1.3,10.25));
#36112=CARTESIAN_POINT('Origin',(-2.25166604983954,1.3,10.4));
#36113=CARTESIAN_POINT('Origin',(2.25166604983954,1.3,10.25));
#36114=CARTESIAN_POINT('',(1.80166604983954,1.3,10.1));
#36115=CARTESIAN_POINT('Origin',(2.25166604983954,1.3,10.1));
#36116=CARTESIAN_POINT('',(1.80166604983954,1.3,10.4));
#36117=CARTESIAN_POINT('',(1.80166604983954,1.3,10.25));
#36118=CARTESIAN_POINT('Origin',(2.25166604983954,1.3,10.4));
#36119=CARTESIAN_POINT('Origin',(2.90118510267787,0.0750000000000004,10.215));
#36120=CARTESIAN_POINT('',(2.77118510267787,0.0750000000000003,10.1));
#36121=CARTESIAN_POINT('Origin',(2.90118510267787,0.0750000000000004,10.1));
#36122=CARTESIAN_POINT('',(2.77118510267787,0.0750000000000003,10.35));
#36123=CARTESIAN_POINT('',(2.77118510267787,0.0750000000000003,10.215));
#36124=CARTESIAN_POINT('Origin',(2.90118510267787,0.0750000000000004,10.35));
#36125=CARTESIAN_POINT('Origin',(2.90118510267787,0.0750000000000004,10.4));
#36126=CARTESIAN_POINT('',(2.72118510267787,0.0750000000000004,10.4));
#36127=CARTESIAN_POINT('',(2.72118510267787,0.0750000000000003,10.4));
#36128=CARTESIAN_POINT('Origin',(2.90118510267787,0.0750000000000004,10.4));
#36129=CARTESIAN_POINT('Origin',(2.94448637286709,-1.7,10.25));
#36130=CARTESIAN_POINT('',(2.79948637286709,-1.7,10.1));
#36131=CARTESIAN_POINT('Origin',(2.94448637286709,-1.7,10.1));
#36132=CARTESIAN_POINT('',(2.79948637286709,-1.7,10.4));
#36133=CARTESIAN_POINT('',(2.79948637286709,-1.7,10.25));
#36134=CARTESIAN_POINT('Origin',(2.94448637286709,-1.7,10.4));
#36135=CARTESIAN_POINT('Origin',(-2.94448637286709,-1.7,10.25));
#36136=CARTESIAN_POINT('',(-3.08948637286709,-1.7,10.1));
#36137=CARTESIAN_POINT('Origin',(-2.94448637286709,-1.7,10.1));
#36138=CARTESIAN_POINT('',(-3.08948637286709,-1.7,10.4));
#36139=CARTESIAN_POINT('',(-3.08948637286709,-1.7,10.25));
#36140=CARTESIAN_POINT('Origin',(-2.94448637286709,-1.7,10.4));
#36141=CARTESIAN_POINT('Origin',(2.0818995585505E-16,3.4,10.25));
#36142=CARTESIAN_POINT('',(-0.145,3.4,10.1));
#36143=CARTESIAN_POINT('Origin',(2.0818995585505E-16,3.4,10.1));
#36144=CARTESIAN_POINT('',(-0.145,3.4,10.4));
#36145=CARTESIAN_POINT('',(-0.145,3.4,10.25));
#36146=CARTESIAN_POINT('Origin',(2.0818995585505E-16,3.4,10.4));
#36147=CARTESIAN_POINT('Origin',(-0.65,-1.6,10.25));
#36148=CARTESIAN_POINT('',(-0.745,-1.6,10.1));
#36149=CARTESIAN_POINT('Origin',(-0.65,-1.6,10.1));
#36150=CARTESIAN_POINT('',(-0.745,-1.6,10.4));
#36151=CARTESIAN_POINT('',(-0.745,-1.6,10.25));
#36152=CARTESIAN_POINT('Origin',(-0.65,-1.6,10.4));
#36153=CARTESIAN_POINT('Origin',(0.65,-1.6,10.25));
#36154=CARTESIAN_POINT('',(0.555,-1.6,10.1));
#36155=CARTESIAN_POINT('Origin',(0.65,-1.6,10.1));
#36156=CARTESIAN_POINT('',(0.555,-1.6,10.4));
#36157=CARTESIAN_POINT('',(0.555,-1.6,10.25));
#36158=CARTESIAN_POINT('Origin',(0.65,-1.6,10.4));
#36159=CARTESIAN_POINT('Origin',(0.,-1.6,10.25));
#36160=CARTESIAN_POINT('',(-0.305,-1.6,10.1));
#36161=CARTESIAN_POINT('Origin',(0.,-1.6,10.1));
#36162=CARTESIAN_POINT('',(-0.305,-1.6,10.4));
#36163=CARTESIAN_POINT('',(-0.305,-1.6,10.25));
#36164=CARTESIAN_POINT('Origin',(0.,-1.6,10.4));
#36165=CARTESIAN_POINT('Origin',(0.,0.,10.115));
#36166=CARTESIAN_POINT('',(0.83,-1.0164568432923E-16,10.1));
#36167=CARTESIAN_POINT('Origin',(0.,0.,10.1));
#36168=CARTESIAN_POINT('',(0.8,9.79717439317883E-17,10.13));
#36169=CARTESIAN_POINT('',(0.815,-9.98087141305093E-17,10.115));
#36170=CARTESIAN_POINT('',(-0.8,-9.79717439317883E-17,10.13));
#36171=CARTESIAN_POINT('Origin',(0.,0.,10.13));
#36172=CARTESIAN_POINT('Origin',(0.,0.,10.13));
#36173=CARTESIAN_POINT('Origin',(0.,0.,10.25));
#36174=CARTESIAN_POINT('',(0.8,-9.79717439317883E-17,10.37));
#36175=CARTESIAN_POINT('',(-0.8,-9.79717439317883E-17,10.37));
#36176=CARTESIAN_POINT('Origin',(0.,0.,10.37));
#36177=CARTESIAN_POINT('Origin',(0.,0.,10.37));
#36178=CARTESIAN_POINT('',(-0.8,-9.79717439317883E-17,10.25));
#36179=CARTESIAN_POINT('Origin',(4.,0.,10.1));
#36180=CARTESIAN_POINT('',(3.97,4.86184779261499E-16,10.1));
#36181=CARTESIAN_POINT('Origin',(0.,0.,10.1));
#36182=CARTESIAN_POINT('Origin',(0.,0.,10.385));
#36183=CARTESIAN_POINT('',(0.83,1.0164568432923E-16,10.4));
#36184=CARTESIAN_POINT('',(0.815,-9.98087141305093E-17,10.385));
#36185=CARTESIAN_POINT('Origin',(0.,0.,10.4));
#36186=CARTESIAN_POINT('Origin',(0.8,0.,10.4));
#36187=CARTESIAN_POINT('',(3.97,-4.86184779261499E-16,10.4));
#36188=CARTESIAN_POINT('Origin',(0.,0.,10.4));
#36189=CARTESIAN_POINT('Origin',(0.,0.,10.385));
#36190=CARTESIAN_POINT('',(4.,4.89858719658941E-16,10.37));
#36191=CARTESIAN_POINT('',(3.985,4.8802174946022E-16,10.385));
#36192=CARTESIAN_POINT('',(-4.,-4.89858719658941E-16,10.37));
#36193=CARTESIAN_POINT('Origin',(0.,0.,10.37));
#36194=CARTESIAN_POINT('Origin',(0.,0.,10.37));
#36195=CARTESIAN_POINT('Origin',(0.,0.,10.25));
#36196=CARTESIAN_POINT('',(-4.,-4.89858719658941E-16,10.13));
#36197=CARTESIAN_POINT('',(-4.,-4.89858719658941E-16,10.25));
#36198=CARTESIAN_POINT('',(4.,-4.89858719658941E-16,10.13));
#36199=CARTESIAN_POINT('Origin',(0.,0.,10.13));
#36200=CARTESIAN_POINT('Origin',(0.,0.,10.13));
#36201=CARTESIAN_POINT('Origin',(0.,0.,10.115));
#36202=CARTESIAN_POINT('',(3.985,4.8802174946022E-16,10.115));
#36203=CARTESIAN_POINT('',(0.,0.,0.));
#36204=CARTESIAN_POINT('Origin',(-0.65,0.,-0.325536576308671));
#36205=CARTESIAN_POINT('',(-0.65,0.,-0.351073152617343));
#36206=CARTESIAN_POINT('',(-0.735,-1.04094977927525E-17,-0.3));
#36207=CARTESIAN_POINT('',(-0.6925,-5.20474889637625E-18,-0.325536576308671));
#36208=CARTESIAN_POINT('Origin',(-0.65,0.,-0.3));
#36209=CARTESIAN_POINT('Origin',(-0.65,0.,-0.125));
#36210=CARTESIAN_POINT('',(-0.735,1.04094977927525E-17,0.));
#36211=CARTESIAN_POINT('',(-0.735,-1.04094977927525E-17,-0.125));
#36212=CARTESIAN_POINT('Origin',(-0.65,0.,0.));
#36213=CARTESIAN_POINT('Origin',(0.65,0.,-0.325536576308671));
#36214=CARTESIAN_POINT('',(0.65,0.,-0.351073152617343));
#36215=CARTESIAN_POINT('',(0.565,-1.04094977927525E-17,-0.3));
#36216=CARTESIAN_POINT('',(0.6075,-5.20474889637625E-18,-0.325536576308671));
#36217=CARTESIAN_POINT('Origin',(0.65,0.,-0.3));
#36218=CARTESIAN_POINT('Origin',(0.65,0.,-0.125));
#36219=CARTESIAN_POINT('',(0.565,1.04094977927525E-17,0.));
#36220=CARTESIAN_POINT('',(0.565,-1.04094977927525E-17,-0.125));
#36221=CARTESIAN_POINT('Origin',(0.65,0.,0.));
#36222=CARTESIAN_POINT('Origin',(0.,0.32,-2.92));
#36223=CARTESIAN_POINT('',(-0.14,0.32,-3.52));
#36224=CARTESIAN_POINT('Origin',(0.,0.32,-3.52));
#36225=CARTESIAN_POINT('',(-0.14,0.32,-2.92));
#36226=CARTESIAN_POINT('',(-0.14,0.32,-2.92));
#36227=CARTESIAN_POINT('Origin',(0.,0.32,-2.92));
#36228=CARTESIAN_POINT('Origin',(0.,0.32,-3.52));
#36229=CARTESIAN_POINT('Origin',(0.5,0.,-2.92));
#36230=CARTESIAN_POINT('',(-0.5,-6.12323399573677E-17,-2.92));
#36231=CARTESIAN_POINT('Origin',(0.,0.,-2.92));
#36232=CARTESIAN_POINT('Origin',(0.,0.,-2.9));
#36233=CARTESIAN_POINT('',(-0.54,-6.61309271539571E-17,-2.88));
#36234=CARTESIAN_POINT('Origin',(0.,0.,-2.88));
#36235=CARTESIAN_POINT('',(-0.52,-6.36816335556624E-17,-2.9));
#36236=CARTESIAN_POINT('Origin',(0.,0.,-2.84));
#36237=CARTESIAN_POINT('',(-0.54,-6.61309271539571E-17,-2.8));
#36238=CARTESIAN_POINT('Origin',(0.,0.,-2.8));
#36239=CARTESIAN_POINT('',(-0.54,-6.61309271539571E-17,-2.84));
#36240=CARTESIAN_POINT('Origin',(0.,0.,-1.47));
#36241=CARTESIAN_POINT('',(-0.78,-9.55224503334935E-17,-1.5));
#36242=CARTESIAN_POINT('Origin',(0.,0.,-1.5));
#36243=CARTESIAN_POINT('',(-0.78,-9.55224503334935E-17,-1.44));
#36244=CARTESIAN_POINT('',(-0.78,-9.55224503334935E-17,-1.47));
#36245=CARTESIAN_POINT('Origin',(0.,0.,-1.44));
#36246=CARTESIAN_POINT('Origin',(0.82,0.,-1.5));
#36247=CARTESIAN_POINT('',(-0.8,9.79717439317883E-17,-1.5));
#36248=CARTESIAN_POINT('Origin',(0.,0.,-1.5));
#36249=CARTESIAN_POINT('Origin',(0.78,0.,-1.44));
#36250=CARTESIAN_POINT('',(-0.8,-9.79717439317883E-17,-1.44));
#36251=CARTESIAN_POINT('Origin',(0.,0.,-1.44));
#36252=CARTESIAN_POINT('Origin',(0.,0.,-1.4));
#36253=CARTESIAN_POINT('',(-0.8,-9.79717439317883E-17,-0.04));
#36254=CARTESIAN_POINT('Origin',(0.,0.,-0.04));
#36255=CARTESIAN_POINT('',(-0.8,-9.79717439317883E-17,-1.4));
#36256=CARTESIAN_POINT('Origin',(0.76,0.,-2.8));
#36257=CARTESIAN_POINT('',(-0.76,-9.30731567351988E-17,-2.8));
#36258=CARTESIAN_POINT('Origin',(0.,0.,-2.8));
#36259=CARTESIAN_POINT('Origin',(0.,0.,-2.78));
#36260=CARTESIAN_POINT('',(-0.8,-9.79717439317883E-17,-2.76));
#36261=CARTESIAN_POINT('Origin',(0.,0.,-2.76));
#36262=CARTESIAN_POINT('',(-0.78,-9.55224503334935E-17,-2.78));
#36263=CARTESIAN_POINT('Origin',(0.,0.,-1.4));
#36264=CARTESIAN_POINT('',(-0.8,-9.79717439317883E-17,-1.4));
#36265=CARTESIAN_POINT('Origin',(0.,0.,-0.02));
#36266=CARTESIAN_POINT('',(-0.76,-9.30731567351988E-17,-1.04083408558608E-17));
#36267=CARTESIAN_POINT('Origin',(0.,0.,0.));
#36268=CARTESIAN_POINT('',(-0.78,-9.55224503334935E-17,-0.02));
#36269=CARTESIAN_POINT('Origin',(0.3,0.,0.));
#36270=CARTESIAN_POINT('',(-0.3,-3.67394039744206E-17,-6.93889390390723E-18));
#36271=CARTESIAN_POINT('Origin',(0.,0.,0.));
#36272=CARTESIAN_POINT('Origin',(0.,0.,0.04));
#36273=CARTESIAN_POINT('',(-0.3,-3.67394039744206E-17,0.08));
#36274=CARTESIAN_POINT('Origin',(0.,0.,0.08));
#36275=CARTESIAN_POINT('',(-0.3,-3.67394039744206E-17,0.04));
#36276=CARTESIAN_POINT('Origin',(0.1,0.,0.08));
#36277=CARTESIAN_POINT('',(-0.1,-1.22464679914735E-17,0.08));
#36278=CARTESIAN_POINT('Origin',(0.,0.,0.08));
#36279=CARTESIAN_POINT('Origin',(0.,0.,0.51));
#36280=CARTESIAN_POINT('',(-0.1,-1.22464679914735E-17,0.94));
#36281=CARTESIAN_POINT('Origin',(0.,0.,0.94));
#36282=CARTESIAN_POINT('',(-0.1,-1.22464679914735E-17,0.51));
#36283=CARTESIAN_POINT('Origin',(0.,0.,0.95));
#36284=CARTESIAN_POINT('',(-0.08,-9.79717439317882E-18,0.96));
#36285=CARTESIAN_POINT('Origin',(0.,0.,0.96));
#36286=CARTESIAN_POINT('',(-0.09,-1.10218211923262E-17,0.95));
#36287=CARTESIAN_POINT('Origin',(0.,0.,0.96));
#36288=CARTESIAN_POINT('',(0.,0.,0.));
#36289=CARTESIAN_POINT('Origin',(0.,0.,11.045));
#36290=CARTESIAN_POINT('',(0.17,-2.0818995585505E-17,11.06));
#36291=CARTESIAN_POINT('Origin',(0.,0.,11.06));
#36292=CARTESIAN_POINT('',(0.2,2.44929359829471E-17,11.03));
#36293=CARTESIAN_POINT('',(0.185,2.2655965784226E-17,11.045));
#36294=CARTESIAN_POINT('',(-0.2,-2.44929359829471E-17,11.03));
#36295=CARTESIAN_POINT('Origin',(0.,0.,11.03));
#36296=CARTESIAN_POINT('Origin',(0.,0.,11.03));
#36297=CARTESIAN_POINT('Origin',(0.1,0.,11.06));
#36298=CARTESIAN_POINT('',(0.13,1.59204083889156E-17,11.06));
#36299=CARTESIAN_POINT('Origin',(0.,0.,11.06));
#36300=CARTESIAN_POINT('Origin',(0.,0.,10.985));
#36301=CARTESIAN_POINT('',(-0.2,-2.44929359829471E-17,10.91));
#36302=CARTESIAN_POINT('',(-0.2,-2.44929359829471E-17,10.985));
#36303=CARTESIAN_POINT('Origin',(0.,0.,10.91));
#36304=CARTESIAN_POINT('Origin',(0.,0.,11.045));
#36305=CARTESIAN_POINT('',(0.1,-1.22464679914735E-17,11.03));
#36306=CARTESIAN_POINT('',(-0.1,-1.22464679914735E-17,11.03));
#36307=CARTESIAN_POINT('Origin',(0.,0.,11.03));
#36308=CARTESIAN_POINT('Origin',(0.,0.,11.03));
#36309=CARTESIAN_POINT('',(0.115,-1.40834381901946E-17,11.045));
#36310=CARTESIAN_POINT('Origin',(0.,0.,10.755));
#36311=CARTESIAN_POINT('',(-0.1,-1.22464679914735E-17,10.48));
#36312=CARTESIAN_POINT('',(-0.1,-1.22464679914735E-17,10.755));
#36313=CARTESIAN_POINT('',(0.0547465096656995,0.0836828517644056,10.48));
#36314=CARTESIAN_POINT('Origin',(0.,0.,10.48));
#36315=CARTESIAN_POINT('',(0.0400022951850117,0.0916331167321948,10.4916905977975));
#36316=CARTESIAN_POINT('Ctrl Pts',(0.0400026971257908,0.091629894956361,
10.4916928986414));
#36317=CARTESIAN_POINT('Ctrl Pts',(0.0449750733872993,0.0894586747527078,
10.4877839912521));
#36318=CARTESIAN_POINT('Ctrl Pts',(0.0499491910902487,0.0868191962733323,
10.4838139809416));
#36319=CARTESIAN_POINT('Ctrl Pts',(0.0547498300911773,0.0836911968368012,
10.4799973371599));
#36320=CARTESIAN_POINT('',(0.0400031709030036,0.091629687702094,10.6683074724692));
#36321=CARTESIAN_POINT('',(0.04,0.0916515138991168,10.755));
#36322=CARTESIAN_POINT('',(0.0400031709030041,-0.0916296877020945,10.6683074724692));
#36323=CARTESIAN_POINT('Ctrl Pts',(0.0400031709030041,-0.0916296877020945,
10.6683074724692));
#36324=CARTESIAN_POINT('Ctrl Pts',(0.0462164496289358,-0.0889165823855752,
10.6731918882274));
#36325=CARTESIAN_POINT('Ctrl Pts',(0.0524198696107662,-0.0854817956373576,
10.6781585108626));
#36326=CARTESIAN_POINT('Ctrl Pts',(0.0583027869865068,-0.0812628967806547,
10.6828213320007));
#36327=CARTESIAN_POINT('Ctrl Pts',(0.0583051566221747,-0.0812611974106702,
10.6828232101823));
#36328=CARTESIAN_POINT('Ctrl Pts',(0.058307526202546,-0.0812594979157138,
10.6828250883107));
#36329=CARTESIAN_POINT('Ctrl Pts',(0.0583098957275982,-0.0812577982957833,
10.682826966386));
#36330=CARTESIAN_POINT('Ctrl Pts',(0.0685201251108097,-0.0739341747962435,
10.6909195499127));
#36331=CARTESIAN_POINT('Ctrl Pts',(0.0791018243371258,-0.0632694863644097,
10.6991954559706));
#36332=CARTESIAN_POINT('Ctrl Pts',(0.0870673985112314,-0.0492439898634108,
10.7052699386598));
#36333=CARTESIAN_POINT('Ctrl Pts',(0.0870677359705705,-0.0492433956771441,
10.7052701960036));
#36334=CARTESIAN_POINT('Ctrl Pts',(0.0870680734252534,-0.049242801484857,
10.7052704533434));
#36335=CARTESIAN_POINT('Ctrl Pts',(0.0870684108752795,-0.0492422072865498,
10.7052707106792));
#36336=CARTESIAN_POINT('Ctrl Pts',(0.0910516748715721,-0.0422282836214033,
10.7083083052616));
#36337=CARTESIAN_POINT('Ctrl Pts',(0.0942888586636921,-0.0343297647086917,
10.7107378284348));
#36338=CARTESIAN_POINT('Ctrl Pts',(0.0965327211088765,-0.0259716063509559,
10.7124125068353));
#36339=CARTESIAN_POINT('Ctrl Pts',(0.0982475846719583,-0.01958391478238,
10.7136923736004));
#36340=CARTESIAN_POINT('Ctrl Pts',(0.0993781637156952,-0.0129130123107152,
10.7145346369017));
#36341=CARTESIAN_POINT('Ctrl Pts',(0.099813360278901,-0.00620869762228023,
10.7148586788687));
#36342=CARTESIAN_POINT('Ctrl Pts',(0.09994765739052,-0.00413981616924315,
10.7149586748335));
#36343=CARTESIAN_POINT('Ctrl Pts',(0.100016017514125,-0.00206780492919306,
10.7150095423241));
#36344=CARTESIAN_POINT('Ctrl Pts',(0.100016017514125,-4.36695016576629E-17,
10.7150095423241));
#36345=CARTESIAN_POINT('Ctrl Pts',(0.100016017514124,0.00670082615866859,
10.7150095423241));
#36346=CARTESIAN_POINT('Ctrl Pts',(0.0992947386787322,0.0134460393231833,
10.7144728477617));
#36347=CARTESIAN_POINT('Ctrl Pts',(0.0979505340509732,0.0199846250780982,
10.713470323343));
#36348=CARTESIAN_POINT('Ctrl Pts',(0.0975357265497413,0.0220023643140571,
10.7131609547838));
#36349=CARTESIAN_POINT('Ctrl Pts',(0.0970619100841739,0.0240004314840473,
10.7128074603445));
#36350=CARTESIAN_POINT('Ctrl Pts',(0.0965327211088716,0.0259716063509535,
10.7124125068353));
#36351=CARTESIAN_POINT('Ctrl Pts',(0.0942888586636877,0.0343297647086844,
10.7107378284348));
#36352=CARTESIAN_POINT('Ctrl Pts',(0.0910516748715695,0.0422282836213917,
10.7083083052616));
#36353=CARTESIAN_POINT('Ctrl Pts',(0.0870684108752762,0.0492422072865391,
10.7052707106792));
#36354=CARTESIAN_POINT('Ctrl Pts',(0.0870680734252483,0.0492428014848496,
10.7052704533434));
#36355=CARTESIAN_POINT('Ctrl Pts',(0.0870677359705637,0.0492433956771398,
10.7052701960036));
#36356=CARTESIAN_POINT('Ctrl Pts',(0.0870673985112227,0.0492439898634097,
10.7052699386598));
#36357=CARTESIAN_POINT('Ctrl Pts',(0.0791018243371071,0.063269486364422,
10.6991954559706));
#36358=CARTESIAN_POINT('Ctrl Pts',(0.0685201251108037,0.0739341747962399,
10.6909195499127));
#36359=CARTESIAN_POINT('Ctrl Pts',(0.0583098957275852,0.0812577982957855,
10.682826966386));
#36360=CARTESIAN_POINT('Ctrl Pts',(0.0583075262025378,0.0812594979157126,
10.6828250883107));
#36361=CARTESIAN_POINT('Ctrl Pts',(0.0583051566221713,0.0812611974106655,
10.6828232101823));
#36362=CARTESIAN_POINT('Ctrl Pts',(0.0583027869865083,0.0812628967806466,
10.6828213320007));
#36363=CARTESIAN_POINT('Ctrl Pts',(0.0524198696107668,0.0854817956373522,
10.6781585108626));
#36364=CARTESIAN_POINT('Ctrl Pts',(0.0462164496289357,0.0889165823855736,
10.6731918882274));
#36365=CARTESIAN_POINT('Ctrl Pts',(0.0400031709030036,0.091629687702094,
10.6683074724692));
#36366=CARTESIAN_POINT('',(0.0400026975908353,-0.0916329430552092,10.4916902797062));
#36367=CARTESIAN_POINT('',(0.04,-0.0916515138991168,10.755));
#36368=CARTESIAN_POINT('',(0.0547465096656977,-0.0836828517644066,10.48));
#36369=CARTESIAN_POINT('Ctrl Pts',(0.0547498564515704,-0.0836911796608913,
10.4799973162027));
#36370=CARTESIAN_POINT('Ctrl Pts',(0.0499493615997624,-0.0868190873748065,
10.4838138453251));
#36371=CARTESIAN_POINT('Ctrl Pts',(0.0449753980973141,-0.0894585033025012,
10.4877837321994));
#36372=CARTESIAN_POINT('Ctrl Pts',(0.0400031703736387,-0.0916296883082219,
10.4916925266094));
#36373=CARTESIAN_POINT('Origin',(0.,0.,10.48));
#36374=CARTESIAN_POINT('Origin',(0.,0.,10.465));
#36375=CARTESIAN_POINT('',(0.13,-1.59204083889156E-17,10.45));
#36376=CARTESIAN_POINT('Origin',(0.,0.,10.45));
#36377=CARTESIAN_POINT('',(0.1175,-5.20790795218413E-18,10.4625));
#36378=CARTESIAN_POINT('',(0.115,-1.40834381901946E-17,10.465));
#36379=CARTESIAN_POINT('Ctrl Pts',(0.1175,3.97378398561307E-18,10.4625));
#36380=CARTESIAN_POINT('Ctrl Pts',(0.1175,0.00168116624611717,10.4625));
#36381=CARTESIAN_POINT('Ctrl Pts',(0.117445299801582,0.00336180897409119,
10.4625186262133));
#36382=CARTESIAN_POINT('Ctrl Pts',(0.11712796129555,0.00823395361238692,
10.4626265875713));
#36383=CARTESIAN_POINT('Ctrl Pts',(0.116722984118053,0.0114065443838321,
10.4627643564121));
#36384=CARTESIAN_POINT('Ctrl Pts',(0.114747805849752,0.0217932663755633,
10.4634333117491));
#36385=CARTESIAN_POINT('Ctrl Pts',(0.112368157615186,0.0287533951010713,
10.4642376426297));
#36386=CARTESIAN_POINT('Ctrl Pts',(0.10440367232782,0.0448544941116708,
10.4668577183297));
#36387=CARTESIAN_POINT('Ctrl Pts',(0.0979725906862171,0.0533246487475542,
10.468932263714));
#36388=CARTESIAN_POINT('Ctrl Pts',(0.0801403078141064,0.0704639960442362,
10.4741919330898));
#36389=CARTESIAN_POINT('Ctrl Pts',(0.0679192198366975,0.0780725887634243,
10.4774832290237));
#36390=CARTESIAN_POINT('Ctrl Pts',(0.0547465096656995,0.0836828517644056,
10.48));
#36391=CARTESIAN_POINT('Ctrl Pts',(0.0547465096656977,-0.0836828517644066,
10.48));
#36392=CARTESIAN_POINT('Ctrl Pts',(0.061953028387731,-0.0806135923009201,
10.4786231263784));
#36393=CARTESIAN_POINT('Ctrl Pts',(0.0688691022940564,-0.0769503000424395,
10.4770113369889));
#36394=CARTESIAN_POINT('Ctrl Pts',(0.0826170742067669,-0.067802259687565,
10.4734642639149));
#36395=CARTESIAN_POINT('Ctrl Pts',(0.0893317161066329,-0.062146954826949,
10.4715149522659));
#36396=CARTESIAN_POINT('Ctrl Pts',(0.102911979968346,-0.0471215719111262,
10.4673741996323));
#36397=CARTESIAN_POINT('Ctrl Pts',(0.109049928744403,-0.0372655563958094,
10.4653399473256));
#36398=CARTESIAN_POINT('Ctrl Pts',(0.11469710309367,-0.0213425122859003,
10.4634512615441));
#36399=CARTESIAN_POINT('Ctrl Pts',(0.115970092871191,-0.0162235405860467,
10.4630196858142));
#36400=CARTESIAN_POINT('Ctrl Pts',(0.117120046050328,-0.00817532652652597,
10.4626293532478));
#36401=CARTESIAN_POINT('Ctrl Pts',(0.117368256214482,-0.00533987258579196,
10.4625448416866));
#36402=CARTESIAN_POINT('Ctrl Pts',(0.117486627839774,-0.0016625527838929,
10.4625045523855));
#36403=CARTESIAN_POINT('Ctrl Pts',(0.1175,-0.000831212403074635,10.4625));
#36404=CARTESIAN_POINT('Ctrl Pts',(0.1175,3.97378398561307E-18,10.4625));
#36405=CARTESIAN_POINT('Ctrl Pts',(0.00894444267269597,-0.0995991814488194,
10.5141610714912));
#36406=CARTESIAN_POINT('Ctrl Pts',(0.0132379567575632,-0.0992136050812441,
10.5116620905429));
#36407=CARTESIAN_POINT('Ctrl Pts',(0.0183531525220914,-0.0984395027524004,
10.5081248887167));
#36408=CARTESIAN_POINT('Ctrl Pts',(0.034707695840997,-0.0945110281336789,
10.4960700069752));
#36409=CARTESIAN_POINT('Ctrl Pts',(0.0471226257755256,-0.0892804815421576,
10.4860357640661));
#36410=CARTESIAN_POINT('Ctrl Pts',(0.0685122634921431,-0.0739398417001646,
10.4690867488427));
#36411=CARTESIAN_POINT('Ctrl Pts',(0.0790926322048203,-0.0632798178846318,
10.4608050384725));
#36412=CARTESIAN_POINT('Ctrl Pts',(0.0950417827106649,-0.0352045502384536,
10.4486511121129));
#36413=CARTESIAN_POINT('Ctrl Pts',(0.10499024921961,2.0497699264001E-14,
10.4413298003685));
#36414=CARTESIAN_POINT('Ctrl Pts',(0.0950417827106623,0.0352045502384679,
10.4486511121129));
#36415=CARTESIAN_POINT('Ctrl Pts',(0.0790926322048192,0.063279817884641,
10.4608050384725));
#36416=CARTESIAN_POINT('Ctrl Pts',(0.0685122634921198,0.0739398417001872,
10.4690867488427));
#36417=CARTESIAN_POINT('Ctrl Pts',(0.0471226257755508,0.0892804815421436,
10.4860357640661));
#36418=CARTESIAN_POINT('Ctrl Pts',(0.0347076958409767,0.0945110281336857,
10.4960700069752));
#36419=CARTESIAN_POINT('Ctrl Pts',(0.0183531525220986,0.0984395027523984,
10.5081248887167));
#36420=CARTESIAN_POINT('Ctrl Pts',(0.0132379567575634,0.0992136050812441,
10.5116620905429));
#36421=CARTESIAN_POINT('Ctrl Pts',(0.00894444267269637,0.0995991814488194,
10.5141610714912));
#36422=CARTESIAN_POINT('Ctrl Pts',(0.0192962951151297,-0.10101340050352,
10.5309232968739));
#36423=CARTESIAN_POINT('Ctrl Pts',(0.0246829710160883,-0.100510889482336,
10.5276355936907));
#36424=CARTESIAN_POINT('Ctrl Pts',(0.0302700618807701,-0.0996151370866697,
10.5235433339832));
#36425=CARTESIAN_POINT('Ctrl Pts',(0.047446855001171,-0.095352727284558,
10.5101326862265));
#36426=CARTESIAN_POINT('Ctrl Pts',(0.0596224836125303,-0.0899496685517302,
10.4994713083419));
#36427=CARTESIAN_POINT('Ctrl Pts',(0.0803741273880472,-0.0743507192264208,
10.4812582586986));
#36428=CARTESIAN_POINT('Ctrl Pts',(0.0904178622326513,-0.0635857683883024,
10.4723242438985));
#36429=CARTESIAN_POINT('Ctrl Pts',(0.105408335734682,-0.0353360781276079,
10.4590400838768));
#36430=CARTESIAN_POINT('Ctrl Pts',(0.1146188438952,2.05947277554036E-14,
10.4509376050958));
#36431=CARTESIAN_POINT('Ctrl Pts',(0.10540833573468,0.035336078127622,10.4590400838768));
#36432=CARTESIAN_POINT('Ctrl Pts',(0.0904178622326502,0.0635857683883118,
10.4723242438985));
#36433=CARTESIAN_POINT('Ctrl Pts',(0.080374127388024,0.0743507192264434,
10.4812582586986));
#36434=CARTESIAN_POINT('Ctrl Pts',(0.0596224836125554,0.0899496685517165,
10.4994713083419));
#36435=CARTESIAN_POINT('Ctrl Pts',(0.0474468550011507,0.0953527272845648,
10.5101326862265));
#36436=CARTESIAN_POINT('Ctrl Pts',(0.0302700618807774,0.0996151370866677,
10.5235433339832));
#36437=CARTESIAN_POINT('Ctrl Pts',(0.0246829710160885,0.100510889482336,
10.5276355936907));
#36438=CARTESIAN_POINT('Ctrl Pts',(0.0192962951151303,0.10101340050352,
10.5309232968739));
#36439=CARTESIAN_POINT('Ctrl Pts',(0.0296481475575634,-0.102427619558221,
10.5476855222567));
#36440=CARTESIAN_POINT('Ctrl Pts',(0.0362443713099572,-0.101809611530983,
10.5435670582213));
#36441=CARTESIAN_POINT('Ctrl Pts',(0.0421748087255316,-0.100789286669114,
10.5389748496896));
#36442=CARTESIAN_POINT('Ctrl Pts',(0.0602984616063804,-0.0961969927156803,
10.524134695165));
#36443=CARTESIAN_POINT('Ctrl Pts',(0.0721769673050456,-0.0906177935398247,
10.5128816249181));
#36444=CARTESIAN_POINT('Ctrl Pts',(0.0922682177891075,-0.0747621107130237,
10.4934215201235));
#36445=CARTESIAN_POINT('Ctrl Pts',(0.101781264257295,-0.0638900076838062,
10.4838094232667));
#36446=CARTESIAN_POINT('Ctrl Pts',(0.115824116633652,-0.0354675295166492,
10.4694291815536));
#36447=CARTESIAN_POINT('Ctrl Pts',(0.124291726247609,8.66907190709113E-15,
10.4605209321096));
#36448=CARTESIAN_POINT('Ctrl Pts',(0.115824116633656,0.0354675295166414,
10.4694291815535));
#36449=CARTESIAN_POINT('Ctrl Pts',(0.101781264257307,0.06389000768379,10.4838094232667));
#36450=CARTESIAN_POINT('Ctrl Pts',(0.0922682177891217,0.0747621107130131,
10.4934215201235));
#36451=CARTESIAN_POINT('Ctrl Pts',(0.0721769673050495,0.0906177935398222,
10.5128816249181));
#36452=CARTESIAN_POINT('Ctrl Pts',(0.0602984616064044,0.0961969927156732,
10.524134695165));
#36453=CARTESIAN_POINT('Ctrl Pts',(0.0421748087255233,0.100789286669116,
10.5389748496896));
#36454=CARTESIAN_POINT('Ctrl Pts',(0.0362443713099577,0.101809611530983,
10.5435670582213));
#36455=CARTESIAN_POINT('Ctrl Pts',(0.0296481475575642,0.102427619558221,
10.5476855222567));
#36456=CARTESIAN_POINT('Ctrl Pts',(0.0399999999999971,-0.103841838612921,
10.5644477476394));
#36457=CARTESIAN_POINT('Ctrl Pts',(0.0476893855684823,-0.103106895932074,
10.5595405613692));
#36458=CARTESIAN_POINT('Ctrl Pts',(0.0540917180842104,-0.101964921003383,
10.5543932949561));
#36459=CARTESIAN_POINT('Ctrl Pts',(0.0730376207665544,-0.0970386918665594,
10.5381973744163));
#36460=CARTESIAN_POINT('Ctrl Pts',(0.0846768251420503,-0.0912869805493973,
10.5263171691939));
#36461=CARTESIAN_POINT('Ctrl Pts',(0.104130081685012,-0.0751729882392799,
10.5055930299794));
#36462=CARTESIAN_POINT('Ctrl Pts',(0.113106494285126,-0.0641959581874768,
10.4953286286927));
#36463=CARTESIAN_POINT('Ctrl Pts',(0.12619066965767,-0.0355990574058035,
10.4798181533174));
#36464=CARTESIAN_POINT('Ctrl Pts',(0.133920320923199,8.76610039849372E-15,
10.4701287368369));
#36465=CARTESIAN_POINT('Ctrl Pts',(0.126190669657674,0.0355990574057956,
10.4798181533174));
#36466=CARTESIAN_POINT('Ctrl Pts',(0.113106494285138,0.0641959581874607,
10.4953286286927));
#36467=CARTESIAN_POINT('Ctrl Pts',(0.104130081685026,0.0751729882392693,
10.5055930299794));
#36468=CARTESIAN_POINT('Ctrl Pts',(0.0846768251420541,0.0912869805493951,
10.5263171691939));
#36469=CARTESIAN_POINT('Ctrl Pts',(0.0730376207665783,0.0970386918665523,
10.5381973744163));
#36470=CARTESIAN_POINT('Ctrl Pts',(0.0540917180842021,0.101964921003385,
10.5543932949561));
#36471=CARTESIAN_POINT('Ctrl Pts',(0.0476893855684828,0.103106895932074,
10.5595405613692));
#36472=CARTESIAN_POINT('Ctrl Pts',(0.0399999999999982,0.103841838612921,
10.5644477476394));
#36473=CARTESIAN_POINT('',(0.0399999999999998,-0.103841838612921,10.5644477476394));
#36474=CARTESIAN_POINT('Ctrl Pts',(0.04,-0.103841838612921,10.5644477476394));
#36475=CARTESIAN_POINT('Ctrl Pts',(0.04,-0.102606877508547,10.5524412635046));
#36476=CARTESIAN_POINT('Ctrl Pts',(0.0399999999999991,-0.101164192447474,
10.5403304050204));
#36477=CARTESIAN_POINT('Ctrl Pts',(0.0399999999999991,-0.0972792884300837,
10.5159352723978));
#36478=CARTESIAN_POINT('Ctrl Pts',(0.0399999999999998,-0.0948285669211716,
10.5037338000625));
#36479=CARTESIAN_POINT('Ctrl Pts',(0.0399999999999998,-0.0916515138991173,
10.4916774593885));
#36480=CARTESIAN_POINT('',(0.0400000000000002,0.103841838612921,10.5644477476394));
#36481=CARTESIAN_POINT('Ctrl Pts',(0.0399999999999971,-0.103841838612921,
10.5644477476394));
#36482=CARTESIAN_POINT('Ctrl Pts',(0.0476893855684823,-0.103106895932074,
10.5595405613692));
#36483=CARTESIAN_POINT('Ctrl Pts',(0.0540917180842104,-0.101964921003383,
10.5543932949561));
#36484=CARTESIAN_POINT('Ctrl Pts',(0.0730376207665544,-0.0970386918665594,
10.5381973744163));
#36485=CARTESIAN_POINT('Ctrl Pts',(0.0846768251420503,-0.0912869805493973,
10.5263171691939));
#36486=CARTESIAN_POINT('Ctrl Pts',(0.104130081685012,-0.0751729882392799,
10.5055930299794));
#36487=CARTESIAN_POINT('Ctrl Pts',(0.113106494285126,-0.0641959581874768,
10.4953286286927));
#36488=CARTESIAN_POINT('Ctrl Pts',(0.12619066965767,-0.0355990574058035,
10.4798181533174));
#36489=CARTESIAN_POINT('Ctrl Pts',(0.133920320923199,8.76610039849372E-15,
10.4701287368369));
#36490=CARTESIAN_POINT('Ctrl Pts',(0.126190669657674,0.0355990574057956,
10.4798181533174));
#36491=CARTESIAN_POINT('Ctrl Pts',(0.113106494285138,0.0641959581874607,
10.4953286286927));
#36492=CARTESIAN_POINT('Ctrl Pts',(0.104130081685026,0.0751729882392693,
10.5055930299794));
#36493=CARTESIAN_POINT('Ctrl Pts',(0.0846768251420541,0.0912869805493951,
10.5263171691939));
#36494=CARTESIAN_POINT('Ctrl Pts',(0.0730376207665783,0.0970386918665523,
10.5381973744163));
#36495=CARTESIAN_POINT('Ctrl Pts',(0.0540917180842021,0.101964921003385,
10.5543932949561));
#36496=CARTESIAN_POINT('Ctrl Pts',(0.0476893855684828,0.103106895932074,
10.5595405613692));
#36497=CARTESIAN_POINT('Ctrl Pts',(0.0399999999999982,0.103841838612921,
10.5644477476394));
#36498=CARTESIAN_POINT('Ctrl Pts',(0.04,0.0916515138991168,10.4916774593885));
#36499=CARTESIAN_POINT('Ctrl Pts',(0.04,0.0935744633639231,10.4989747042521));
#36500=CARTESIAN_POINT('Ctrl Pts',(0.0399999999895264,0.095234686169019,
10.5063427163767));
#36501=CARTESIAN_POINT('Ctrl Pts',(0.0399999999895264,0.0999665537033885,
10.5306029708398));
#36502=CARTESIAN_POINT('Ctrl Pts',(0.0399999999999997,0.102095101447083,
10.5474656969538));
#36503=CARTESIAN_POINT('Ctrl Pts',(0.0399999999999997,0.103841838612921,
10.5644477476394));
#36504=CARTESIAN_POINT('Origin',(0.4,0.,10.45));
#36505=CARTESIAN_POINT('',(0.38,4.65365783675994E-17,10.45));
#36506=CARTESIAN_POINT('Origin',(0.,0.,10.45));
#36507=CARTESIAN_POINT('Ctrl Pts',(0.377017787534816,0.133632286077702,
10.58));
#36508=CARTESIAN_POINT('Ctrl Pts',(0.377017787534816,0.133632286077702,
10.5628264326263));
#36509=CARTESIAN_POINT('Ctrl Pts',(0.378257950025364,0.130263180113984,
10.5445759528919));
#36510=CARTESIAN_POINT('Ctrl Pts',(0.382671361121133,0.116705198842861,
10.5112796752359));
#36511=CARTESIAN_POINT('Ctrl Pts',(0.385743385887353,0.106539573413826,
10.4962244912617));
#36512=CARTESIAN_POINT('Ctrl Pts',(0.391476660649127,0.0830605783691531,
10.4724755856568));
#36513=CARTESIAN_POINT('Ctrl Pts',(0.39450689508103,0.068151397938132,10.4621678753065));
#36514=CARTESIAN_POINT('Ctrl Pts',(0.39881767731416,0.0351337186655312,
10.4484079854916));
#36515=CARTESIAN_POINT('Ctrl Pts',(0.400013024202683,0.0170314150408282,
10.4449835136144));
#36516=CARTESIAN_POINT('Ctrl Pts',(0.400012819411827,-0.0170559807859546,
10.4449833066593));
#36517=CARTESIAN_POINT('Ctrl Pts',(0.398817117536753,-0.0351583934957051,
10.4484074138439));
#36518=CARTESIAN_POINT('Ctrl Pts',(0.394505922058271,-0.0681763245922,10.4621668950494));
#36519=CARTESIAN_POINT('Ctrl Pts',(0.391475324666216,-0.0830858365898015,
10.4724741911262));
#36520=CARTESIAN_POINT('Ctrl Pts',(0.385741628020441,-0.106565333574474,
10.4962227929474));
#36521=CARTESIAN_POINT('Ctrl Pts',(0.382669212588462,-0.11673154779195,
10.5112770534905));
#36522=CARTESIAN_POINT('Ctrl Pts',(0.378255397171514,-0.130290214216898,
10.5445743531652));
#36523=CARTESIAN_POINT('Ctrl Pts',(0.377014663925107,-0.133660501471551,
10.5628181917482));
#36524=CARTESIAN_POINT('Ctrl Pts',(0.377014663925106,-0.133660501471554,
10.5971818082517));
#36525=CARTESIAN_POINT('Ctrl Pts',(0.378255397171518,-0.13029021421689,
10.6154256468348));
#36526=CARTESIAN_POINT('Ctrl Pts',(0.382669212588457,-0.116731547791971,
10.6487229465094));
#36527=CARTESIAN_POINT('Ctrl Pts',(0.385741628020435,-0.1065653335745,10.6637772070525));
#36528=CARTESIAN_POINT('Ctrl Pts',(0.39147532466622,-0.0830858365897902,
10.6875258088738));
#36529=CARTESIAN_POINT('Ctrl Pts',(0.394505922058272,-0.0681763245922005,
10.6978331049505));
#36530=CARTESIAN_POINT('Ctrl Pts',(0.398817117536754,-0.0351583934957121,
10.7115925861561));
#36531=CARTESIAN_POINT('Ctrl Pts',(0.400012819411829,-0.0170559807859655,
10.7150166933406));
#36532=CARTESIAN_POINT('Ctrl Pts',(0.400013024202684,0.0170314150408249,
10.7150164863856));
#36533=CARTESIAN_POINT('Ctrl Pts',(0.398817677314164,0.0351337186655008,
10.7115920145084));
#36534=CARTESIAN_POINT('Ctrl Pts',(0.394506895081026,0.068151397938163,
10.6978321246935));
#36535=CARTESIAN_POINT('Ctrl Pts',(0.391476660649127,0.0830605783691558,
10.6875244143432));
#36536=CARTESIAN_POINT('Ctrl Pts',(0.385743385887349,0.106539573413844,
10.6637755087383));
#36537=CARTESIAN_POINT('Ctrl Pts',(0.382671361121131,0.116705198842871,
10.6487203247641));
#36538=CARTESIAN_POINT('Ctrl Pts',(0.378257950025365,0.130263180113984,
10.6154240471081));
#36539=CARTESIAN_POINT('Ctrl Pts',(0.377017787534816,0.133632286077702,
10.5971735673738));
#36540=CARTESIAN_POINT('Ctrl Pts',(0.377017787534816,0.133632286077702,
10.58));
#36541=CARTESIAN_POINT('Ctrl Pts',(0.370002790679512,0.124088190718468,
10.58));
#36542=CARTESIAN_POINT('Ctrl Pts',(0.370006405685752,0.124088635524633,
10.5637880731882));
#36543=CARTESIAN_POINT('Ctrl Pts',(0.371101921434292,0.120800521232035,
10.5465693309555));
#36544=CARTESIAN_POINT('Ctrl Pts',(0.374989826903314,0.107735332893418,
10.5153991323168));
#36545=CARTESIAN_POINT('Ctrl Pts',(0.377685178239063,0.0980280855761085,
10.5014498597172));
#36546=CARTESIAN_POINT('Ctrl Pts',(0.382674879286364,0.0759567643144633,
10.4796760923536));
#36547=CARTESIAN_POINT('Ctrl Pts',(0.385295227322924,0.062110380135337,
10.4703530240385));
#36548=CARTESIAN_POINT('Ctrl Pts',(0.388992255115961,0.0318559581336749,
10.4580194294971));
#36549=CARTESIAN_POINT('Ctrl Pts',(0.390011657552353,0.0154317369722092,
10.4549861845637));
#36550=CARTESIAN_POINT('Ctrl Pts',(0.390011508655186,-0.0154563035124759,
10.4549859776087));
#36551=CARTESIAN_POINT('Ctrl Pts',(0.388991613942717,-0.0318806292414934,
10.4580188578494));
#36552=CARTESIAN_POINT('Ctrl Pts',(0.3852943745433,-0.0621353133809165,
10.4703520437814));
#36553=CARTESIAN_POINT('Ctrl Pts',(0.3826733055481,-0.0759820082990766,
10.479674697823));
#36554=CARTESIAN_POINT('Ctrl Pts',(0.37768379836919,-0.0980538687874221,
10.5014481614029));
#36555=CARTESIAN_POINT('Ctrl Pts',(0.374986900891037,-0.107761633235289,
10.5153965105715));
#36556=CARTESIAN_POINT('Ctrl Pts',(0.371100617680385,-0.120827636867808,
10.5465677312288));
#36557=CARTESIAN_POINT('Ctrl Pts',(0.370000627774456,-0.124116615118387,
10.5637798323102));
#36558=CARTESIAN_POINT('Ctrl Pts',(0.370000627774456,-0.12411661511839,
10.5962201676897));
#36559=CARTESIAN_POINT('Ctrl Pts',(0.371100617680389,-0.1208276368678,10.6134322687712));
#36560=CARTESIAN_POINT('Ctrl Pts',(0.374986900891032,-0.10776163323531,
10.6446034894284));
#36561=CARTESIAN_POINT('Ctrl Pts',(0.377683798369184,-0.098053868787448,
10.658551838597));
#36562=CARTESIAN_POINT('Ctrl Pts',(0.382673305548104,-0.0759820082990655,
10.680325302177));
#36563=CARTESIAN_POINT('Ctrl Pts',(0.385294374543301,-0.062135313380917,
10.6896479562185));
#36564=CARTESIAN_POINT('Ctrl Pts',(0.388991613942718,-0.0318806292415004,
10.7019811421505));
#36565=CARTESIAN_POINT('Ctrl Pts',(0.390011508655187,-0.0154563035124868,
10.7050140223912));
#36566=CARTESIAN_POINT('Ctrl Pts',(0.390011657552354,0.0154317369722058,
10.7050138154362));
#36567=CARTESIAN_POINT('Ctrl Pts',(0.388992255115965,0.0318559581336445,
10.7019805705029));
#36568=CARTESIAN_POINT('Ctrl Pts',(0.38529522732292,0.0621103801353678,
10.6896469759614));
#36569=CARTESIAN_POINT('Ctrl Pts',(0.382674879286364,0.075956764314466,
10.6803239076464));
#36570=CARTESIAN_POINT('Ctrl Pts',(0.377685178239059,0.0980280855761259,
10.6585501402828));
#36571=CARTESIAN_POINT('Ctrl Pts',(0.374989826903312,0.107735332893429,
10.6446008676831));
#36572=CARTESIAN_POINT('Ctrl Pts',(0.371101921434293,0.120800521232036,
10.6134306690445));
#36573=CARTESIAN_POINT('Ctrl Pts',(0.370006405685752,0.124088635524634,
10.5962119268118));
#36574=CARTESIAN_POINT('Ctrl Pts',(0.370002790679512,0.124088190718468,
10.58));
#36575=CARTESIAN_POINT('Ctrl Pts',(0.362987793824209,0.114544095359234,
10.58));
#36576=CARTESIAN_POINT('Ctrl Pts',(0.362984178817969,0.114543650553069,
10.5647559738531));
#36577=CARTESIAN_POINT('Ctrl Pts',(0.363944180231836,0.111328542612427,
10.548562151861));
#36578=CARTESIAN_POINT('Ctrl Pts',(0.367306317957412,0.0987741164193237,
10.5195209482943));
#36579=CARTESIAN_POINT('Ctrl Pts',(0.369622188878733,0.0895126083068797,
10.5066817992144));
#36580=CARTESIAN_POINT('Ctrl Pts',(0.373874212172674,0.0688567722200343,
10.4868715827257));
#36581=CARTESIAN_POINT('Ctrl Pts',(0.376076337898789,0.0560754474460455,
10.4785490202942));
#36582=CARTESIAN_POINT('Ctrl Pts',(0.37917104833718,0.0285718270842341,
10.4676207455255));
#36583=CARTESIAN_POINT('Ctrl Pts',(0.380009038186307,0.013843656528979,
10.4649889870543));
#36584=CARTESIAN_POINT('Ctrl Pts',(0.380008842010176,-0.0138687919798646,
10.4649887173818));
#36585=CARTESIAN_POINT('Ctrl Pts',(0.37917074628356,-0.0285970786710002,
10.4676200006407));
#36586=CARTESIAN_POINT('Ctrl Pts',(0.376075551131707,-0.0561009463910287,
10.4785477429714));
#36587=CARTESIAN_POINT('Ctrl Pts',(0.37387353477512,-0.0688826312592696,
10.4868697655843));
#36588=CARTESIAN_POINT('Ctrl Pts',(0.369620606736793,-0.0895389436561773,
10.506679586228));
#36589=CARTESIAN_POINT('Ctrl Pts',(0.367305623684723,-0.0988011258886412,
10.5195175320322));
#36590=CARTESIAN_POINT('Ctrl Pts',(0.363941182418194,-0.111356123007109,
10.5485600673391));
#36591=CARTESIAN_POINT('Ctrl Pts',(0.362984693436124,-0.114572757005271,
10.5647452355871));
#36592=CARTESIAN_POINT('Ctrl Pts',(0.362984693436123,-0.114572757005271,
10.5952547644128));
#36593=CARTESIAN_POINT('Ctrl Pts',(0.363941182418194,-0.111356123007106,
10.6114399326608));
#36594=CARTESIAN_POINT('Ctrl Pts',(0.367305623684722,-0.0988011258886432,
10.6404824679677));
#36595=CARTESIAN_POINT('Ctrl Pts',(0.369620606736792,-0.0895389436561786,
10.6533204137719));
#36596=CARTESIAN_POINT('Ctrl Pts',(0.37387353477512,-0.0688826312592703,
10.6731302344156));
#36597=CARTESIAN_POINT('Ctrl Pts',(0.376075551131706,-0.0561009463910289,
10.6814522570286));
#36598=CARTESIAN_POINT('Ctrl Pts',(0.37917074628356,-0.028597078670995,
10.6923799993593));
#36599=CARTESIAN_POINT('Ctrl Pts',(0.380008842010175,-0.0138687919798612,
10.6950112826181));
#36600=CARTESIAN_POINT('Ctrl Pts',(0.380009038186307,0.0138436565289819,
10.6950110129456));
#36601=CARTESIAN_POINT('Ctrl Pts',(0.379171048337179,0.0285718270842431,
10.6923792544745));
#36602=CARTESIAN_POINT('Ctrl Pts',(0.37607633789879,0.0560754474460394,
10.6814509797058));
#36603=CARTESIAN_POINT('Ctrl Pts',(0.373874212172674,0.0688567722200364,
10.6731284172743));
#36604=CARTESIAN_POINT('Ctrl Pts',(0.369622188878734,0.0895126083068803,
10.6533182007855));
#36605=CARTESIAN_POINT('Ctrl Pts',(0.367306317957412,0.0987741164193243,
10.6404790517057));
#36606=CARTESIAN_POINT('Ctrl Pts',(0.363944180231836,0.111328542612426,
10.611437848139));
#36607=CARTESIAN_POINT('Ctrl Pts',(0.362984178817969,0.114543650553068,
10.5952440261469));
#36608=CARTESIAN_POINT('Ctrl Pts',(0.362987793824209,0.114544095359234,
10.58));
#36609=CARTESIAN_POINT('Ctrl Pts',(0.355972796968906,0.105,10.58));
#36610=CARTESIAN_POINT('Ctrl Pts',(0.355972796968906,0.105,10.5657176144151));
#36611=CARTESIAN_POINT('Ctrl Pts',(0.356788151640763,0.101865883730478,
10.5505555299246));
#36612=CARTESIAN_POINT('Ctrl Pts',(0.359624783739593,0.0898042504698815,
10.5236404053753));
#36613=CARTESIAN_POINT('Ctrl Pts',(0.361563981230443,0.0810011204691618,
10.5119071676699));
#36614=CARTESIAN_POINT('Ctrl Pts',(0.365072430809911,0.0617529581653445,
10.4940720894225));
#36615=CARTESIAN_POINT('Ctrl Pts',(0.366864670140683,0.0500344296432505,
10.4867341690262));
#36616=CARTESIAN_POINT('Ctrl Pts',(0.369345626138981,0.0252940665523777,
10.477232189531));
#36617=CARTESIAN_POINT('Ctrl Pts',(0.370007671535977,0.01224397846036,10.4749916580037));
#36618=CARTESIAN_POINT('Ctrl Pts',(0.370007531253534,-0.0122691147063859,
10.4749913883312));
#36619=CARTESIAN_POINT('Ctrl Pts',(0.369345242689524,-0.0253193144167885,
10.4772314446462));
#36620=CARTESIAN_POINT('Ctrl Pts',(0.366864003616736,-0.0500599351797451,
10.4867328917034));
#36621=CARTESIAN_POINT('Ctrl Pts',(0.365071515657005,-0.0617788029685447,
10.4940702722811));
#36622=CARTESIAN_POINT('Ctrl Pts',(0.361562777085542,-0.0810274788691257,
10.5119049546835));
#36623=CARTESIAN_POINT('Ctrl Pts',(0.359623311987298,-0.0898312113319797,
10.5236369891132));
#36624=CARTESIAN_POINT('Ctrl Pts',(0.356786402927065,-0.101893545658019,
10.5505534454027));
#36625=CARTESIAN_POINT('Ctrl Pts',(0.355970657285474,-0.105028870652107,
10.5657068761491));
#36626=CARTESIAN_POINT('Ctrl Pts',(0.355970657285473,-0.105028870652107,
10.5942931238509));
#36627=CARTESIAN_POINT('Ctrl Pts',(0.356786402927066,-0.101893545658015,
10.6094465545972));
#36628=CARTESIAN_POINT('Ctrl Pts',(0.359623311987297,-0.0898312113319818,
10.6363630108867));
#36629=CARTESIAN_POINT('Ctrl Pts',(0.361562777085541,-0.0810274788691267,
10.6480950453164));
#36630=CARTESIAN_POINT('Ctrl Pts',(0.365071515657004,-0.0617788029685456,
10.6659297277188));
#36631=CARTESIAN_POINT('Ctrl Pts',(0.366864003616735,-0.0500599351797454,
10.6732671082965));
#36632=CARTESIAN_POINT('Ctrl Pts',(0.369345242689524,-0.0253193144167833,
10.6827685553537));
#36633=CARTESIAN_POINT('Ctrl Pts',(0.370007531253534,-0.0122691147063825,
10.6850086116688));
#36634=CARTESIAN_POINT('Ctrl Pts',(0.370007671535977,0.0122439784603628,
10.6850083419962));
#36635=CARTESIAN_POINT('Ctrl Pts',(0.36934562613898,0.0252940665523868,
10.6827678104689));
#36636=CARTESIAN_POINT('Ctrl Pts',(0.366864670140684,0.0500344296432442,
10.6732658309738));
#36637=CARTESIAN_POINT('Ctrl Pts',(0.365072430809911,0.0617529581653465,
10.6659279105774));
#36638=CARTESIAN_POINT('Ctrl Pts',(0.361563981230444,0.0810011204691621,
10.6480928323301));
#36639=CARTESIAN_POINT('Ctrl Pts',(0.359624783739593,0.0898042504698822,
10.6363595946247));
#36640=CARTESIAN_POINT('Ctrl Pts',(0.356788151640764,0.101865883730477,
10.6094444700754));
#36641=CARTESIAN_POINT('Ctrl Pts',(0.355972796968906,0.105,10.5942823855849));
#36642=CARTESIAN_POINT('Ctrl Pts',(0.355972796968906,0.105,10.58));
#36643=CARTESIAN_POINT('',(0.392324587256711,-0.0779994227069357,10.4700129327839));
#36644=CARTESIAN_POINT('',(0.38750984162879,-1.13350214458844E-5,10.4574879118198));
#36645=CARTESIAN_POINT('Ctrl Pts',(0.392324587256711,-0.0779994227069357,
10.4700129327839));
#36646=CARTESIAN_POINT('Ctrl Pts',(0.3914179472595,-0.0710898798500254,
10.4677824164029));
#36647=CARTESIAN_POINT('Ctrl Pts',(0.390647674347867,-0.0640945112802287,
10.4658141254007));
#36648=CARTESIAN_POINT('Ctrl Pts',(0.390006979063182,-0.057004463951378,
10.4641394037107));
#36649=CARTESIAN_POINT('Ctrl Pts',(0.389738309424129,-0.0540313182107284,
10.4634371246668));
#36650=CARTESIAN_POINT('Ctrl Pts',(0.389492752976518,-0.0510460578652142,
10.4627882375969));
#36651=CARTESIAN_POINT('Ctrl Pts',(0.389268637081754,-0.0480486678529736,
10.4621981307677));
#36652=CARTESIAN_POINT('Ctrl Pts',(0.388773697289598,-0.0414292016556794,
10.4608949329213));
#36653=CARTESIAN_POINT('Ctrl Pts',(0.388374227255805,-0.0347520280387355,
10.4598756996778));
#36654=CARTESIAN_POINT('Ctrl Pts',(0.388086077313271,-0.0280389018830262,
10.4591141553202));
#36655=CARTESIAN_POINT('Ctrl Pts',(0.387922086290066,-0.0242183478426609,
10.4586807475003));
#36656=CARTESIAN_POINT('Ctrl Pts',(0.387793898518198,-0.0203854294882888,
10.4583313532265));
#36657=CARTESIAN_POINT('Ctrl Pts',(0.38770134624721,-0.016541244006537,
10.458067528716));
#36658=CARTESIAN_POINT('Ctrl Pts',(0.387628168683527,-0.0135017926252255,
10.4578589327009));
#36659=CARTESIAN_POINT('Ctrl Pts',(0.387577297833347,-0.0104585822931131,
10.4577041418123));
#36660=CARTESIAN_POINT('Ctrl Pts',(0.387546792306271,-0.00741190850063314,
10.457606743657));
#36661=CARTESIAN_POINT('Ctrl Pts',(0.387530351373301,-0.00576990574219154,
10.4575542509877));
#36662=CARTESIAN_POINT('Ctrl Pts',(0.387519801015628,-0.00412720254292159,
10.4575184923917));
#36663=CARTESIAN_POINT('Ctrl Pts',(0.387514611538262,-0.00248401466470584,
10.4575004335314));
#36664=CARTESIAN_POINT('Ctrl Pts',(0.387512010291039,-0.00166035987157767,
10.4574913814522));
#36665=CARTESIAN_POINT('Ctrl Pts',(0.387510753131607,-0.000834836263530225,
10.4574867801339));
#36666=CARTESIAN_POINT('Ctrl Pts',(0.387510757804169,-1.23902195018747E-5,
10.4574867865088));
#36667=CARTESIAN_POINT('',(0.392324929054758,0.0779792774862667,10.4700112775181));
#36668=CARTESIAN_POINT('Ctrl Pts',(0.387510757804169,-1.23902195018771E-5,
10.4574867865088));
#36669=CARTESIAN_POINT('Ctrl Pts',(0.387510760917883,0.000525053166309368,
10.4574867906143));
#36670=CARTESIAN_POINT('Ctrl Pts',(0.387511301666096,0.00106361088239916,
10.4574887586056));
#36671=CARTESIAN_POINT('Ctrl Pts',(0.387512404993374,0.00160185431838427,
10.4574926511551));
#36672=CARTESIAN_POINT('Ctrl Pts',(0.38751555332776,0.00313772708404272,
10.4575037585098));
#36673=CARTESIAN_POINT('Ctrl Pts',(0.387523288659664,0.00467326443951501,
10.4575305065774));
#36674=CARTESIAN_POINT('Ctrl Pts',(0.387536072247131,0.00620825863535256,
10.4575720543493));
#36675=CARTESIAN_POINT('Ctrl Pts',(0.387557367005732,0.00876523498789927,
10.4576412641682));
#36676=CARTESIAN_POINT('Ctrl Pts',(0.387592709089323,0.0113200607878381,
10.4577514381998));
#36677=CARTESIAN_POINT('Ctrl Pts',(0.387643462116037,0.013872445644174,
10.4579000655362));
#36678=CARTESIAN_POINT('Ctrl Pts',(0.387745259086891,0.0189918456809811,
10.4581981721439));
#36679=CARTESIAN_POINT('Ctrl Pts',(0.387909563732894,0.0240968961657213,
10.4586494962418));
#36680=CARTESIAN_POINT('Ctrl Pts',(0.388138027023152,0.0291870207304549,
10.4592504297026));
#36681=CARTESIAN_POINT('Ctrl Pts',(0.38842171987062,0.0355076507542359,
10.4599966350314));
#36682=CARTESIAN_POINT('Ctrl Pts',(0.388803515452204,0.041793505019326,
10.460972224136));
#36683=CARTESIAN_POINT('Ctrl Pts',(0.389269380504044,0.0480237819441658,
10.4621989247368));
#36684=CARTESIAN_POINT('Ctrl Pts',(0.389445324894814,0.0503767858313245,
10.4626622157456));
#36685=CARTESIAN_POINT('Ctrl Pts',(0.389634435791483,0.0527216898232129,
10.4631616413639));
#36686=CARTESIAN_POINT('Ctrl Pts',(0.389837537339329,0.0550584657624432,
10.4636944184715));
#36687=CARTESIAN_POINT('Ctrl Pts',(0.390433239144012,0.0619122867150533,
10.4652570667517));
#36688=CARTESIAN_POINT('Ctrl Pts',(0.391148398175305,0.0686769039822018,
10.4670981722794));
#36689=CARTESIAN_POINT('Ctrl Pts',(0.391990110278716,0.0753629866058349,
10.4691851390505));
#36690=CARTESIAN_POINT('Ctrl Pts',(0.392099863338824,0.0762348025451608,
10.4694572641495));
#36691=CARTESIAN_POINT('Ctrl Pts',(0.392211757415364,0.077105234082072,
10.4697336199639));
#36692=CARTESIAN_POINT('Ctrl Pts',(0.392325801285573,0.0779742601298161,
10.4700141742871));
#36693=CARTESIAN_POINT('',(0.377017787534816,0.133632286077702,10.58));
#36694=CARTESIAN_POINT('Ctrl Pts',(0.392325801275538,0.0779742601803755,
10.4700141743233));
#36695=CARTESIAN_POINT('Ctrl Pts',(0.391112328098889,0.0840879572291327,
10.4744019432579));
#36696=CARTESIAN_POINT('Ctrl Pts',(0.389846070963454,0.0897381943461625,
10.4792299663789));
#36697=CARTESIAN_POINT('Ctrl Pts',(0.385743385887353,0.106539573413826,
10.4962244912617));
#36698=CARTESIAN_POINT('Ctrl Pts',(0.382671361121133,0.116705198842861,
10.5112796752359));
#36699=CARTESIAN_POINT('Ctrl Pts',(0.378257950025364,0.130263180113984,
10.5445759528919));
#36700=CARTESIAN_POINT('Ctrl Pts',(0.377017787534816,0.133632286077702,
10.5628264326263));
#36701=CARTESIAN_POINT('Ctrl Pts',(0.377017787534816,0.133632286077702,
10.58));
#36702=CARTESIAN_POINT('',(0.355972796968906,0.105,10.58));
#36703=CARTESIAN_POINT('',(0.377017787534816,0.133632286077702,10.58));
#36704=CARTESIAN_POINT('',(0.355970657285473,-0.105028870652107,10.58));
#36705=CARTESIAN_POINT('Ctrl Pts',(0.355972796968906,0.105,10.58));
#36706=CARTESIAN_POINT('Ctrl Pts',(0.355972796968906,0.105,10.5657176144151));
#36707=CARTESIAN_POINT('Ctrl Pts',(0.356788151640763,0.101865883730478,
10.5505555299246));
#36708=CARTESIAN_POINT('Ctrl Pts',(0.359624783739593,0.0898042504698815,
10.5236404053753));
#36709=CARTESIAN_POINT('Ctrl Pts',(0.361563981230443,0.0810011204691618,
10.5119071676699));
#36710=CARTESIAN_POINT('Ctrl Pts',(0.365072430809911,0.0617529581653445,
10.4940720894225));
#36711=CARTESIAN_POINT('Ctrl Pts',(0.366864670140683,0.0500344296432505,
10.4867341690262));
#36712=CARTESIAN_POINT('Ctrl Pts',(0.369345626138981,0.0252940665523777,
10.477232189531));
#36713=CARTESIAN_POINT('Ctrl Pts',(0.370007671535977,0.01224397846036,10.4749916580037));
#36714=CARTESIAN_POINT('Ctrl Pts',(0.370007531253534,-0.0122691147063859,
10.4749913883312));
#36715=CARTESIAN_POINT('Ctrl Pts',(0.369345242689524,-0.0253193144167885,
10.4772314446462));
#36716=CARTESIAN_POINT('Ctrl Pts',(0.366864003616736,-0.0500599351797451,
10.4867328917034));
#36717=CARTESIAN_POINT('Ctrl Pts',(0.365071515657005,-0.0617788029685447,
10.4940702722811));
#36718=CARTESIAN_POINT('Ctrl Pts',(0.361562777085542,-0.0810274788691257,
10.5119049546835));
#36719=CARTESIAN_POINT('Ctrl Pts',(0.359623311987298,-0.0898312113319797,
10.5236369891132));
#36720=CARTESIAN_POINT('Ctrl Pts',(0.356786402927065,-0.101893545658019,
10.5505534454027));
#36721=CARTESIAN_POINT('Ctrl Pts',(0.355970657285474,-0.105028870652107,
10.5657068761491));
#36722=CARTESIAN_POINT('Ctrl Pts',(0.355970657285473,-0.105028870652107,
10.58));
#36723=CARTESIAN_POINT('Ctrl Pts',(0.355970657285473,-0.105028870652107,
10.58));
#36724=CARTESIAN_POINT('Ctrl Pts',(0.355970657285473,-0.105028870652107,
10.5942931238509));
#36725=CARTESIAN_POINT('Ctrl Pts',(0.356786402927066,-0.101893545658015,
10.6094465545972));
#36726=CARTESIAN_POINT('Ctrl Pts',(0.359623311987297,-0.0898312113319818,
10.6363630108867));
#36727=CARTESIAN_POINT('Ctrl Pts',(0.361562777085541,-0.0810274788691267,
10.6480950453164));
#36728=CARTESIAN_POINT('Ctrl Pts',(0.365071515657004,-0.0617788029685456,
10.6659297277188));
#36729=CARTESIAN_POINT('Ctrl Pts',(0.366864003616735,-0.0500599351797454,
10.6732671082965));
#36730=CARTESIAN_POINT('Ctrl Pts',(0.369345242689524,-0.0253193144167833,
10.6827685553537));
#36731=CARTESIAN_POINT('Ctrl Pts',(0.370007531253534,-0.0122691147063825,
10.6850086116688));
#36732=CARTESIAN_POINT('Ctrl Pts',(0.370007671535977,0.0122439784603628,
10.6850083419962));
#36733=CARTESIAN_POINT('Ctrl Pts',(0.36934562613898,0.0252940665523868,
10.6827678104689));
#36734=CARTESIAN_POINT('Ctrl Pts',(0.366864670140684,0.0500344296432442,
10.6732658309738));
#36735=CARTESIAN_POINT('Ctrl Pts',(0.365072430809911,0.0617529581653465,
10.6659279105774));
#36736=CARTESIAN_POINT('Ctrl Pts',(0.361563981230444,0.0810011204691621,
10.6480928323301));
#36737=CARTESIAN_POINT('Ctrl Pts',(0.359624783739593,0.0898042504698822,
10.6363595946247));
#36738=CARTESIAN_POINT('Ctrl Pts',(0.356788151640764,0.101865883730477,
10.6094444700754));
#36739=CARTESIAN_POINT('Ctrl Pts',(0.355972796968906,0.105,10.5942823855849));
#36740=CARTESIAN_POINT('Ctrl Pts',(0.355972796968906,0.105,10.58));
#36741=CARTESIAN_POINT('',(0.398342724806441,0.0363740785969918,10.7099999999999));
#36742=CARTESIAN_POINT('Ctrl Pts',(0.377017787534816,0.133632286077702,
10.58));
#36743=CARTESIAN_POINT('Ctrl Pts',(0.377017787534816,0.133632286077702,
10.5971735673738));
#36744=CARTESIAN_POINT('Ctrl Pts',(0.378257950025365,0.130263180113984,
10.6154240471081));
#36745=CARTESIAN_POINT('Ctrl Pts',(0.382671361121131,0.116705198842871,
10.6487203247641));
#36746=CARTESIAN_POINT('Ctrl Pts',(0.385743385887349,0.106539573413844,
10.6637755087383));
#36747=CARTESIAN_POINT('Ctrl Pts',(0.391476660649127,0.0830605783691558,
10.6875244143432));
#36748=CARTESIAN_POINT('Ctrl Pts',(0.394506895081026,0.068151397938163,
10.6978321246935));
#36749=CARTESIAN_POINT('Ctrl Pts',(0.397311776340776,0.0466679026410903,
10.7067852229923));
#36750=CARTESIAN_POINT('Ctrl Pts',(0.397874093042254,0.0415485580836963,
10.7085446143007));
#36751=CARTESIAN_POINT('Ctrl Pts',(0.398342795273631,0.0363570891554297,
10.7099910945945));
#36752=CARTESIAN_POINT('',(0.398342724806499,-0.03637407859636,10.71));
#36753=CARTESIAN_POINT('Ctrl Pts',(0.398342247906153,-0.0363817831807788,
10.7099916508698));
#36754=CARTESIAN_POINT('Ctrl Pts',(0.397665066396712,-0.0326461425599149,
10.7099853342879));
#36755=CARTESIAN_POINT('Ctrl Pts',(0.397083002923767,-0.0288995863484758,
10.7099810242112));
#36756=CARTESIAN_POINT('Ctrl Pts',(0.396604742785928,-0.0251364196314169,
10.7099811705733));
#36757=CARTESIAN_POINT('Ctrl Pts',(0.395872802041393,-0.0193771793544803,
10.7099813945695));
#36758=CARTESIAN_POINT('Ctrl Pts',(0.395389651144243,-0.0136148183112041,
10.7099940233747));
#36759=CARTESIAN_POINT('Ctrl Pts',(0.395163312234515,-0.00781210949747046,
10.7100055875414));
#36760=CARTESIAN_POINT('Ctrl Pts',(0.39510698933434,-0.00636814482673823,
10.7100084652058));
#36761=CARTESIAN_POINT('Ctrl Pts',(0.395066553089786,-0.00492380828909155,
10.7100110998838));
#36762=CARTESIAN_POINT('Ctrl Pts',(0.395041766952865,-0.00347852169201901,
10.7100129042549));
#36763=CARTESIAN_POINT('Ctrl Pts',(0.39502804355889,-0.00267830673951237,
10.710013903285));
#36764=CARTESIAN_POINT('Ctrl Pts',(0.395019119897156,-0.00187802612202232,
10.7100146444282));
#36765=CARTESIAN_POINT('Ctrl Pts',(0.395014934638734,-0.00107759250488598,
10.7100150047607));
#36766=CARTESIAN_POINT('Ctrl Pts',(0.39501307801116,-0.00072251117550288,
10.7100151646083));
#36767=CARTESIAN_POINT('Ctrl Pts',(0.395012153921115,-0.000367158428743391,
10.7100152493742));
#36768=CARTESIAN_POINT('Ctrl Pts',(0.395012155839313,-1.23041126689258E-5,
10.7100152469662));
#36769=CARTESIAN_POINT('Ctrl Pts',(0.39501215756284,0.000306537193240153,
10.7100152448027));
#36770=CARTESIAN_POINT('Ctrl Pts',(0.39501290706911,0.000625760855678687,
10.71001517254));
#36771=CARTESIAN_POINT('Ctrl Pts',(0.395014408943175,0.000944808589093608,
10.7100150384837));
#36772=CARTESIAN_POINT('Ctrl Pts',(0.395018110328239,0.00173110521886498,
10.7100147081003));
#36773=CARTESIAN_POINT('Ctrl Pts',(0.395026381611087,0.00251725892388332,
10.7100140041378));
#36774=CARTESIAN_POINT('Ctrl Pts',(0.395039281660777,0.00330335200016204,
10.7100130440316));
#36775=CARTESIAN_POINT('Ctrl Pts',(0.395061946304566,0.0046844722273079,
10.7100113571803));
#36776=CARTESIAN_POINT('Ctrl Pts',(0.395098893168343,0.00606475624817226,
10.7100088886225));
#36777=CARTESIAN_POINT('Ctrl Pts',(0.395150336257454,0.00744470557640811,
10.7100061596766));
#36778=CARTESIAN_POINT('Ctrl Pts',(0.395255859270476,0.0102753367350618,
10.7100005619064));
#36779=CARTESIAN_POINT('Ctrl Pts',(0.395422268232612,0.0130994926770529,
10.7099940194268));
#36780=CARTESIAN_POINT('Ctrl Pts',(0.39564974640504,0.0159218010131768,
10.709989245592));
#36781=CARTESIAN_POINT('Ctrl Pts',(0.396153036495399,0.0221660916294672,
10.7099786835951));
#36782=CARTESIAN_POINT('Ctrl Pts',(0.396952990163372,0.028357002547276,
10.7099791005708));
#36783=CARTESIAN_POINT('Ctrl Pts',(0.398019360427533,0.0345300530562236,
10.7099882094322));
#36784=CARTESIAN_POINT('Ctrl Pts',(0.398124600500028,0.0351392713595705,
10.7099891083857));
#36785=CARTESIAN_POINT('Ctrl Pts',(0.3982324238991,0.035748280023644,10.7099900739033));
#36786=CARTESIAN_POINT('Ctrl Pts',(0.398342795273687,0.0363570891548118,
10.7099910945946));
#36787=CARTESIAN_POINT('Ctrl Pts',(0.398342247906152,-0.0363817831807865,
10.7099916508698));
#36788=CARTESIAN_POINT('Ctrl Pts',(0.397873464638273,-0.0415732844705318,
10.7085452525623));
#36789=CARTESIAN_POINT('Ctrl Pts',(0.397311072202917,-0.0466926654416248,
10.706785937381));
#36790=CARTESIAN_POINT('Ctrl Pts',(0.394505922058272,-0.0681763245922005,
10.6978331049505));
#36791=CARTESIAN_POINT('Ctrl Pts',(0.39147532466622,-0.0830858365897902,
10.6875258088738));
#36792=CARTESIAN_POINT('Ctrl Pts',(0.385741628020435,-0.1065653335745,10.6637772070525));
#36793=CARTESIAN_POINT('Ctrl Pts',(0.382669212588457,-0.116731547791971,
10.6487229465094));
#36794=CARTESIAN_POINT('Ctrl Pts',(0.378255397171518,-0.13029021421689,
10.6154256468348));
#36795=CARTESIAN_POINT('Ctrl Pts',(0.377014663925106,-0.133660501471554,
10.5971818082517));
#36796=CARTESIAN_POINT('Ctrl Pts',(0.377014663925107,-0.133660501471551,
10.5628181917482));
#36797=CARTESIAN_POINT('Ctrl Pts',(0.378255397171514,-0.130290214216898,
10.5445743531652));
#36798=CARTESIAN_POINT('Ctrl Pts',(0.382669212588462,-0.11673154779195,
10.5112770534905));
#36799=CARTESIAN_POINT('Ctrl Pts',(0.385741628020441,-0.106565333574474,
10.4962227929474));
#36800=CARTESIAN_POINT('Ctrl Pts',(0.389844614775671,-0.0897635962138861,
10.4792284863512));
#36801=CARTESIAN_POINT('Ctrl Pts',(0.391110990879574,-0.0841132370178976,
10.4744005782828));
#36802=CARTESIAN_POINT('Ctrl Pts',(0.392324586605502,-0.0779994259875773,
10.4700129351383));
#36803=CARTESIAN_POINT('Origin',(0.,0.,10.58));
#36804=CARTESIAN_POINT('Origin',(0.,0.,10.47));
#36805=CARTESIAN_POINT('Origin',(0.,0.,10.71));
#36806=CARTESIAN_POINT('Origin',(0.,0.,10.46));
#36807=CARTESIAN_POINT('',(0.39,4.77612251667468E-17,10.46));
#36808=CARTESIAN_POINT('Origin',(0.245,0.,10.58));
#36809=CARTESIAN_POINT('',(0.0400000000000001,0.103841838612921,10.5955522523606));
#36810=CARTESIAN_POINT('',(0.0400000000000005,-0.103841838612921,10.5955522523606));
#36811=CARTESIAN_POINT('Ctrl Pts',(0.0399999999999981,0.103841838612921,
10.5955522523606));
#36812=CARTESIAN_POINT('Ctrl Pts',(0.0476893855684824,0.103106895932074,
10.6004594386308));
#36813=CARTESIAN_POINT('Ctrl Pts',(0.0540917217987843,0.101964920739599,
10.6056067063421));
#36814=CARTESIAN_POINT('Ctrl Pts',(0.0730376318384075,0.0970386910483417,
10.6218026292622));
#36815=CARTESIAN_POINT('Ctrl Pts',(0.0846768485016188,0.0912869792271611,
10.6336828384074));
#36816=CARTESIAN_POINT('Ctrl Pts',(0.10413011273211,0.0751729867880902,
10.6544069799274));
#36817=CARTESIAN_POINT('Ctrl Pts',(0.113106530347439,0.0641959568676023,
10.6646713825649));
#36818=CARTESIAN_POINT('Ctrl Pts',(0.12619070930351,0.0355990566133719,
10.6801818582265));
#36819=CARTESIAN_POINT('Ctrl Pts',(0.13392036430385,-1.94332703229122E-14,
10.6898712751113));
#36820=CARTESIAN_POINT('Ctrl Pts',(0.126190709303508,-0.0355990566133874,
10.6801818582265));
#36821=CARTESIAN_POINT('Ctrl Pts',(0.113106530347436,-0.0641959568676066,
10.6646713825649));
#36822=CARTESIAN_POINT('Ctrl Pts',(0.104130112732119,-0.0751729867880824,
10.6544069799274));
#36823=CARTESIAN_POINT('Ctrl Pts',(0.0846768485015844,-0.0912869792271854,
10.6336828384074));
#36824=CARTESIAN_POINT('Ctrl Pts',(0.0730376318384033,-0.097038691048342,
10.6218026292622));
#36825=CARTESIAN_POINT('Ctrl Pts',(0.0540917217987876,-0.101964920739599,
10.6056067063421));
#36826=CARTESIAN_POINT('Ctrl Pts',(0.0476893855684835,-0.103106895932074,
10.6004594386308));
#36827=CARTESIAN_POINT('Ctrl Pts',(0.0399999999999999,-0.103841838612921,
10.5955522523606));
#36828=CARTESIAN_POINT('Origin',(0.04,0.,10.58));
#36829=CARTESIAN_POINT('',(0.0399999999999996,-0.105,10.58));
#36830=CARTESIAN_POINT('Origin',(0.04,0.,10.58));
#36831=CARTESIAN_POINT('',(0.245,-0.105,10.58));
#36832=CARTESIAN_POINT('Origin',(0.04,0.,10.58));
#36833=CARTESIAN_POINT('Ctrl Pts',(0.00894444267269635,0.0995991814488194,
10.6458389285088));
#36834=CARTESIAN_POINT('Ctrl Pts',(0.0132379567575632,0.0992136050812441,
10.6483379094571));
#36835=CARTESIAN_POINT('Ctrl Pts',(0.0183531529868693,0.0984395024940475,
10.6518751113904));
#36836=CARTESIAN_POINT('Ctrl Pts',(0.0347076968180254,0.0945110273189231,
10.6639299928277));
#36837=CARTESIAN_POINT('Ctrl Pts',(0.0471226277111957,0.0892804802504122,
10.6739642355804));
#36838=CARTESIAN_POINT('Ctrl Pts',(0.0685122659420266,0.0739398403060646,
10.6909132508036));
#36839=CARTESIAN_POINT('Ctrl Pts',(0.0790926347687259,0.0632798166374917,
10.6991949609786));
#36840=CARTESIAN_POINT('Ctrl Pts',(0.095041784574442,0.0352045494840137,
10.7113488867527));
#36841=CARTESIAN_POINT('Ctrl Pts',(0.104990250453808,-1.94764728236301E-14,
10.7186701978954));
#36842=CARTESIAN_POINT('Ctrl Pts',(0.0950417845744413,-0.0352045494840311,
10.7113488867527));
#36843=CARTESIAN_POINT('Ctrl Pts',(0.0790926347687328,-0.0632798166374956,
10.6991949609786));
#36844=CARTESIAN_POINT('Ctrl Pts',(0.0685122659420257,-0.0739398403060731,
10.6909132508036));
#36845=CARTESIAN_POINT('Ctrl Pts',(0.047122627711224,-0.0892804802503985,
10.6739642355805));
#36846=CARTESIAN_POINT('Ctrl Pts',(0.0347076968180293,-0.0945110273189234,
10.6639299928277));
#36847=CARTESIAN_POINT('Ctrl Pts',(0.0183531529868686,-0.0984395024940474,
10.6518751113904));
#36848=CARTESIAN_POINT('Ctrl Pts',(0.0132379567575637,-0.099213605081244,
10.6483379094571));
#36849=CARTESIAN_POINT('Ctrl Pts',(0.00894444267269703,-0.0995991814488193,
10.6458389285088));
#36850=CARTESIAN_POINT('Ctrl Pts',(0.0192962951151303,0.10101340050352,
10.6290767031261));
#36851=CARTESIAN_POINT('Ctrl Pts',(0.0246829710160882,0.100510889482336,
10.6323644063093));
#36852=CARTESIAN_POINT('Ctrl Pts',(0.0302700623455481,0.0996151368283168,
10.636456666124));
#36853=CARTESIAN_POINT('Ctrl Pts',(0.0474468559781996,0.0953527264698026,
10.6498673135763));
#36854=CARTESIAN_POINT('Ctrl Pts',(0.0596224855482002,0.0899496672599846,
10.6605286913046));
#36855=CARTESIAN_POINT('Ctrl Pts',(0.0803741298379308,0.0743507178323205,
10.6787417409477));
#36856=CARTESIAN_POINT('Ctrl Pts',(0.0904178647965569,0.0635857671411624,
10.6876757555526));
#36857=CARTESIAN_POINT('Ctrl Pts',(0.105408337598459,0.0353360773731678,
10.7009599149888));
#36858=CARTESIAN_POINT('Ctrl Pts',(0.114618845129398,-1.94606231903746E-14,
10.7090623931681));
#36859=CARTESIAN_POINT('Ctrl Pts',(0.105408337598459,-0.0353360773731852,
10.7009599149888));
#36860=CARTESIAN_POINT('Ctrl Pts',(0.0904178647965638,-0.0635857671411668,
10.6876757555526));
#36861=CARTESIAN_POINT('Ctrl Pts',(0.08037412983793,-0.074350717832329,
10.6787417409477));
#36862=CARTESIAN_POINT('Ctrl Pts',(0.0596224855482286,-0.0899496672599712,
10.6605286913046));
#36863=CARTESIAN_POINT('Ctrl Pts',(0.0474468559782033,-0.0953527264698027,
10.6498673135763));
#36864=CARTESIAN_POINT('Ctrl Pts',(0.0302700623455475,-0.0996151368283167,
10.636456666124));
#36865=CARTESIAN_POINT('Ctrl Pts',(0.0246829710160884,-0.100510889482335,
10.6323644063093));
#36866=CARTESIAN_POINT('Ctrl Pts',(0.0192962951151313,-0.10101340050352,
10.6290767031261));
#36867=CARTESIAN_POINT('Ctrl Pts',(0.0296481475575642,0.102427619558221,
10.6123144777433));
#36868=CARTESIAN_POINT('Ctrl Pts',(0.0362443713099573,0.101809611530983,
10.6164329417787));
#36869=CARTESIAN_POINT('Ctrl Pts',(0.0421748124401054,0.100789286405329,
10.6210251516086));
#36870=CARTESIAN_POINT('Ctrl Pts',(0.0602984726782332,0.0961969918974622,
10.6358653085135));
#36871=CARTESIAN_POINT('Ctrl Pts',(0.0721769906646143,0.0906177922175886,
10.6471183826832));
#36872=CARTESIAN_POINT('Ctrl Pts',(0.0922682488362055,0.0747621092618343,
10.6665784897832));
#36873=CARTESIAN_POINT('Ctrl Pts',(0.101781300319608,0.0638900063639316,
10.6761905879909));
#36874=CARTESIAN_POINT('Ctrl Pts',(0.115824156279493,0.0354675287242178,
10.6905708299903));
#36875=CARTESIAN_POINT('Ctrl Pts',(0.12429176962826,-1.94491199561677E-14,
10.6994790798386));
#36876=CARTESIAN_POINT('Ctrl Pts',(0.115824156279491,-0.0354675287242332,
10.6905708299903));
#36877=CARTESIAN_POINT('Ctrl Pts',(0.101781300319605,-0.0638900063639355,
10.6761905879909));
#36878=CARTESIAN_POINT('Ctrl Pts',(0.0922682488362152,-0.0747621092618265,
10.6665784897832));
#36879=CARTESIAN_POINT('Ctrl Pts',(0.0721769906645798,-0.0906177922176127,
10.6471183826832));
#36880=CARTESIAN_POINT('Ctrl Pts',(0.0602984726782293,-0.0961969918974626,
10.6358653085135));
#36881=CARTESIAN_POINT('Ctrl Pts',(0.0421748124401086,-0.100789286405329,
10.6210251516086));
#36882=CARTESIAN_POINT('Ctrl Pts',(0.0362443713099588,-0.101809611530983,
10.6164329417787));
#36883=CARTESIAN_POINT('Ctrl Pts',(0.0296481475575656,-0.102427619558221,
10.6123144777433));
#36884=CARTESIAN_POINT('Ctrl Pts',(0.0399999999999981,0.103841838612921,
10.5955522523606));
#36885=CARTESIAN_POINT('Ctrl Pts',(0.0476893855684824,0.103106895932074,
10.6004594386308));
#36886=CARTESIAN_POINT('Ctrl Pts',(0.0540917217987843,0.101964920739599,
10.6056067063421));
#36887=CARTESIAN_POINT('Ctrl Pts',(0.0730376318384075,0.0970386910483417,
10.6218026292622));
#36888=CARTESIAN_POINT('Ctrl Pts',(0.0846768485016188,0.0912869792271611,
10.6336828384074));
#36889=CARTESIAN_POINT('Ctrl Pts',(0.10413011273211,0.0751729867880902,
10.6544069799274));
#36890=CARTESIAN_POINT('Ctrl Pts',(0.113106530347439,0.0641959568676023,
10.6646713825649));
#36891=CARTESIAN_POINT('Ctrl Pts',(0.12619070930351,0.0355990566133719,
10.6801818582265));
#36892=CARTESIAN_POINT('Ctrl Pts',(0.13392036430385,-1.94332703229122E-14,
10.6898712751113));
#36893=CARTESIAN_POINT('Ctrl Pts',(0.126190709303508,-0.0355990566133874,
10.6801818582265));
#36894=CARTESIAN_POINT('Ctrl Pts',(0.113106530347436,-0.0641959568676066,
10.6646713825649));
#36895=CARTESIAN_POINT('Ctrl Pts',(0.104130112732119,-0.0751729867880824,
10.6544069799274));
#36896=CARTESIAN_POINT('Ctrl Pts',(0.0846768485015844,-0.0912869792271854,
10.6336828384074));
#36897=CARTESIAN_POINT('Ctrl Pts',(0.0730376318384033,-0.097038691048342,
10.6218026292622));
#36898=CARTESIAN_POINT('Ctrl Pts',(0.0540917217987876,-0.101964920739599,
10.6056067063421));
#36899=CARTESIAN_POINT('Ctrl Pts',(0.0476893855684835,-0.103106895932074,
10.6004594386308));
#36900=CARTESIAN_POINT('Ctrl Pts',(0.0399999999999999,-0.103841838612921,
10.5955522523606));
#36901=CARTESIAN_POINT('Ctrl Pts',(0.04,0.103841838612921,10.5955522523606));
#36902=CARTESIAN_POINT('Ctrl Pts',(0.04,0.102606878649513,10.6075587254027));
#36903=CARTESIAN_POINT('Ctrl Pts',(0.0399999999999975,0.101164195082993,
10.6196695728954));
#36904=CARTESIAN_POINT('Ctrl Pts',(0.0399999999999975,0.0972792927935932,
10.6440647058907));
#36905=CARTESIAN_POINT('Ctrl Pts',(0.04,0.0948285697695771,10.6562661891283));
#36906=CARTESIAN_POINT('Ctrl Pts',(0.04,0.0916515138991168,10.6683225406115));
#36907=CARTESIAN_POINT('Ctrl Pts',(0.04,-0.0916515138991168,10.6683225406115));
#36908=CARTESIAN_POINT('Ctrl Pts',(0.04,-0.0935748723716089,10.6610237436378));
#36909=CARTESIAN_POINT('Ctrl Pts',(0.0399999999895056,-0.0952353918400671,
10.6536541522208));
#36910=CARTESIAN_POINT('Ctrl Pts',(0.0399999999895056,-0.0999669573193089,
10.62939385374));
#36911=CARTESIAN_POINT('Ctrl Pts',(0.0400000000000004,-0.102095272100589,
10.6125326439262));
#36912=CARTESIAN_POINT('Ctrl Pts',(0.0400000000000004,-0.103841838612921,
10.5955522523606));
#36913=CARTESIAN_POINT('Origin',(0.55,0.,10.725));
#36914=CARTESIAN_POINT('',(0.435,1.40834381901946E-17,10.71));
#36915=CARTESIAN_POINT('Origin',(0.55,0.,10.71));
#36916=CARTESIAN_POINT('',(0.465,-1.04094977927525E-17,10.74));
#36917=CARTESIAN_POINT('',(0.45,1.22464679914735E-17,10.725));
#36918=CARTESIAN_POINT('Origin',(0.55,0.,10.74));
#36919=CARTESIAN_POINT('Origin',(0.55,0.,10.825));
#36920=CARTESIAN_POINT('',(0.465,1.04094977927525E-17,10.88));
#36921=CARTESIAN_POINT('',(0.465,-1.04094977927525E-17,10.825));
#36922=CARTESIAN_POINT('Origin',(0.55,0.,10.88));
#36923=CARTESIAN_POINT('Origin',(0.7,0.,10.71));
#36924=CARTESIAN_POINT('',(0.68,8.327598234202E-17,10.71));
#36925=CARTESIAN_POINT('Origin',(0.,0.,10.71));
#36926=CARTESIAN_POINT('',(-0.39,0.476313972081441,10.71));
#36927=CARTESIAN_POINT('Origin',(-0.275,0.476313972081441,10.71));
#36928=CARTESIAN_POINT('',(-0.39,-0.476313972081441,10.71));
#36929=CARTESIAN_POINT('Origin',(-0.275,-0.476313972081441,10.71));
#36930=CARTESIAN_POINT('Origin',(0.55,0.,10.895));
#36931=CARTESIAN_POINT('',(0.435,-1.40834381901946E-17,10.91));
#36932=CARTESIAN_POINT('Origin',(0.55,0.,10.91));
#36933=CARTESIAN_POINT('',(0.45,-1.22464679914735E-17,10.895));
#36934=CARTESIAN_POINT('Origin',(0.2,0.,10.91));
#36935=CARTESIAN_POINT('',(0.68,-8.327598234202E-17,10.91));
#36936=CARTESIAN_POINT('Origin',(0.,0.,10.91));
#36937=CARTESIAN_POINT('',(-0.39,0.476313972081441,10.91));
#36938=CARTESIAN_POINT('Origin',(-0.275,0.476313972081441,10.91));
#36939=CARTESIAN_POINT('',(-0.39,-0.476313972081441,10.91));
#36940=CARTESIAN_POINT('Origin',(-0.275,-0.476313972081441,10.91));
#36941=CARTESIAN_POINT('Origin',(-0.275,0.476313972081441,10.725));
#36942=CARTESIAN_POINT('',(-0.36,0.476313972081441,10.74));
#36943=CARTESIAN_POINT('',(-0.375,0.476313972081441,10.725));
#36944=CARTESIAN_POINT('Origin',(-0.275,0.476313972081441,10.74));
#36945=CARTESIAN_POINT('Origin',(-0.275,0.476313972081441,10.825));
#36946=CARTESIAN_POINT('',(-0.36,0.476313972081441,10.88));
#36947=CARTESIAN_POINT('',(-0.36,0.476313972081441,10.825));
#36948=CARTESIAN_POINT('Origin',(-0.275,0.476313972081441,10.88));
#36949=CARTESIAN_POINT('Origin',(-0.275,0.476313972081441,10.895));
#36950=CARTESIAN_POINT('',(-0.375,0.476313972081441,10.895));
#36951=CARTESIAN_POINT('Origin',(-0.275,-0.476313972081441,10.725));
#36952=CARTESIAN_POINT('',(-0.36,-0.476313972081441,10.74));
#36953=CARTESIAN_POINT('',(-0.375,-0.476313972081441,10.725));
#36954=CARTESIAN_POINT('Origin',(-0.275,-0.476313972081441,10.74));
#36955=CARTESIAN_POINT('Origin',(-0.275,-0.476313972081441,10.825));
#36956=CARTESIAN_POINT('',(-0.36,-0.476313972081441,10.88));
#36957=CARTESIAN_POINT('',(-0.36,-0.476313972081441,10.825));
#36958=CARTESIAN_POINT('Origin',(-0.275,-0.476313972081441,10.88));
#36959=CARTESIAN_POINT('Origin',(-0.275,-0.476313972081441,10.895));
#36960=CARTESIAN_POINT('',(-0.375,-0.476313972081441,10.895));
#36961=CARTESIAN_POINT('Origin',(0.04,0.105,10.58));
#36962=CARTESIAN_POINT('Origin',(0.04,0.105,10.58));
#36963=CARTESIAN_POINT('Origin',(0.,0.,10.9));
#36964=CARTESIAN_POINT('',(0.7,8.57252759403147E-17,10.89));
#36965=CARTESIAN_POINT('',(0.69,8.45006291411674E-17,10.9));
#36966=CARTESIAN_POINT('',(-0.7,-8.57252759403147E-17,10.89));
#36967=CARTESIAN_POINT('Origin',(0.,0.,10.89));
#36968=CARTESIAN_POINT('Origin',(0.,0.,10.89));
#36969=CARTESIAN_POINT('Origin',(0.,0.,10.81));
#36970=CARTESIAN_POINT('',(-0.7,-8.57252759403147E-17,10.73));
#36971=CARTESIAN_POINT('',(-0.7,-8.57252759403147E-17,10.81));
#36972=CARTESIAN_POINT('',(0.7,-8.57252759403147E-17,10.73));
#36973=CARTESIAN_POINT('Origin',(0.,0.,10.73));
#36974=CARTESIAN_POINT('Origin',(0.,0.,10.73));
#36975=CARTESIAN_POINT('Origin',(0.,0.,10.72));
#36976=CARTESIAN_POINT('',(0.69,8.45006291411674E-17,10.72));
#36977=CARTESIAN_POINT('',(0.,0.,0.));
#36978=CARTESIAN_POINT('Origin',(0.,0.,10.975));
#36979=CARTESIAN_POINT('',(0.2325,-2.8473038080176E-17,10.96));
#36980=CARTESIAN_POINT('Origin',(0.,0.,10.96));
#36981=CARTESIAN_POINT('',(0.2025,2.47990976827339E-17,10.99));
#36982=CARTESIAN_POINT('',(0.2175,-2.66360678814549E-17,10.975));
#36983=CARTESIAN_POINT('',(-0.2025,-2.47990976827339E-17,10.99));
#36984=CARTESIAN_POINT('Origin',(0.,0.,10.99));
#36985=CARTESIAN_POINT('Origin',(0.,0.,10.99));
#36986=CARTESIAN_POINT('Origin',(0.,0.,11.01));
#36987=CARTESIAN_POINT('',(0.2025,-2.47990976827339E-17,11.03));
#36988=CARTESIAN_POINT('',(-0.2025,-2.47990976827339E-17,11.03));
#36989=CARTESIAN_POINT('Origin',(0.,0.,11.03));
#36990=CARTESIAN_POINT('Origin',(0.,0.,11.03));
#36991=CARTESIAN_POINT('',(-0.2025,-2.47990976827339E-17,11.01));
#36992=CARTESIAN_POINT('Origin',(0.7,0.,10.96));
#36993=CARTESIAN_POINT('',(-0.335,0.580237020535574,10.96));
#36994=CARTESIAN_POINT('',(-0.394999999999999,0.476313972081441,10.96));
#36995=CARTESIAN_POINT('Origin',(-0.275,0.476313972081441,10.96));
#36996=CARTESIAN_POINT('',(0.67,0.,10.96));
#36997=CARTESIAN_POINT('Origin',(0.,0.,10.96));
#36998=CARTESIAN_POINT('',(0.43,1.46957615897682E-17,10.96));
#36999=CARTESIAN_POINT('Origin',(0.55,0.,10.96));
#37000=CARTESIAN_POINT('Origin',(0.55,0.,10.96));
#37001=CARTESIAN_POINT('',(-0.335,-0.580237020535574,10.96));
#37002=CARTESIAN_POINT('Origin',(0.,0.,10.96));
#37003=CARTESIAN_POINT('',(-0.395,-0.476313972081441,10.96));
#37004=CARTESIAN_POINT('Origin',(-0.275,-0.476313972081441,10.96));
#37005=CARTESIAN_POINT('Origin',(-0.275,-0.476313972081441,10.96));
#37006=CARTESIAN_POINT('Origin',(0.,0.,10.96));
#37007=CARTESIAN_POINT('Origin',(-0.275,0.476313972081441,10.96));
#37008=CARTESIAN_POINT('Origin',(0.,0.,11.045));
#37009=CARTESIAN_POINT('',(0.2325,2.8473038080176E-17,11.06));
#37010=CARTESIAN_POINT('',(0.2175,-2.66360678814549E-17,11.045));
#37011=CARTESIAN_POINT('Origin',(0.,0.,11.06));
#37012=CARTESIAN_POINT('Origin',(0.2025,0.,11.06));
#37013=CARTESIAN_POINT('',(0.68,-8.327598234202E-17,11.06));
#37014=CARTESIAN_POINT('Origin',(0.,0.,11.06));
#37015=CARTESIAN_POINT('',(0.43,-1.46957615897682E-17,11.06));
#37016=CARTESIAN_POINT('Origin',(0.55,0.,11.06));
#37017=CARTESIAN_POINT('',(-0.395,-0.476313972081441,11.06));
#37018=CARTESIAN_POINT('Origin',(-0.275,-0.476313972081441,11.06));
#37019=CARTESIAN_POINT('',(-0.395,0.476313972081441,11.06));
#37020=CARTESIAN_POINT('Origin',(-0.275,0.476313972081441,11.06));
#37021=CARTESIAN_POINT('Origin',(0.,0.,10.975));
#37022=CARTESIAN_POINT('',(0.7,-8.57252759403147E-17,10.99));
#37023=CARTESIAN_POINT('',(-0.7,-8.57252759403147E-17,10.99));
#37024=CARTESIAN_POINT('Origin',(0.,0.,10.99));
#37025=CARTESIAN_POINT('Origin',(0.,0.,10.99));
#37026=CARTESIAN_POINT('',(0.685,8.38883057415937E-17,10.975));
#37027=CARTESIAN_POINT('Origin',(0.,0.,11.01));
#37028=CARTESIAN_POINT('',(0.7,8.57252759403147E-17,11.04));
#37029=CARTESIAN_POINT('',(-0.7,-8.57252759403147E-17,11.04));
#37030=CARTESIAN_POINT('Origin',(0.,0.,11.04));
#37031=CARTESIAN_POINT('Origin',(0.,0.,11.04));
#37032=CARTESIAN_POINT('',(-0.7,-8.57252759403147E-17,11.01));
#37033=CARTESIAN_POINT('Origin',(0.55,0.,10.975));
#37034=CARTESIAN_POINT('',(0.46,-1.10218211923262E-17,10.99));
#37035=CARTESIAN_POINT('',(0.445,1.28587913910472E-17,10.975));
#37036=CARTESIAN_POINT('Origin',(0.55,0.,10.99));
#37037=CARTESIAN_POINT('Origin',(0.55,0.,11.025));
#37038=CARTESIAN_POINT('',(0.46,1.10218211923262E-17,11.03));
#37039=CARTESIAN_POINT('',(0.46,-1.10218211923262E-17,11.025));
#37040=CARTESIAN_POINT('Origin',(0.55,0.,11.03));
#37041=CARTESIAN_POINT('Origin',(0.55,0.,11.045));
#37042=CARTESIAN_POINT('',(0.445,-1.28587913910472E-17,11.045));
#37043=CARTESIAN_POINT('Origin',(-0.275,0.476313972081441,10.975));
#37044=CARTESIAN_POINT('',(-0.365,0.476313972081441,10.99));
#37045=CARTESIAN_POINT('',(-0.38,0.476313972081441,10.975));
#37046=CARTESIAN_POINT('Origin',(-0.275,0.476313972081441,10.99));
#37047=CARTESIAN_POINT('Origin',(-0.275,0.476313972081441,11.025));
#37048=CARTESIAN_POINT('',(-0.365,0.476313972081441,11.03));
#37049=CARTESIAN_POINT('',(-0.365,0.476313972081441,11.025));
#37050=CARTESIAN_POINT('Origin',(-0.275,0.476313972081441,11.03));
#37051=CARTESIAN_POINT('Origin',(-0.275,0.476313972081441,11.045));
#37052=CARTESIAN_POINT('',(-0.38,0.476313972081441,11.045));
#37053=CARTESIAN_POINT('Origin',(-0.275,-0.476313972081441,10.975));
#37054=CARTESIAN_POINT('',(-0.365,-0.476313972081441,10.99));
#37055=CARTESIAN_POINT('',(-0.38,-0.476313972081441,10.975));
#37056=CARTESIAN_POINT('Origin',(-0.275,-0.476313972081441,10.99));
#37057=CARTESIAN_POINT('Origin',(-0.275,-0.476313972081441,11.025));
#37058=CARTESIAN_POINT('',(-0.365,-0.476313972081441,11.03));
#37059=CARTESIAN_POINT('',(-0.365,-0.476313972081441,11.025));
#37060=CARTESIAN_POINT('Origin',(-0.275,-0.476313972081441,11.03));
#37061=CARTESIAN_POINT('Origin',(-0.275,-0.476313972081441,11.045));
#37062=CARTESIAN_POINT('',(-0.38,-0.476313972081441,11.045));
#37063=CARTESIAN_POINT('Origin',(0.,0.,11.05));
#37064=CARTESIAN_POINT('',(0.69,8.45006291411674E-17,11.05));
#37065=CARTESIAN_POINT('',(0.,0.,0.));
#37066=CARTESIAN_POINT('Origin',(2.4,0.06,10.91));
#37067=CARTESIAN_POINT('',(2.34923391768466,0.06,10.96));
#37068=CARTESIAN_POINT('',(2.34923391768466,0.06,10.91));
#37069=CARTESIAN_POINT('',(2.34923391768466,0.06,10.935));
#37070=CARTESIAN_POINT('',(2.23,0.06,10.96));
#37071=CARTESIAN_POINT('',(1.30125,0.06,10.96));
#37072=CARTESIAN_POINT('',(2.23,0.06,10.91));
#37073=CARTESIAN_POINT('',(2.23,0.06,10.91));
#37074=CARTESIAN_POINT('',(2.375,0.06,10.91));
#37075=CARTESIAN_POINT('Origin',(2.23,-0.06,10.91));
#37076=CARTESIAN_POINT('',(2.34923391768466,-0.06,10.91));
#37077=CARTESIAN_POINT('',(2.34923391768466,-0.06,10.96));
#37078=CARTESIAN_POINT('',(2.34923391768466,-0.06,10.935));
#37079=CARTESIAN_POINT('',(2.23,-0.06,10.91));
#37080=CARTESIAN_POINT('',(2.29,-0.06,10.91));
#37081=CARTESIAN_POINT('',(2.23,-0.06,10.96));
#37082=CARTESIAN_POINT('',(2.23,-0.06,10.91));
#37083=CARTESIAN_POINT('',(1.21625,-0.06,10.96));
#37084=CARTESIAN_POINT('Origin',(2.23,0.06,10.91));
#37085=CARTESIAN_POINT('',(2.23,0.03,10.91));
#37086=CARTESIAN_POINT('',(2.23,0.03,10.96));
#37087=CARTESIAN_POINT('Origin',(2.35,0.,10.91));
#37088=CARTESIAN_POINT('Origin',(0.,0.,10.91));
#37089=CARTESIAN_POINT('',(-0.185,-0.476313972081441,10.91));
#37090=CARTESIAN_POINT('Origin',(-0.275,-0.476313972081441,10.91));
#37091=CARTESIAN_POINT('',(0.64,1.10218211923262E-17,10.91));
#37092=CARTESIAN_POINT('Origin',(0.55,0.,10.91));
#37093=CARTESIAN_POINT('',(-0.2025,-2.47990976827339E-17,10.91));
#37094=CARTESIAN_POINT('Origin',(0.,0.,10.91));
#37095=CARTESIAN_POINT('',(1.1,0.,10.91));
#37096=CARTESIAN_POINT('',(2.15,0.,10.91));
#37097=CARTESIAN_POINT('',(1.725,0.,10.91));
#37098=CARTESIAN_POINT('',(1.86195461813654,1.075,10.91));
#37099=CARTESIAN_POINT('Origin',(-2.22044604925031E-15,-4.44089209850063E-16,
10.91));
#37100=CARTESIAN_POINT('',(0.952627944162883,0.55,10.91));
#37101=CARTESIAN_POINT('',(1.81222730906827,1.04628992472336,10.91));
#37102=CARTESIAN_POINT('Origin',(-3.33066907387547E-15,-8.88178419700125E-16,
10.91));
#37103=CARTESIAN_POINT('',(0.55,0.952627944162883,10.91));
#37104=CARTESIAN_POINT('',(1.075,1.86195461813654,10.91));
#37105=CARTESIAN_POINT('',(0.56875,0.985103896804799,10.91));
#37106=CARTESIAN_POINT('',(5.55111512312578E-16,2.15,10.91));
#37107=CARTESIAN_POINT('Origin',(-7.25630487348444E-16,-2.1450072913086E-15,
10.91));
#37108=CARTESIAN_POINT('',(2.77555756156289E-16,1.1,10.91));
#37109=CARTESIAN_POINT('',(2.22044604925031E-16,1.075,10.91));
#37110=CARTESIAN_POINT('Origin',(-8.9614946238431E-16,-3.32853323942541E-15,
10.91));
#37111=CARTESIAN_POINT('',(-0.55,0.952627944162883,10.91));
#37112=CARTESIAN_POINT('',(-1.075,1.86195461813654,10.91));
#37113=CARTESIAN_POINT('',(0.0187499999999997,-0.0324759526419162,10.91));
#37114=CARTESIAN_POINT('',(-1.86195461813654,1.075,10.91));
#37115=CARTESIAN_POINT('Origin',(1.49481556190187E-15,-1.70091808145853E-15,
10.91));
#37116=CARTESIAN_POINT('',(-0.952627944162882,0.55,10.91));
#37117=CARTESIAN_POINT('',(-0.0497273090682718,0.0287100752766422,10.91));
#37118=CARTESIAN_POINT('Origin',(2.43451961149116E-15,-2.44035481972528E-15,
10.91));
#37119=CARTESIAN_POINT('',(-1.1,1.66533453693773E-16,10.91));
#37120=CARTESIAN_POINT('',(-2.15,3.33066907387547E-16,10.91));
#37121=CARTESIAN_POINT('',(0.625,-1.20736753927986E-16,10.91));
#37122=CARTESIAN_POINT('',(-1.86195461813654,-1.075,10.91));
#37123=CARTESIAN_POINT('Origin',(2.22044604925031E-15,4.44089209850062E-16,
10.91));
#37124=CARTESIAN_POINT('',(-0.952627944162883,-0.55,10.91));
#37125=CARTESIAN_POINT('',(-0.0497273090682713,-0.0287100752766424,10.91));
#37126=CARTESIAN_POINT('Origin',(3.33066907387547E-15,8.88178419700125E-16,
10.91));
#37127=CARTESIAN_POINT('',(-0.55,-0.952627944162882,10.91));
#37128=CARTESIAN_POINT('',(-1.075,-1.86195461813654,10.91));
#37129=CARTESIAN_POINT('',(0.0187500000000005,0.0324759526419168,10.91));
#37130=CARTESIAN_POINT('',(-1.33226762955019E-15,-2.15,10.91));
#37131=CARTESIAN_POINT('Origin',(7.25630487348445E-16,2.14500729130859E-15,
10.91));
#37132=CARTESIAN_POINT('',(-6.66133814775094E-16,-1.1,10.91));
#37133=CARTESIAN_POINT('',(-6.66133814775094E-16,-1.075,10.91));
#37134=CARTESIAN_POINT('Origin',(8.96149462384311E-16,3.32853323942541E-15,
10.91));
#37135=CARTESIAN_POINT('',(0.549999999999999,-0.952627944162883,10.91));
#37136=CARTESIAN_POINT('',(1.075,-1.86195461813654,10.91));
#37137=CARTESIAN_POINT('',(0.568749999999999,-0.985103896804799,10.91));
#37138=CARTESIAN_POINT('',(1.86195461813654,-1.075,10.91));
#37139=CARTESIAN_POINT('Origin',(-1.49481556190187E-15,1.70091808145853E-15,
10.91));
#37140=CARTESIAN_POINT('',(0.952627944162882,-0.550000000000001,10.91));
#37141=CARTESIAN_POINT('',(1.81222730906827,-1.04628992472336,10.91));
#37142=CARTESIAN_POINT('Origin',(-2.43451961149116E-15,2.44035481972529E-15,
10.91));
#37143=CARTESIAN_POINT('',(-0.185,0.476313972081441,10.91));
#37144=CARTESIAN_POINT('Origin',(-0.275,0.476313972081441,10.91));
#37145=CARTESIAN_POINT('Origin',(0.,0.,10.935));
#37146=CARTESIAN_POINT('Origin',(0.,0.,10.96));
#37147=CARTESIAN_POINT('Origin',(-0.275,-0.476313972081441,10.91));
#37148=CARTESIAN_POINT('',(-0.185,-0.476313972081441,10.96));
#37149=CARTESIAN_POINT('Origin',(-0.275,-0.476313972081441,10.96));
#37150=CARTESIAN_POINT('',(-0.185,-0.476313972081441,10.91));
#37151=CARTESIAN_POINT('Origin',(-0.275,0.476313972081441,10.91));
#37152=CARTESIAN_POINT('',(-0.185,0.476313972081441,10.96));
#37153=CARTESIAN_POINT('Origin',(-0.275,0.476313972081441,10.96));
#37154=CARTESIAN_POINT('',(-0.185,0.476313972081441,10.91));
#37155=CARTESIAN_POINT('Origin',(0.55,0.,10.91));
#37156=CARTESIAN_POINT('',(0.64,-1.10218211923262E-17,10.96));
#37157=CARTESIAN_POINT('Origin',(0.55,0.,10.96));
#37158=CARTESIAN_POINT('',(0.64,-1.10218211923262E-17,10.91));
#37159=CARTESIAN_POINT('Origin',(0.549999999999999,-0.952627944162883,10.91));
#37160=CARTESIAN_POINT('',(0.549999999999999,-0.952627944162883,10.96));
#37161=CARTESIAN_POINT('',(0.549999999999999,-0.952627944162883,10.91));
#37162=CARTESIAN_POINT('',(1.075,-1.86195461813654,10.96));
#37163=CARTESIAN_POINT('',(0.3003125,-0.520156508148029,10.96));
#37164=CARTESIAN_POINT('',(1.075,-1.86195461813654,10.91));
#37165=CARTESIAN_POINT('Origin',(-2.43451961149116E-15,2.44035481972529E-15,
10.91));
#37166=CARTESIAN_POINT('',(0.952627944162882,-0.550000000000001,10.96));
#37167=CARTESIAN_POINT('',(0.952627944162882,-0.550000000000001,10.91));
#37168=CARTESIAN_POINT('Origin',(-2.43451961149116E-15,2.44035481972529E-15,
10.96));
#37169=CARTESIAN_POINT('Origin',(1.86195461813654,-1.075,10.91));
#37170=CARTESIAN_POINT('',(1.86195461813654,-1.075,10.96));
#37171=CARTESIAN_POINT('',(1.86195461813654,-1.075,10.91));
#37172=CARTESIAN_POINT('',(1.00691480906827,-0.581342536066588,10.96));
#37173=CARTESIAN_POINT('Origin',(-1.49481556190187E-15,1.70091808145853E-15,
10.91));
#37174=CARTESIAN_POINT('Origin',(-1.49481556190187E-15,1.70091808145853E-15,
10.96));
#37175=CARTESIAN_POINT('Origin',(-0.55,-0.952627944162882,10.91));
#37176=CARTESIAN_POINT('',(-0.55,-0.952627944162882,10.96));
#37177=CARTESIAN_POINT('',(-0.55,-0.952627944162882,10.91));
#37178=CARTESIAN_POINT('',(-1.075,-1.86195461813654,10.96));
#37179=CARTESIAN_POINT('',(-0.2496875,-0.432471436014854,10.96));
#37180=CARTESIAN_POINT('',(-1.075,-1.86195461813654,10.91));
#37181=CARTESIAN_POINT('Origin',(8.96149462384311E-16,3.32853323942541E-15,
10.91));
#37182=CARTESIAN_POINT('',(-6.66133814775094E-16,-1.1,10.96));
#37183=CARTESIAN_POINT('',(-6.66133814775094E-16,-1.1,10.91));
#37184=CARTESIAN_POINT('Origin',(8.96149462384311E-16,3.32853323942541E-15,
10.96));
#37185=CARTESIAN_POINT('Origin',(-1.33226762955019E-15,-2.15,10.91));
#37186=CARTESIAN_POINT('',(-1.33226762955019E-15,-2.15,10.96));
#37187=CARTESIAN_POINT('',(-1.33226762955019E-15,-2.15,10.91));
#37188=CARTESIAN_POINT('',(-6.10622663543836E-16,-1.075,10.96));
#37189=CARTESIAN_POINT('Origin',(7.25630487348445E-16,2.14500729130859E-15,
10.91));
#37190=CARTESIAN_POINT('Origin',(7.25630487348445E-16,2.14500729130859E-15,
10.96));
#37191=CARTESIAN_POINT('Origin',(-1.1,1.66533453693773E-16,10.91));
#37192=CARTESIAN_POINT('',(-1.1,1.66533453693773E-16,10.96));
#37193=CARTESIAN_POINT('',(-1.1,1.66533453693773E-16,10.91));
#37194=CARTESIAN_POINT('',(-2.15,3.33066907387547E-16,10.96));
#37195=CARTESIAN_POINT('',(-0.44875,5.80785419757035E-17,10.96));
#37196=CARTESIAN_POINT('',(-2.15,3.33066907387547E-16,10.91));
#37197=CARTESIAN_POINT('Origin',(3.33066907387547E-15,8.88178419700125E-16,
10.91));
#37198=CARTESIAN_POINT('',(-0.952627944162883,-0.55,10.96));
#37199=CARTESIAN_POINT('',(-0.952627944162883,-0.55,10.91));
#37200=CARTESIAN_POINT('Origin',(3.33066907387547E-15,8.88178419700125E-16,
10.96));
#37201=CARTESIAN_POINT('Origin',(-1.86195461813654,-1.075,10.91));
#37202=CARTESIAN_POINT('',(-1.86195461813654,-1.075,10.96));
#37203=CARTESIAN_POINT('',(-1.86195461813654,-1.075,10.91));
#37204=CARTESIAN_POINT('',(-0.855039809068272,-0.493657463933413,10.96));
#37205=CARTESIAN_POINT('Origin',(2.22044604925031E-15,4.44089209850062E-16,
10.91));
#37206=CARTESIAN_POINT('Origin',(2.22044604925031E-15,4.44089209850062E-16,
10.96));
#37207=CARTESIAN_POINT('Origin',(-0.55,0.952627944162883,10.91));
#37208=CARTESIAN_POINT('',(-0.55,0.952627944162883,10.96));
#37209=CARTESIAN_POINT('',(-0.55,0.952627944162883,10.91));
#37210=CARTESIAN_POINT('',(-1.075,1.86195461813654,10.96));
#37211=CARTESIAN_POINT('',(-0.2496875,0.432471436014854,10.96));
#37212=CARTESIAN_POINT('',(-1.075,1.86195461813654,10.91));
#37213=CARTESIAN_POINT('Origin',(2.43451961149116E-15,-2.44035481972528E-15,
10.91));
#37214=CARTESIAN_POINT('',(-0.952627944162882,0.55,10.96));
#37215=CARTESIAN_POINT('',(-0.952627944162882,0.55,10.91));
#37216=CARTESIAN_POINT('Origin',(2.43451961149116E-15,-2.44035481972528E-15,
10.96));
#37217=CARTESIAN_POINT('Origin',(-1.86195461813654,1.075,10.91));
#37218=CARTESIAN_POINT('',(-1.86195461813654,1.075,10.96));
#37219=CARTESIAN_POINT('',(-1.86195461813654,1.075,10.91));
#37220=CARTESIAN_POINT('',(-0.855039809068271,0.493657463933413,10.96));
#37221=CARTESIAN_POINT('Origin',(1.49481556190187E-15,-1.70091808145853E-15,
10.91));
#37222=CARTESIAN_POINT('Origin',(1.49481556190187E-15,-1.70091808145853E-15,
10.96));
#37223=CARTESIAN_POINT('Origin',(0.55,0.952627944162883,10.91));
#37224=CARTESIAN_POINT('',(0.55,0.952627944162883,10.96));
#37225=CARTESIAN_POINT('',(0.55,0.952627944162883,10.91));
#37226=CARTESIAN_POINT('',(1.075,1.86195461813654,10.96));
#37227=CARTESIAN_POINT('',(0.3003125,0.520156508148028,10.96));
#37228=CARTESIAN_POINT('',(1.075,1.86195461813654,10.91));
#37229=CARTESIAN_POINT('Origin',(-8.9614946238431E-16,-3.32853323942541E-15,
10.91));
#37230=CARTESIAN_POINT('',(2.77555756156289E-16,1.1,10.96));
#37231=CARTESIAN_POINT('',(2.77555756156289E-16,1.1,10.91));
#37232=CARTESIAN_POINT('Origin',(-8.9614946238431E-16,-3.32853323942541E-15,
10.96));
#37233=CARTESIAN_POINT('Origin',(5.55111512312578E-16,2.15,10.91));
#37234=CARTESIAN_POINT('',(5.55111512312578E-16,2.15,10.96));
#37235=CARTESIAN_POINT('',(5.55111512312578E-16,2.15,10.91));
#37236=CARTESIAN_POINT('',(2.4980018054066E-16,1.075,10.96));
#37237=CARTESIAN_POINT('Origin',(-7.25630487348444E-16,-2.1450072913086E-15,
10.91));
#37238=CARTESIAN_POINT('Origin',(-7.25630487348444E-16,-2.1450072913086E-15,
10.96));
#37239=CARTESIAN_POINT('Origin',(1.1,0.,10.91));
#37240=CARTESIAN_POINT('',(1.1,0.,10.96));
#37241=CARTESIAN_POINT('',(1.1,0.,10.91));
#37242=CARTESIAN_POINT('',(2.15,0.,10.96));
#37243=CARTESIAN_POINT('',(0.65125,0.,10.96));
#37244=CARTESIAN_POINT('',(2.15,0.,10.91));
#37245=CARTESIAN_POINT('Origin',(-3.33066907387547E-15,-8.88178419700125E-16,
10.91));
#37246=CARTESIAN_POINT('',(0.952627944162883,0.55,10.96));
#37247=CARTESIAN_POINT('',(0.952627944162883,0.55,10.91));
#37248=CARTESIAN_POINT('Origin',(-3.33066907387547E-15,-8.88178419700125E-16,
10.96));
#37249=CARTESIAN_POINT('Origin',(1.86195461813654,1.075,10.91));
#37250=CARTESIAN_POINT('',(1.86195461813654,1.075,10.96));
#37251=CARTESIAN_POINT('',(1.86195461813654,1.075,10.91));
#37252=CARTESIAN_POINT('',(1.00691480906827,0.581342536066587,10.96));
#37253=CARTESIAN_POINT('Origin',(-2.22044604925031E-15,-4.44089209850063E-16,
10.91));
#37254=CARTESIAN_POINT('Origin',(-2.22044604925031E-15,-4.44089209850063E-16,
10.96));
#37255=CARTESIAN_POINT('Origin',(0.,0.,10.935));
#37256=CARTESIAN_POINT('',(-0.2025,-2.47990976827339E-17,10.96));
#37257=CARTESIAN_POINT('Origin',(0.,0.,10.96));
#37258=CARTESIAN_POINT('',(-0.2025,-2.47990976827339E-17,10.935));
#37259=CARTESIAN_POINT('Origin',(0.2025,0.,10.96));
#37260=CARTESIAN_POINT('',(0.,0.,0.));
#37261=CARTESIAN_POINT('Origin',(1.46,0.15,-0.305));
#37262=CARTESIAN_POINT('',(1.47,-0.3,-0.315));
#37263=CARTESIAN_POINT('',(1.45,-0.3,-0.295));
#37264=CARTESIAN_POINT('',(1.46,-0.3,-0.305));
#37265=CARTESIAN_POINT('',(1.45,0.3,-0.295));
#37266=CARTESIAN_POINT('',(1.45,0.15,-0.295));
#37267=CARTESIAN_POINT('',(1.47,0.3,-0.315));
#37268=CARTESIAN_POINT('',(1.785,0.3,-0.63));
#37269=CARTESIAN_POINT('',(1.47,0.15,-0.315));
#37270=CARTESIAN_POINT('Origin',(1.45,0.3,-0.315));
#37271=CARTESIAN_POINT('',(1.45,-0.3,-0.17));
#37272=CARTESIAN_POINT('',(1.45,-0.3,-0.315));
#37273=CARTESIAN_POINT('',(1.45,0.3,-0.17));
#37274=CARTESIAN_POINT('',(1.45,0.15,-0.17));
#37275=CARTESIAN_POINT('',(1.45,0.3,-0.315));
#37276=CARTESIAN_POINT('Origin',(1.45,-0.3,-0.315));
#37277=CARTESIAN_POINT('',(2.73,-0.3,-0.315));
#37278=CARTESIAN_POINT('',(1.45,-0.3,-0.315));
#37279=CARTESIAN_POINT('',(2.75,-0.3,-0.335));
#37280=CARTESIAN_POINT('',(2.415,-0.3,1.11022302462516E-16));
#37281=CARTESIAN_POINT('',(2.75,-0.3,0.335));
#37282=CARTESIAN_POINT('',(2.75,-0.3,-0.315));
#37283=CARTESIAN_POINT('',(2.73,-0.3,0.315));
#37284=CARTESIAN_POINT('',(2.2575,-0.3,-0.1575));
#37285=CARTESIAN_POINT('',(1.47,-0.3,0.315));
#37286=CARTESIAN_POINT('',(1.45,-0.3,0.315));
#37287=CARTESIAN_POINT('',(1.45,-0.3,0.295));
#37288=CARTESIAN_POINT('',(1.3025,-0.3,0.1475));
#37289=CARTESIAN_POINT('',(1.45,-0.3,0.17));
#37290=CARTESIAN_POINT('',(1.45,-0.3,-0.315));
#37291=CARTESIAN_POINT('',(1.47,-0.3,0.15));
#37292=CARTESIAN_POINT('',(1.57625,-0.3,0.0437499999999999));
#37293=CARTESIAN_POINT('',(2.43,-0.3,0.15));
#37294=CARTESIAN_POINT('',(1.6875,-0.3,0.15));
#37295=CARTESIAN_POINT('',(2.45,-0.3,0.13));
#37296=CARTESIAN_POINT('',(2.30625,-0.3,0.27375));
#37297=CARTESIAN_POINT('',(2.45,-0.3,-0.13));
#37298=CARTESIAN_POINT('',(2.45,-0.3,-0.2325));
#37299=CARTESIAN_POINT('',(2.43,-0.3,-0.15));
#37300=CARTESIAN_POINT('',(2.14875,-0.3,-0.43125));
#37301=CARTESIAN_POINT('',(1.47,-0.3,-0.15));
#37302=CARTESIAN_POINT('',(1.6875,-0.3,-0.15));
#37303=CARTESIAN_POINT('',(1.41875,-0.3,-0.20125));
#37304=CARTESIAN_POINT('Origin',(1.46,0.15,0.305));
#37305=CARTESIAN_POINT('',(1.47,0.3,0.315));
#37306=CARTESIAN_POINT('',(1.47,0.15,0.315));
#37307=CARTESIAN_POINT('',(1.45,0.3,0.295));
#37308=CARTESIAN_POINT('',(1.6275,0.3,0.4725));
#37309=CARTESIAN_POINT('',(1.45,0.15,0.295));
#37310=CARTESIAN_POINT('Origin',(1.45,0.3,-0.315));
#37311=CARTESIAN_POINT('',(1.45,0.3,0.17));
#37312=CARTESIAN_POINT('',(1.45,0.3,-0.315));
#37313=CARTESIAN_POINT('',(1.45,0.15,0.17));
#37314=CARTESIAN_POINT('Origin',(2.75,0.3,-0.315));
#37315=CARTESIAN_POINT('',(1.47,0.3,-0.15));
#37316=CARTESIAN_POINT('',(1.74375,0.3,0.12375));
#37317=CARTESIAN_POINT('',(2.43,0.3,-0.15));
#37318=CARTESIAN_POINT('',(2.3375,0.3,-0.15));
#37319=CARTESIAN_POINT('',(2.45,0.3,-0.13));
#37320=CARTESIAN_POINT('',(2.47375,0.3,-0.10625));
#37321=CARTESIAN_POINT('',(2.45,0.3,0.13));
#37322=CARTESIAN_POINT('',(2.45,0.3,-0.2325));
#37323=CARTESIAN_POINT('',(2.43,0.3,0.15));
#37324=CARTESIAN_POINT('',(2.63125,0.3,-0.0512499999999997));
#37325=CARTESIAN_POINT('',(1.47,0.3,0.15));
#37326=CARTESIAN_POINT('',(2.3375,0.3,0.15));
#37327=CARTESIAN_POINT('',(1.90125,0.3,-0.28125));
#37328=CARTESIAN_POINT('',(2.73,0.3,0.315));
#37329=CARTESIAN_POINT('',(2.75,0.3,0.315));
#37330=CARTESIAN_POINT('',(2.75,0.3,0.335));
#37331=CARTESIAN_POINT('',(2.5825,0.3,0.1675));
#37332=CARTESIAN_POINT('',(2.75,0.3,-0.335));
#37333=CARTESIAN_POINT('',(2.75,0.3,-0.315));
#37334=CARTESIAN_POINT('',(2.73,0.3,-0.315));
#37335=CARTESIAN_POINT('',(2.74,0.3,-0.325));
#37336=CARTESIAN_POINT('',(2.75,0.3,-0.315));
#37337=CARTESIAN_POINT('Origin',(1.46,0.15,-0.16));
#37338=CARTESIAN_POINT('',(1.47,0.15,-0.15));
#37339=CARTESIAN_POINT('Origin',(1.925,0.,-0.15));
#37340=CARTESIAN_POINT('',(2.43,-0.175,-0.15));
#37341=CARTESIAN_POINT('',(1.65,0.05,-0.15));
#37342=CARTESIAN_POINT('',(1.75,0.05,-0.15));
#37343=CARTESIAN_POINT('',(1.8375,0.05,-0.15));
#37344=CARTESIAN_POINT('',(1.75,-0.05,-0.15));
#37345=CARTESIAN_POINT('',(1.75,-0.025,-0.15));
#37346=CARTESIAN_POINT('',(1.65,-0.05,-0.15));
#37347=CARTESIAN_POINT('',(1.7875,-0.05,-0.15));
#37348=CARTESIAN_POINT('',(1.65,0.025,-0.15));
#37349=CARTESIAN_POINT('Origin',(2.44,-0.175,-0.14));
#37350=CARTESIAN_POINT('',(2.45,-0.175,-0.13));
#37351=CARTESIAN_POINT('Origin',(2.45,-0.35,-0.15));
#37352=CARTESIAN_POINT('',(2.45,-0.175,0.13));
#37353=CARTESIAN_POINT('Origin',(1.46,0.15,0.16));
#37354=CARTESIAN_POINT('',(1.47,0.15,0.15));
#37355=CARTESIAN_POINT('Origin',(1.925,0.,0.15));
#37356=CARTESIAN_POINT('',(2.43,-0.175,0.15));
#37357=CARTESIAN_POINT('',(1.75,0.05,0.15));
#37358=CARTESIAN_POINT('',(1.65,0.05,0.15));
#37359=CARTESIAN_POINT('',(1.8375,0.05,0.15));
#37360=CARTESIAN_POINT('',(1.65,-0.05,0.15));
#37361=CARTESIAN_POINT('',(1.65,0.025,0.15));
#37362=CARTESIAN_POINT('',(1.75,-0.05,0.15));
#37363=CARTESIAN_POINT('',(1.7875,-0.05,0.15));
#37364=CARTESIAN_POINT('',(1.75,-0.025,0.15));
#37365=CARTESIAN_POINT('Origin',(2.44,-0.175,0.14));
#37366=CARTESIAN_POINT('Origin',(2.74,0.35,0.325));
#37367=CARTESIAN_POINT('',(2.75,0.35,0.335));
#37368=CARTESIAN_POINT('',(2.73,0.35,0.315));
#37369=CARTESIAN_POINT('Origin',(2.75,0.7,-0.385));
#37370=CARTESIAN_POINT('',(2.75,0.7,-0.385));
#37371=CARTESIAN_POINT('',(2.75,-0.7,-0.385));
#37372=CARTESIAN_POINT('',(2.75,0.7,-0.385));
#37373=CARTESIAN_POINT('',(2.75,-0.7,0.365));
#37374=CARTESIAN_POINT('',(2.75,-0.7,-0.385));
#37375=CARTESIAN_POINT('',(2.75,0.7,0.365));
#37376=CARTESIAN_POINT('',(2.75,0.7,0.365));
#37377=CARTESIAN_POINT('',(2.75,0.7,-0.385));
#37378=CARTESIAN_POINT('',(2.75,0.61,1.10218211923262E-17));
#37379=CARTESIAN_POINT('Origin',(2.75,0.52,0.));
#37380=CARTESIAN_POINT('',(2.75,-0.43,1.10218211923262E-17));
#37381=CARTESIAN_POINT('Origin',(2.75,-0.52,0.));
#37382=CARTESIAN_POINT('',(2.75,0.35,-0.335));
#37383=CARTESIAN_POINT('Origin',(2.74,0.35,-0.325));
#37384=CARTESIAN_POINT('',(2.73,0.35,-0.315));
#37385=CARTESIAN_POINT('Origin',(2.1,0.,-0.315));
#37386=CARTESIAN_POINT('Origin',(2.805,-0.52,0.));
#37387=CARTESIAN_POINT('',(2.91,-0.43,-1.10218211923262E-17));
#37388=CARTESIAN_POINT('Origin',(2.91,-0.52,0.));
#37389=CARTESIAN_POINT('',(2.805,-0.43,-1.10218211923262E-17));
#37390=CARTESIAN_POINT('Origin',(2.805,0.52,0.));
#37391=CARTESIAN_POINT('',(2.91,0.61,-1.10218211923262E-17));
#37392=CARTESIAN_POINT('Origin',(2.91,0.52,0.));
#37393=CARTESIAN_POINT('',(2.805,0.61,-1.10218211923262E-17));
#37394=CARTESIAN_POINT('Origin',(2.91,0.7,-0.385));
#37395=CARTESIAN_POINT('',(2.91,0.7,-0.385));
#37396=CARTESIAN_POINT('',(2.91,0.7,-0.385));
#37397=CARTESIAN_POINT('',(2.91,0.7,0.365));
#37398=CARTESIAN_POINT('',(2.91,0.7,0.365));
#37399=CARTESIAN_POINT('',(2.91,0.7,-0.385));
#37400=CARTESIAN_POINT('Origin',(2.91,-0.7,-0.385));
#37401=CARTESIAN_POINT('',(2.91,-0.7,-0.385));
#37402=CARTESIAN_POINT('',(2.91,-0.7,-0.385));
#37403=CARTESIAN_POINT('',(2.91,-0.7,0.365));
#37404=CARTESIAN_POINT('',(2.91,-0.7,0.365));
#37405=CARTESIAN_POINT('',(2.91,-0.7,-0.385));
#37406=CARTESIAN_POINT('Origin',(2.75,-0.7,-0.385));
#37407=CARTESIAN_POINT('',(2.75,-0.7,-0.385));
#37408=CARTESIAN_POINT('',(2.75,-0.7,0.365));
#37409=CARTESIAN_POINT('Origin',(2.83,0.,0.365));
#37410=CARTESIAN_POINT('Origin',(2.83,0.,-0.385));
#37411=CARTESIAN_POINT('Origin',(1.75,0.05,-0.19));
#37412=CARTESIAN_POINT('',(1.75,0.05,-0.19));
#37413=CARTESIAN_POINT('',(1.65,0.05,-0.19));
#37414=CARTESIAN_POINT('',(1.75,0.05,-0.19));
#37415=CARTESIAN_POINT('',(1.75,0.05,-0.19));
#37416=CARTESIAN_POINT('',(1.65,0.05,-0.19));
#37417=CARTESIAN_POINT('Origin',(1.75,-0.05,-0.19));
#37418=CARTESIAN_POINT('',(1.75,-0.05,-0.19));
#37419=CARTESIAN_POINT('',(1.75,-0.05,-0.19));
#37420=CARTESIAN_POINT('',(1.75,-0.05,-0.19));
#37421=CARTESIAN_POINT('Origin',(1.65,-0.05,-0.19));
#37422=CARTESIAN_POINT('',(1.65,-0.05,-0.19));
#37423=CARTESIAN_POINT('',(1.65,-0.05,-0.19));
#37424=CARTESIAN_POINT('',(1.65,-0.05,-0.19));
#37425=CARTESIAN_POINT('Origin',(1.65,0.05,-0.19));
#37426=CARTESIAN_POINT('',(1.65,0.05,-0.19));
#37427=CARTESIAN_POINT('Origin',(1.7,0.,-0.19));
#37428=CARTESIAN_POINT('Origin',(1.75,0.05,0.15));
#37429=CARTESIAN_POINT('',(1.75,0.05,0.19));
#37430=CARTESIAN_POINT('',(1.75,0.05,0.15));
#37431=CARTESIAN_POINT('',(1.65,0.05,0.19));
#37432=CARTESIAN_POINT('',(1.75,0.05,0.19));
#37433=CARTESIAN_POINT('',(1.65,0.05,0.15));
#37434=CARTESIAN_POINT('Origin',(1.75,-0.05,0.15));
#37435=CARTESIAN_POINT('',(1.75,-0.05,0.19));
#37436=CARTESIAN_POINT('',(1.75,-0.05,0.15));
#37437=CARTESIAN_POINT('',(1.75,-0.05,0.19));
#37438=CARTESIAN_POINT('Origin',(1.65,-0.05,0.15));
#37439=CARTESIAN_POINT('',(1.65,-0.05,0.19));
#37440=CARTESIAN_POINT('',(1.65,-0.05,0.15));
#37441=CARTESIAN_POINT('',(1.65,-0.05,0.19));
#37442=CARTESIAN_POINT('Origin',(1.65,0.05,0.15));
#37443=CARTESIAN_POINT('',(1.65,0.05,0.19));
#37444=CARTESIAN_POINT('Origin',(1.7,0.,0.19));
#37445=CARTESIAN_POINT('Origin',(2.1,0.,0.315));
#37446=CARTESIAN_POINT('',(0.,0.,0.));
#37447=CARTESIAN_POINT('Origin',(3.55,-0.35,-0.535));
#37448=CARTESIAN_POINT('',(3.7,-0.35,-0.385));
#37449=CARTESIAN_POINT('',(3.55,-0.5,-0.385));
#37450=CARTESIAN_POINT('Origin',(3.55,-0.35,-0.385));
#37451=CARTESIAN_POINT('',(3.55,-0.5,-0.535));
#37452=CARTESIAN_POINT('',(3.55,-0.5,-0.535));
#37453=CARTESIAN_POINT('',(3.7,-0.35,-0.535));
#37454=CARTESIAN_POINT('Origin',(3.55,-0.35,-0.535));
#37455=CARTESIAN_POINT('',(3.7,-0.35,-0.535));
#37456=CARTESIAN_POINT('Origin',(3.38,0.,-0.385));
#37457=CARTESIAN_POINT('',(3.7,0.35,-0.385));
#37458=CARTESIAN_POINT('',(3.7,-0.5,-0.385));
#37459=CARTESIAN_POINT('',(3.55,0.5,-0.385));
#37460=CARTESIAN_POINT('Origin',(3.55,0.35,-0.385));
#37461=CARTESIAN_POINT('',(3.12,0.5,-0.385));
#37462=CARTESIAN_POINT('',(3.7,0.5,-0.385));
#37463=CARTESIAN_POINT('',(3.12,0.120933866224478,-0.385));
#37464=CARTESIAN_POINT('',(3.12,-0.35,-0.385));
#37465=CARTESIAN_POINT('',(3.2,0.145,-0.385));
#37466=CARTESIAN_POINT('Origin',(3.2,0.,-0.385));
#37467=CARTESIAN_POINT('',(3.5,0.145,-0.385));
#37468=CARTESIAN_POINT('',(3.29,0.145,-0.385));
#37469=CARTESIAN_POINT('',(3.5,-0.145,-0.385));
#37470=CARTESIAN_POINT('Origin',(3.5,-1.38777878078145E-17,-0.385));
#37471=CARTESIAN_POINT('',(3.2,-0.145,-0.385));
#37472=CARTESIAN_POINT('',(3.44,-0.145,-0.385));
#37473=CARTESIAN_POINT('',(3.12,-0.120933866224478,-0.385));
#37474=CARTESIAN_POINT('Origin',(3.2,0.,-0.385));
#37475=CARTESIAN_POINT('',(3.12,-0.5,-0.385));
#37476=CARTESIAN_POINT('',(3.12,-0.35,-0.385));
#37477=CARTESIAN_POINT('',(3.06,-0.5,-0.385));
#37478=CARTESIAN_POINT('Origin',(3.7,-0.5,-0.535));
#37479=CARTESIAN_POINT('',(3.7,0.35,-0.535));
#37480=CARTESIAN_POINT('',(3.7,-0.5,-0.535));
#37481=CARTESIAN_POINT('',(3.7,0.35,-0.535));
#37482=CARTESIAN_POINT('Origin',(3.55,0.35,-0.535));
#37483=CARTESIAN_POINT('',(3.55,0.5,-0.535));
#37484=CARTESIAN_POINT('Origin',(3.55,0.35,-0.535));
#37485=CARTESIAN_POINT('',(3.55,0.5,-0.535));
#37486=CARTESIAN_POINT('Origin',(2.985,-0.52,0.));
#37487=CARTESIAN_POINT('',(3.06,-0.435,-1.04094977927525E-17));
#37488=CARTESIAN_POINT('Origin',(3.06,-0.52,0.));
#37489=CARTESIAN_POINT('',(2.91,-0.435,1.04094977927525E-17));
#37490=CARTESIAN_POINT('',(2.985,-0.435,-1.04094977927525E-17));
#37491=CARTESIAN_POINT('Origin',(2.91,-0.52,0.));
#37492=CARTESIAN_POINT('Origin',(2.985,0.52,0.));
#37493=CARTESIAN_POINT('',(3.06,0.605,-1.04094977927525E-17));
#37494=CARTESIAN_POINT('Origin',(3.06,0.52,0.));
#37495=CARTESIAN_POINT('',(2.91,0.605,1.04094977927525E-17));
#37496=CARTESIAN_POINT('',(2.985,0.605,-1.04094977927525E-17));
#37497=CARTESIAN_POINT('Origin',(2.91,0.52,0.));
#37498=CARTESIAN_POINT('Origin',(3.5,-0.145,-0.385));
#37499=CARTESIAN_POINT('',(3.5,-0.145,-0.535));
#37500=CARTESIAN_POINT('',(3.5,-0.145,-0.385));
#37501=CARTESIAN_POINT('',(3.2,-0.145,-0.535));
#37502=CARTESIAN_POINT('',(3.2425,-0.145,-0.535));
#37503=CARTESIAN_POINT('',(3.2,-0.145,-0.385));
#37504=CARTESIAN_POINT('Origin',(3.5,-1.38777878078145E-17,-0.385));
#37505=CARTESIAN_POINT('',(3.5,0.145,-0.535));
#37506=CARTESIAN_POINT('',(3.5,0.145,-0.385));
#37507=CARTESIAN_POINT('Origin',(3.5,-1.38777878078145E-17,-0.535));
#37508=CARTESIAN_POINT('Origin',(3.2,0.145,-0.385));
#37509=CARTESIAN_POINT('',(3.2,0.145,-0.535));
#37510=CARTESIAN_POINT('',(3.2,0.145,-0.385));
#37511=CARTESIAN_POINT('',(3.0925,0.145,-0.535));
#37512=CARTESIAN_POINT('Origin',(3.2,0.,-0.385));
#37513=CARTESIAN_POINT('Origin',(3.2,0.,-0.385));
#37514=CARTESIAN_POINT('Origin',(3.2,0.,-0.535));
#37515=CARTESIAN_POINT('Origin',(3.35,0.,-0.385));
#37516=CARTESIAN_POINT('',(3.12,-0.35,-0.385));
#37517=CARTESIAN_POINT('Origin',(3.12,-0.35,-0.325));
#37518=CARTESIAN_POINT('',(3.06,-0.5,-0.325));
#37519=CARTESIAN_POINT('Origin',(3.12,-0.5,-0.325));
#37520=CARTESIAN_POINT('',(3.06,0.5,-0.325));
#37521=CARTESIAN_POINT('Origin',(3.12,0.5,-0.325));
#37522=CARTESIAN_POINT('',(3.06,-0.35,-0.325));
#37523=CARTESIAN_POINT('Origin',(3.7,0.5,-0.535));
#37524=CARTESIAN_POINT('',(3.06,0.5,-0.535));
#37525=CARTESIAN_POINT('',(3.7,0.5,-0.535));
#37526=CARTESIAN_POINT('',(3.06,0.5,-0.535));
#37527=CARTESIAN_POINT('Origin',(3.06,-0.5,-0.535));
#37528=CARTESIAN_POINT('',(3.06,-0.5,-0.535));
#37529=CARTESIAN_POINT('',(3.06,-0.5,-0.535));
#37530=CARTESIAN_POINT('',(3.06,-0.5,-0.535));
#37531=CARTESIAN_POINT('Origin',(3.06,0.7,-0.535));
#37532=CARTESIAN_POINT('',(3.06,0.7,-0.535));
#37533=CARTESIAN_POINT('',(2.91,0.7,-0.535));
#37534=CARTESIAN_POINT('',(3.06,0.7,-0.535));
#37535=CARTESIAN_POINT('',(2.91,0.7,0.365));
#37536=CARTESIAN_POINT('',(2.91,0.7,-0.535));
#37537=CARTESIAN_POINT('',(3.06,0.7,0.365));
#37538=CARTESIAN_POINT('',(3.06,0.7,0.365));
#37539=CARTESIAN_POINT('',(3.06,0.7,-0.535));
#37540=CARTESIAN_POINT('Origin',(3.06,-0.7,-0.535));
#37541=CARTESIAN_POINT('',(3.06,-0.7,-0.535));
#37542=CARTESIAN_POINT('',(3.06,-0.7,0.365));
#37543=CARTESIAN_POINT('',(3.06,-0.7,0.365));
#37544=CARTESIAN_POINT('',(3.06,-0.7,-0.535));
#37545=CARTESIAN_POINT('',(3.06,-0.7,-0.535));
#37546=CARTESIAN_POINT('',(3.06,-0.7,-0.535));
#37547=CARTESIAN_POINT('Origin',(2.91,-0.7,-0.535));
#37548=CARTESIAN_POINT('',(2.91,-0.7,-0.535));
#37549=CARTESIAN_POINT('',(2.91,-0.7,-0.535));
#37550=CARTESIAN_POINT('',(2.91,-0.7,0.365));
#37551=CARTESIAN_POINT('',(2.91,-0.7,0.365));
#37552=CARTESIAN_POINT('',(2.91,-0.7,-0.535));
#37553=CARTESIAN_POINT('Origin',(2.91,0.7,-0.535));
#37554=CARTESIAN_POINT('',(2.91,0.7,-0.535));
#37555=CARTESIAN_POINT('',(2.91,0.7,0.365));
#37556=CARTESIAN_POINT('Origin',(2.985,0.,0.365));
#37557=CARTESIAN_POINT('Origin',(2.985,0.,-0.535));
#37558=CARTESIAN_POINT('',(0.,0.,0.));
#37559=CARTESIAN_POINT('Origin',(2.4,0.9,3.16));
#37560=CARTESIAN_POINT('',(1.8,0.9,3.16));
#37561=CARTESIAN_POINT('',(2.4,0.9,3.16));
#37562=CARTESIAN_POINT('',(1.6,0.9,3.16));
#37563=CARTESIAN_POINT('',(1.8,0.9,3.46));
#37564=CARTESIAN_POINT('',(1.8,0.9,3.16));
#37565=CARTESIAN_POINT('',(2.4,0.9,3.46));
#37566=CARTESIAN_POINT('',(2.4,0.9,3.46));
#37567=CARTESIAN_POINT('',(2.4,0.9,3.16));
#37568=CARTESIAN_POINT('Origin',(2.4,0.6,3.16));
#37569=CARTESIAN_POINT('',(2.4,0.6,3.16));
#37570=CARTESIAN_POINT('',(2.4,0.3,3.16));
#37571=CARTESIAN_POINT('',(2.4,0.6,3.46));
#37572=CARTESIAN_POINT('',(2.4,0.6,3.46));
#37573=CARTESIAN_POINT('',(2.4,0.6,3.16));
#37574=CARTESIAN_POINT('Origin',(1.8,0.6,3.16));
#37575=CARTESIAN_POINT('',(1.8,0.6,3.16));
#37576=CARTESIAN_POINT('',(1.3,0.6,3.16));
#37577=CARTESIAN_POINT('',(1.8,0.6,3.46));
#37578=CARTESIAN_POINT('',(1.8,0.6,3.46));
#37579=CARTESIAN_POINT('',(1.8,0.6,3.16));
#37580=CARTESIAN_POINT('Origin',(1.8,0.9,3.16));
#37581=CARTESIAN_POINT('',(1.8,0.45,3.16));
#37582=CARTESIAN_POINT('',(1.8,0.9,3.46));
#37583=CARTESIAN_POINT('Origin',(2.1,0.75,3.46));
#37584=CARTESIAN_POINT('Origin',(0.3,-2.6,3.16));
#37585=CARTESIAN_POINT('',(-0.9,-2.6,3.16));
#37586=CARTESIAN_POINT('',(0.3,-2.6,3.16));
#37587=CARTESIAN_POINT('',(0.55,-2.6,3.16));
#37588=CARTESIAN_POINT('',(-0.9,-2.6,3.76));
#37589=CARTESIAN_POINT('',(-0.9,-2.6,3.16));
#37590=CARTESIAN_POINT('',(0.3,-2.6,3.76));
#37591=CARTESIAN_POINT('',(0.3,-2.6,3.76));
#37592=CARTESIAN_POINT('',(0.3,-2.6,3.16));
#37593=CARTESIAN_POINT('Origin',(0.3,-3.2,3.16));
#37594=CARTESIAN_POINT('',(0.3,-3.2,3.16));
#37595=CARTESIAN_POINT('',(0.3,-1.6,3.16));
#37596=CARTESIAN_POINT('',(0.3,-3.2,3.76));
#37597=CARTESIAN_POINT('',(0.3,-3.2,3.76));
#37598=CARTESIAN_POINT('',(0.3,-3.2,3.16));
#37599=CARTESIAN_POINT('Origin',(-0.9,-3.2,3.16));
#37600=CARTESIAN_POINT('',(-0.9,-3.2,3.16));
#37601=CARTESIAN_POINT('',(-0.0500000000000001,-3.2,3.16));
#37602=CARTESIAN_POINT('',(-0.9,-3.2,3.76));
#37603=CARTESIAN_POINT('',(-0.9,-3.2,3.76));
#37604=CARTESIAN_POINT('',(-0.9,-3.2,3.16));
#37605=CARTESIAN_POINT('Origin',(-0.9,-2.6,3.16));
#37606=CARTESIAN_POINT('',(-0.9,-1.3,3.16));
#37607=CARTESIAN_POINT('',(-0.9,-2.6,3.76));
#37608=CARTESIAN_POINT('Origin',(-0.3,-2.9,3.76));
#37609=CARTESIAN_POINT('Origin',(2.,-1.,3.16));
#37610=CARTESIAN_POINT('',(1.7,-1.,3.86));
#37611=CARTESIAN_POINT('Origin',(2.,-1.,3.86));
#37612=CARTESIAN_POINT('',(1.7,-1.,3.16));
#37613=CARTESIAN_POINT('',(1.7,-1.,3.16));
#37614=CARTESIAN_POINT('Origin',(2.,-1.,3.16));
#37615=CARTESIAN_POINT('Origin',(2.,-1.,3.86));
#37616=CARTESIAN_POINT('Origin',(-0.5,2.4,3.16));
#37617=CARTESIAN_POINT('',(-1.,2.4,3.16));
#37618=CARTESIAN_POINT('',(-0.5,2.4,3.16));
#37619=CARTESIAN_POINT('',(0.15,2.4,3.16));
#37620=CARTESIAN_POINT('',(-1.,2.4,3.31));
#37621=CARTESIAN_POINT('',(-1.,2.4,3.16));
#37622=CARTESIAN_POINT('',(-0.5,2.4,3.31));
#37623=CARTESIAN_POINT('',(-0.5,2.4,3.31));
#37624=CARTESIAN_POINT('',(-0.5,2.4,3.16));
#37625=CARTESIAN_POINT('Origin',(-0.5,1.8,3.16));
#37626=CARTESIAN_POINT('',(-0.5,1.8,3.16));
#37627=CARTESIAN_POINT('',(-0.5,0.9,3.16));
#37628=CARTESIAN_POINT('',(-0.5,1.8,3.31));
#37629=CARTESIAN_POINT('',(-0.5,1.8,3.31));
#37630=CARTESIAN_POINT('',(-0.5,1.8,3.16));
#37631=CARTESIAN_POINT('Origin',(-1.,1.8,3.16));
#37632=CARTESIAN_POINT('',(-1.,1.8,3.16));
#37633=CARTESIAN_POINT('',(-0.1,1.8,3.16));
#37634=CARTESIAN_POINT('',(-1.,1.8,3.31));
#37635=CARTESIAN_POINT('',(-1.,1.8,3.31));
#37636=CARTESIAN_POINT('',(-1.,1.8,3.16));
#37637=CARTESIAN_POINT('Origin',(-1.,2.4,3.16));
#37638=CARTESIAN_POINT('',(-1.,1.2,3.16));
#37639=CARTESIAN_POINT('',(-1.,2.4,3.31));
#37640=CARTESIAN_POINT('Origin',(-0.75,2.1,3.31));
#37641=CARTESIAN_POINT('Origin',(-1.3,0.3,3.16));
#37642=CARTESIAN_POINT('',(-1.8,0.3,3.16));
#37643=CARTESIAN_POINT('',(-1.3,0.3,3.16));
#37644=CARTESIAN_POINT('',(-0.25,0.3,3.16));
#37645=CARTESIAN_POINT('',(-1.8,0.3,3.31));
#37646=CARTESIAN_POINT('',(-1.8,0.3,3.16));
#37647=CARTESIAN_POINT('',(-1.3,0.3,3.31));
#37648=CARTESIAN_POINT('',(-1.3,0.3,3.31));
#37649=CARTESIAN_POINT('',(-1.3,0.3,3.16));
#37650=CARTESIAN_POINT('Origin',(-1.3,-0.3,3.16));
#37651=CARTESIAN_POINT('',(-1.3,-0.3,3.16));
#37652=CARTESIAN_POINT('',(-1.3,-0.15,3.16));
#37653=CARTESIAN_POINT('',(-1.3,-0.3,3.31));
#37654=CARTESIAN_POINT('',(-1.3,-0.3,3.31));
#37655=CARTESIAN_POINT('',(-1.3,-0.3,3.16));
#37656=CARTESIAN_POINT('Origin',(-1.8,-0.3,3.16));
#37657=CARTESIAN_POINT('',(-1.8,-0.3,3.16));
#37658=CARTESIAN_POINT('',(-0.5,-0.3,3.16));
#37659=CARTESIAN_POINT('',(-1.8,-0.3,3.31));
#37660=CARTESIAN_POINT('',(-1.8,-0.3,3.31));
#37661=CARTESIAN_POINT('',(-1.8,-0.3,3.16));
#37662=CARTESIAN_POINT('Origin',(-1.8,0.3,3.16));
#37663=CARTESIAN_POINT('',(-1.8,0.15,3.16));
#37664=CARTESIAN_POINT('',(-1.8,0.3,3.31));
#37665=CARTESIAN_POINT('Origin',(-1.55,0.,3.31));
#37666=CARTESIAN_POINT('Origin',(-1.3,1.2,3.16));
#37667=CARTESIAN_POINT('',(-1.8,1.2,3.16));
#37668=CARTESIAN_POINT('',(-1.3,1.2,3.16));
#37669=CARTESIAN_POINT('',(-0.25,1.2,3.16));
#37670=CARTESIAN_POINT('',(-1.8,1.2,3.31));
#37671=CARTESIAN_POINT('',(-1.8,1.2,3.16));
#37672=CARTESIAN_POINT('',(-1.3,1.2,3.31));
#37673=CARTESIAN_POINT('',(-1.3,1.2,3.31));
#37674=CARTESIAN_POINT('',(-1.3,1.2,3.16));
#37675=CARTESIAN_POINT('Origin',(-1.3,0.6,3.16));
#37676=CARTESIAN_POINT('',(-1.3,0.6,3.16));
#37677=CARTESIAN_POINT('',(-1.3,0.3,3.16));
#37678=CARTESIAN_POINT('',(-1.3,0.6,3.31));
#37679=CARTESIAN_POINT('',(-1.3,0.6,3.31));
#37680=CARTESIAN_POINT('',(-1.3,0.6,3.16));
#37681=CARTESIAN_POINT('Origin',(-1.8,0.6,3.16));
#37682=CARTESIAN_POINT('',(-1.8,0.6,3.16));
#37683=CARTESIAN_POINT('',(-0.5,0.6,3.16));
#37684=CARTESIAN_POINT('',(-1.8,0.6,3.31));
#37685=CARTESIAN_POINT('',(-1.8,0.6,3.31));
#37686=CARTESIAN_POINT('',(-1.8,0.6,3.16));
#37687=CARTESIAN_POINT('Origin',(-1.8,1.2,3.16));
#37688=CARTESIAN_POINT('',(-1.8,0.6,3.16));
#37689=CARTESIAN_POINT('',(-1.8,1.2,3.31));
#37690=CARTESIAN_POINT('Origin',(-1.55,0.9,3.31));
#37691=CARTESIAN_POINT('Origin',(1.6,1.6,3.16));
#37692=CARTESIAN_POINT('',(0.8,1.6,3.16));
#37693=CARTESIAN_POINT('',(1.6,1.6,3.16));
#37694=CARTESIAN_POINT('',(1.2,1.6,3.16));
#37695=CARTESIAN_POINT('',(0.8,1.6,3.28));
#37696=CARTESIAN_POINT('',(0.8,1.6,3.16));
#37697=CARTESIAN_POINT('',(1.6,1.6,3.28));
#37698=CARTESIAN_POINT('',(1.6,1.6,3.28));
#37699=CARTESIAN_POINT('',(1.6,1.6,3.16));
#37700=CARTESIAN_POINT('Origin',(1.6,0.8,3.16));
#37701=CARTESIAN_POINT('',(1.6,0.8,3.16));
#37702=CARTESIAN_POINT('',(1.6,0.4,3.16));
#37703=CARTESIAN_POINT('',(1.6,0.8,3.28));
#37704=CARTESIAN_POINT('',(1.6,0.8,3.28));
#37705=CARTESIAN_POINT('',(1.6,0.8,3.16));
#37706=CARTESIAN_POINT('Origin',(0.8,0.8,3.16));
#37707=CARTESIAN_POINT('',(0.8,0.8,3.16));
#37708=CARTESIAN_POINT('',(0.8,0.8,3.16));
#37709=CARTESIAN_POINT('',(0.8,0.8,3.28));
#37710=CARTESIAN_POINT('',(0.8,0.8,3.28));
#37711=CARTESIAN_POINT('',(0.8,0.8,3.16));
#37712=CARTESIAN_POINT('Origin',(0.8,1.6,3.16));
#37713=CARTESIAN_POINT('',(0.8,0.8,3.16));
#37714=CARTESIAN_POINT('',(0.8,1.6,3.28));
#37715=CARTESIAN_POINT('Origin',(1.2,1.2,3.28));
#37716=CARTESIAN_POINT('Origin',(2.94448637286709,-1.7,3.085));
#37717=CARTESIAN_POINT('',(2.80948637286709,-1.7,3.));
#37718=CARTESIAN_POINT('Origin',(2.94448637286709,-1.7,3.));
#37719=CARTESIAN_POINT('',(2.80948637286709,-1.7,3.16));
#37720=CARTESIAN_POINT('',(2.80948637286709,-1.7,3.085));
#37721=CARTESIAN_POINT('Origin',(2.94448637286709,-1.7,3.16));
#37722=CARTESIAN_POINT('Origin',(-2.94448637286709,-1.7,3.085));
#37723=CARTESIAN_POINT('',(-3.07948637286709,-1.7,3.));
#37724=CARTESIAN_POINT('Origin',(-2.94448637286709,-1.7,3.));
#37725=CARTESIAN_POINT('',(-3.07948637286709,-1.7,3.16));
#37726=CARTESIAN_POINT('',(-3.07948637286709,-1.7,3.085));
#37727=CARTESIAN_POINT('Origin',(-2.94448637286709,-1.7,3.16));
#37728=CARTESIAN_POINT('Origin',(2.0818995585505E-16,3.4,3.085));
#37729=CARTESIAN_POINT('',(-0.135,3.4,3.));
#37730=CARTESIAN_POINT('Origin',(2.0818995585505E-16,3.4,3.));
#37731=CARTESIAN_POINT('',(-0.135,3.4,3.16));
#37732=CARTESIAN_POINT('',(-0.135,3.4,3.085));
#37733=CARTESIAN_POINT('Origin',(2.0818995585505E-16,3.4,3.16));
#37734=CARTESIAN_POINT('Origin',(0.,0.,3.08));
#37735=CARTESIAN_POINT('',(-0.8,-9.79717439317883E-17,3.16));
#37736=CARTESIAN_POINT('Origin',(0.,0.,3.16));
#37737=CARTESIAN_POINT('',(-0.8,-9.79717439317883E-17,3.));
#37738=CARTESIAN_POINT('',(-0.8,-9.79717439317883E-17,3.08));
#37739=CARTESIAN_POINT('Origin',(0.,0.,3.));
#37740=CARTESIAN_POINT('Origin',(3.8,0.,3.));
#37741=CARTESIAN_POINT('',(-3.8,-4.65365783675994E-16,3.));
#37742=CARTESIAN_POINT('Origin',(0.,0.,3.));
#37743=CARTESIAN_POINT('Origin',(0.,0.,3.08));
#37744=CARTESIAN_POINT('',(-3.8,-4.65365783675994E-16,3.16));
#37745=CARTESIAN_POINT('Origin',(0.,0.,3.16));
#37746=CARTESIAN_POINT('',(-3.8,-4.65365783675994E-16,3.08));
#37747=CARTESIAN_POINT('Origin',(0.8,0.,3.16));
#37748=CARTESIAN_POINT('',(0.,0.,0.));
#37749=CARTESIAN_POINT('Origin',(0.,0.,0.1025));
#37750=CARTESIAN_POINT('',(-0.0966658713741579,-8.30033664664526E-5,0.0751277583556343));
#37751=CARTESIAN_POINT('',(-0.0966485063039693,-8.22854894029733E-5,0.0693305749776991));
#37752=CARTESIAN_POINT('',(-0.096675,-1.1839272930757E-17,0.1025));
#37753=CARTESIAN_POINT('',(-0.0965779349718935,5.35477908776769E-5,0.0351277583556343));
#37754=CARTESIAN_POINT('Ctrl Pts',(-0.0966658713741579,-8.30033664664526E-5,
0.0751277583556343));
#37755=CARTESIAN_POINT('Ctrl Pts',(-0.0964554816322757,0.0239708948875215,
0.0735437011748551));
#37756=CARTESIAN_POINT('Ctrl Pts',(-0.0873429088905798,0.048167382154486,
0.0719596439940758));
#37757=CARTESIAN_POINT('Ctrl Pts',(-0.071078953014767,0.0657492986486455,
0.0703755868132966));
#37758=CARTESIAN_POINT('Ctrl Pts',(-0.0496033408668211,0.0889652014910574,
0.0682839310135428));
#37759=CARTESIAN_POINT('Ctrl Pts',(-0.015658810541703,0.100648154665348,
0.0661922752137891));
#37760=CARTESIAN_POINT('Ctrl Pts',(0.0155551384254827,0.0955677385731121,
0.0641006194140353));
#37761=CARTESIAN_POINT('Ctrl Pts',(0.0467690873926682,0.0904873224808759,
0.0620089636142815));
#37762=CARTESIAN_POINT('Ctrl Pts',(0.0752524550019215,0.0686435371221129,
0.0599173078145278));
#37763=CARTESIAN_POINT('Ctrl Pts',(0.0882585289492488,0.0398157711278956,
0.057825652014774));
#37764=CARTESIAN_POINT('Ctrl Pts',(0.101264602896576,0.010988005133678,
0.0557339962150202));
#37765=CARTESIAN_POINT('Ctrl Pts',(0.0987933831819777,-0.024823741495994,
0.0536423404152665));
#37766=CARTESIAN_POINT('Ctrl Pts',(0.0819414258178345,-0.0515867990200962,
0.0515506846155127));
#37767=CARTESIAN_POINT('Ctrl Pts',(0.0650894684536913,-0.0783498565441982,
0.049459028815759));
#37768=CARTESIAN_POINT('Ctrl Pts',(0.0338567734400037,-0.0960642249627305,
0.0473673730160052));
#37769=CARTESIAN_POINT('Ctrl Pts',(0.00224472816243995,-0.0967991363303525,
0.0452757172162514));
#37770=CARTESIAN_POINT('Ctrl Pts',(-0.0293673171151238,-0.0975340476979745,
0.0431840614164977));
#37771=CARTESIAN_POINT('Ctrl Pts',(-0.0613587126565637,-0.0812895020146863,
0.0410924056167439));
#37772=CARTESIAN_POINT('Ctrl Pts',(-0.079442849947587,-0.0553384044193135,
0.0390007498169901));
#37773=CARTESIAN_POINT('Ctrl Pts',(-0.0906046146003188,-0.0393210495862792,
0.0377097526632049));
#37774=CARTESIAN_POINT('Ctrl Pts',(-0.096468382952661,-0.0196059654673,
0.0364187555094196));
#37775=CARTESIAN_POINT('Ctrl Pts',(-0.0965779349718935,5.35477908776769E-5,
0.0351277583556343));
#37776=CARTESIAN_POINT('',(-0.096675,-1.1839272930757E-17,0.0222291666666667));
#37777=CARTESIAN_POINT('',(-0.096675,-1.1839272930757E-17,0.1025));
#37778=CARTESIAN_POINT('Origin',(0.,0.,0.0222291666666667));
#37779=CARTESIAN_POINT('',(-0.0929420004886496,0.02708977403664,0.033325));
#37780=CARTESIAN_POINT('Ctrl Pts',(-0.0965779349718935,5.35477908776769E-5,
0.0351277583556343));
#37781=CARTESIAN_POINT('Ctrl Pts',(-0.0966289280659962,0.00920444630111537,
0.0345268389037562));
#37782=CARTESIAN_POINT('Ctrl Pts',(-0.095433203415953,0.0183433047394809,
0.0339259194518781));
#37783=CARTESIAN_POINT('Ctrl Pts',(-0.0929447515460691,0.0270916053744145,
0.033325));
#37784=CARTESIAN_POINT('',(-0.0782614497120755,-0.0567556262758529,0.033325));
#37785=CARTESIAN_POINT('Origin',(0.,0.,0.033325));
#37786=CARTESIAN_POINT('Ctrl Pts',(-0.0782614497120756,-0.0567556262758528,
0.033325));
#37787=CARTESIAN_POINT('Ctrl Pts',(-0.0596140183847306,-0.0824689362125857,
0.0354166557997537));
#37788=CARTESIAN_POINT('Ctrl Pts',(-0.0274771552068993,-0.0980768870368331,
0.0375083115995075));
#37789=CARTESIAN_POINT('Ctrl Pts',(0.00406898269203012,-0.0967332918525559,
0.0395999673992613));
#37790=CARTESIAN_POINT('Ctrl Pts',(0.0356151205909597,-0.0953896966682786,
0.041691623199015));
#37791=CARTESIAN_POINT('Ctrl Pts',(0.0665705332109873,-0.0770945554754765,
0.0437832789987688));
#37792=CARTESIAN_POINT('Ctrl Pts',(0.0829257401395832,-0.0500177063557517,
0.0458749347985226));
#37793=CARTESIAN_POINT('Ctrl Pts',(0.0992809470681791,-0.022940857236027,
0.0479665905982763));
#37794=CARTESIAN_POINT('Ctrl Pts',(0.101035948305343,0.0129176998106204,
0.0500582463980301));
#37795=CARTESIAN_POINT('Ctrl Pts',(0.0874745068942844,0.0414936169721777,
0.0521499021977838));
#37796=CARTESIAN_POINT('Ctrl Pts',(0.0739130654832254,0.0700695341337352,
0.0542415579975376));
#37797=CARTESIAN_POINT('Ctrl Pts',(0.0450351814239432,0.0913628114102026,
0.0563332137972914));
#37798=CARTESIAN_POINT('Ctrl Pts',(0.0137340407189411,0.0958461699181061,
0.0584248695970452));
#37799=CARTESIAN_POINT('Ctrl Pts',(-0.0175670999860608,0.10032952842601,
0.0605165253967989));
#37800=CARTESIAN_POINT('Ctrl Pts',(-0.0512914973367827,0.0880029681653493,
0.0626081811965526));
#37801=CARTESIAN_POINT('Ctrl Pts',(-0.072322500665143,0.064382075719902,
0.0646998369963064));
#37802=CARTESIAN_POINT('Ctrl Pts',(-0.0878427511625237,0.0469505646311909,
0.0662434163234373));
#37803=CARTESIAN_POINT('Ctrl Pts',(-0.096450181952939,0.0233681626171319,
0.0677869956505682));
#37804=CARTESIAN_POINT('Ctrl Pts',(-0.0966485063039693,-8.22854894029733E-5,
0.0693305749776991));
#37805=CARTESIAN_POINT('Origin',(0.,0.,0.1025));
#37806=CARTESIAN_POINT('',(-0.0967646650617208,6.3821447323616E-5,0.115127758355634));
#37807=CARTESIAN_POINT('',(-0.0967793169573732,5.66163319584007E-5,0.109330574977699));
#37808=CARTESIAN_POINT('',(-0.096675,-1.1839272930757E-17,0.1025));
#37809=CARTESIAN_POINT('Ctrl Pts',(-0.0967646650617208,6.3821447323616E-5,
0.115127758355634));
#37810=CARTESIAN_POINT('Ctrl Pts',(-0.0967967436437804,0.00424079196011727,
0.114851958439798));
#37811=CARTESIAN_POINT('Ctrl Pts',(-0.0965491014611655,0.00841393489638481,
0.114576158523962));
#37812=CARTESIAN_POINT('Ctrl Pts',(-0.0960086603335039,0.012548805287274,
0.114300358608126));
#37813=CARTESIAN_POINT('Ctrl Pts',(-0.091909975909792,0.0439075009856079,
0.112208702808372));
#37814=CARTESIAN_POINT('Ctrl Pts',(-0.0709705314650557,0.0730648952004004,
0.110117047008618));
#37815=CARTESIAN_POINT('Ctrl Pts',(-0.042564880047698,0.0869675511134677,
0.108025391208864));
#37816=CARTESIAN_POINT('Ctrl Pts',(-0.0141592286303404,0.100870207026535,
0.105933735409111));
#37817=CARTESIAN_POINT('Ctrl Pts',(0.0217126297596384,0.0995181246378772,
0.103842079609357));
#37818=CARTESIAN_POINT('Ctrl Pts',(0.0489910406446355,0.0835165288481682,
0.101750423809603));
#37819=CARTESIAN_POINT('Ctrl Pts',(0.0762694515296325,0.0675149330584592,
0.0996587680098494));
#37820=CARTESIAN_POINT('Ctrl Pts',(0.0949544149096479,0.0368638238676987,
0.0975671122100956));
#37821=CARTESIAN_POINT('Ctrl Pts',(0.0966808481865763,0.0052855987430675,
0.0954754564103418));
#37822=CARTESIAN_POINT('Ctrl Pts',(0.0984072814635047,-0.0262926263815637,
0.093383800610588));
#37823=CARTESIAN_POINT('Ctrl Pts',(0.0831751846373464,-0.0587979674400657,
0.0912921448108343));
#37824=CARTESIAN_POINT('Ctrl Pts',(0.0578036983412537,-0.0776779752004735,
0.0892004890110805));
#37825=CARTESIAN_POINT('Ctrl Pts',(0.0324322120451609,-0.0965579829608814,
0.0871088332113267));
#37826=CARTESIAN_POINT('Ctrl Pts',(-0.00307866372086639,-0.101812657423195,
0.085017177411573));
#37827=CARTESIAN_POINT('Ctrl Pts',(-0.0328305038734412,-0.091089490875905,
0.0829255216118192));
#37828=CARTESIAN_POINT('Ctrl Pts',(-0.0625823440260158,-0.0803663243286154,
0.0808338658120654));
#37829=CARTESIAN_POINT('Ctrl Pts',(-0.086575148565138,-0.0536653167717232,
0.0787422100123117));
#37830=CARTESIAN_POINT('Ctrl Pts',(-0.0940682038493122,-0.0229403867380109,
0.0766505542125579));
#37831=CARTESIAN_POINT('Ctrl Pts',(-0.0958866027056606,-0.0154841255046677,
0.0761429555935834));
#37832=CARTESIAN_POINT('Ctrl Pts',(-0.0967332891061196,-0.00779088517959144,
0.0756353569746089));
#37833=CARTESIAN_POINT('Ctrl Pts',(-0.0966658713741579,-8.30033664664526E-5,
0.0751277583556343));
#37834=CARTESIAN_POINT('Ctrl Pts',(-0.0966485063039693,-8.22854894029733E-5,
0.0693305749776991));
#37835=CARTESIAN_POINT('Ctrl Pts',(-0.0967189250436074,-0.0084088020822012,
0.069878651450322));
#37836=CARTESIAN_POINT('Ctrl Pts',(-0.0957291768326631,-0.0167186827609739,
0.0704267279229449));
#37837=CARTESIAN_POINT('Ctrl Pts',(-0.0936122806995565,-0.0247306772532468,
0.0709748043955678));
#37838=CARTESIAN_POINT('Ctrl Pts',(-0.085533448099611,-0.0553073131507138,
0.0730664601953215));
#37839=CARTESIAN_POINT('Ctrl Pts',(-0.0610381735937214,-0.0815453603154133,
0.0751581159950752));
#37840=CARTESIAN_POINT('Ctrl Pts',(-0.0310877945671743,-0.0916989920757568,
0.0772497717948289));
#37841=CARTESIAN_POINT('Ctrl Pts',(-0.0011374155406272,-0.1018526238361,
0.0793414275945827));
#37842=CARTESIAN_POINT('Ctrl Pts',(0.0342680680065774,-0.0959218401920879,
0.0814330833943366));
#37843=CARTESIAN_POINT('Ctrl Pts',(0.0592751346151767,-0.0765613965401887,
0.0835247391940904));
#37844=CARTESIAN_POINT('Ctrl Pts',(0.0842822012237761,-0.0572009528882895,
0.0856163949938442));
#37845=CARTESIAN_POINT('Ctrl Pts',(0.0988908508937702,-0.0244108492285036,
0.0877080507935979));
#37846=CARTESIAN_POINT('Ctrl Pts',(0.096562264665659,0.00712872955992228,
0.0897997065933517));
#37847=CARTESIAN_POINT('Ctrl Pts',(0.0942336784375477,0.0386683083483482,
0.0918913623931054));
#37848=CARTESIAN_POINT('Ctrl Pts',(0.0749678563113312,0.0689573622654141,
0.0939830181928592));
#37849=CARTESIAN_POINT('Ctrl Pts',(0.047389275909168,0.0844357455165206,
0.096074673992613));
#37850=CARTESIAN_POINT('Ctrl Pts',(0.019810695507005,0.099914128767627,
0.0981663297923668));
#37851=CARTESIAN_POINT('Ctrl Pts',(-0.0160806431711048,0.100581841352774,
0.10025798559212));
#37852=CARTESIAN_POINT('Ctrl Pts',(-0.0442159874082662,0.0861399043308145,
0.102349641391874));
#37853=CARTESIAN_POINT('Ctrl Pts',(-0.0723513316454278,0.0716979673088548,
0.104441297191628));
#37854=CARTESIAN_POINT('Ctrl Pts',(-0.092730681441641,0.0421463806797884,
0.106532952991382));
#37855=CARTESIAN_POINT('Ctrl Pts',(-0.0962304983171589,0.0107152449419454,
0.108624608791136));
#37856=CARTESIAN_POINT('Ctrl Pts',(-0.0966242457609418,0.0071790801104245,
0.108859930853323));
#37857=CARTESIAN_POINT('Ctrl Pts',(-0.0968043420335512,0.00361912505495288,
0.109095252915511));
#37858=CARTESIAN_POINT('Ctrl Pts',(-0.0967793169573732,5.66163319584007E-5,
0.109330574977699));
#37859=CARTESIAN_POINT('Origin',(0.,0.,0.1025));
#37860=CARTESIAN_POINT('',(-0.0965227763075221,-6.77612820726425E-6,0.155127758355634));
#37861=CARTESIAN_POINT('',(-0.096524893308144,5.91499715830822E-6,0.149330574977699));
#37862=CARTESIAN_POINT('',(-0.096675,-1.1839272930757E-17,0.1025));
#37863=CARTESIAN_POINT('Ctrl Pts',(-0.0965227763075221,-6.77612820726425E-6,
0.155127758355634));
#37864=CARTESIAN_POINT('Ctrl Pts',(-0.0965190680182828,0.016138816148185,
0.154068559904987));
#37865=CARTESIAN_POINT('Ctrl Pts',(-0.0926787895564408,0.032287429622825,
0.153009361454341));
#37866=CARTESIAN_POINT('Ctrl Pts',(-0.0850136266094788,0.0463495241496994,
0.151950163003694));
#37867=CARTESIAN_POINT('Ctrl Pts',(-0.0698768195982166,0.0741186938986332,
0.14985850720394));
#37868=CARTESIAN_POINT('Ctrl Pts',(-0.0398242971867013,0.0937511675138199,
0.147766851404186));
#37869=CARTESIAN_POINT('Ctrl Pts',(-0.00831514275533874,0.0964661700481194,
0.145675195604432));
#37870=CARTESIAN_POINT('Ctrl Pts',(0.0231940116760242,0.099181172582419,
0.143583539804678));
#37871=CARTESIAN_POINT('Ctrl Pts',(0.0561597981272341,0.0849787040358313,
0.141491884004925));
#37872=CARTESIAN_POINT('Ctrl Pts',(0.0758260807513075,0.0602126271251373,
0.139400228205171));
#37873=CARTESIAN_POINT('Ctrl Pts',(0.0954923633753807,0.0354465502144436,
0.137308572405417));
#37874=CARTESIAN_POINT('Ctrl Pts',(0.101859142172317,0.00011686493964403,
0.135216916605663));
#37875=CARTESIAN_POINT('Ctrl Pts',(0.0920747404299595,-0.0299571361985723,
0.13312526080591));
#37876=CARTESIAN_POINT('Ctrl Pts',(0.0822903386876017,-0.0600311373367887,
0.131033605006156));
#37877=CARTESIAN_POINT('Ctrl Pts',(0.0563547564059492,-0.0848494543384221,
0.128941949206402));
#37878=CARTESIAN_POINT('Ctrl Pts',(0.0258799039839752,-0.0933022984116978,
0.126850293406648));
#37879=CARTESIAN_POINT('Ctrl Pts',(-0.00459494843799892,-0.101755142484973,
0.124758637606895));
#37880=CARTESIAN_POINT('Ctrl Pts',(-0.0396090710002945,-0.0938425136298918,
0.122666981807141));
#37881=CARTESIAN_POINT('Ctrl Pts',(-0.0634871700800987,-0.0731062006114135,
0.120575326007387));
#37882=CARTESIAN_POINT('Ctrl Pts',(-0.0842167694319298,-0.0551041201497079,
0.118759470123469));
#37883=CARTESIAN_POINT('Ctrl Pts',(-0.0965534609291739,-0.0274371894199573,
0.116943614239552));
#37884=CARTESIAN_POINT('Ctrl Pts',(-0.0967646650617208,6.3821447323616E-5,
0.115127758355634));
#37885=CARTESIAN_POINT('Ctrl Pts',(-0.0967793169573732,5.66163319584007E-5,
0.109330574977699));
#37886=CARTESIAN_POINT('Ctrl Pts',(-0.0965819071065392,-0.0280461678752784,
0.111186908715265));
#37887=CARTESIAN_POINT('Ctrl Pts',(-0.0836201771217612,-0.056307862064192,
0.113043242452831));
#37888=CARTESIAN_POINT('Ctrl Pts',(-0.0620812934444443,-0.0743037478312695,
0.114899576190397));
#37889=CARTESIAN_POINT('Ctrl Pts',(-0.0378119877413892,-0.0945809200200219,
0.116991231990151));
#37890=CARTESIAN_POINT('Ctrl Pts',(-0.00265309238045642,-0.101824579550907,
0.119082887789904));
#37891=CARTESIAN_POINT('Ctrl Pts',(0.0276549125922369,-0.0927918697411059,
0.121174543589658));
#37892=CARTESIAN_POINT('Ctrl Pts',(0.0579629175649301,-0.0837591599313047,
0.123266199389412));
#37893=CARTESIAN_POINT('Ctrl Pts',(0.0834200321493839,-0.0584500807808171,
0.125357855189166));
#37894=CARTESIAN_POINT('Ctrl Pts',(0.0926291959676316,-0.0281951895719809,
0.127449510988919));
#37895=CARTESIAN_POINT('Ctrl Pts',(0.101838359785879,0.00205970163685511,
0.129541166788673));
#37896=CARTESIAN_POINT('Ctrl Pts',(0.0947995728379207,0.0372604049040397,
0.131632822588427));
#37897=CARTESIAN_POINT('Ctrl Pts',(0.0746641789865216,0.0616473760057519,
0.133724478388181));
#37898=CARTESIAN_POINT('Ctrl Pts',(0.0545287851351224,0.086034347107464,
0.135816134187934));
#37899=CARTESIAN_POINT('Ctrl Pts',(0.0212967843802825,0.0996075860437037,
0.137907789987688));
#37900=CARTESIAN_POINT('Ctrl Pts',(-0.0101542637302986,0.0962911245681284,
0.139999445787442));
#37901=CARTESIAN_POINT('Ctrl Pts',(-0.04160531184088,0.0929746630925531,
0.142091101587196));
#37902=CARTESIAN_POINT('Ctrl Pts',(-0.0712754073072026,0.0727685012051628,
0.14418275738695));
#37903=CARTESIAN_POINT('Ctrl Pts',(-0.0858809318046248,0.0447174974277489,
0.146274413186703));
#37904=CARTESIAN_POINT('Ctrl Pts',(-0.092994410340263,0.0310555290876898,
0.147293133783702));
#37905=CARTESIAN_POINT('Ctrl Pts',(-0.0965344488013378,0.0155326997615265,
0.148311854380701));
#37906=CARTESIAN_POINT('Ctrl Pts',(-0.096524893308144,5.91499715830822E-6,
0.149330574977699));
#37907=CARTESIAN_POINT('Origin',(0.,0.,-0.0517230892635719));
#37908=CARTESIAN_POINT('',(-0.0737836376428848,-5.17978665142374E-6,0.168276910736428));
#37909=CARTESIAN_POINT('',(-0.0739538094612803,-8.06377484251428E-5,0.176181422596906));
#37910=CARTESIAN_POINT('',(-0.0739,-5.47916578054271E-16,-0.0517230892635719));
#37911=CARTESIAN_POINT('',(0.0526484240822812,-0.0518589764809553,0.183325));
#37912=CARTESIAN_POINT('Ctrl Pts',(-0.0737836376428848,-5.17978665143075E-6,
0.168276910736428));
#37913=CARTESIAN_POINT('Ctrl Pts',(-0.0737864007558564,-0.0120355508218365,
0.169309368085535));
#37914=CARTESIAN_POINT('Ctrl Pts',(-0.0653630139236587,-0.0484316160730116,
0.172433481234396));
#37915=CARTESIAN_POINT('Ctrl Pts',(-0.0107526223003796,-0.085088910335128,
0.177449510988919));
#37916=CARTESIAN_POINT('Ctrl Pts',(0.0372917034486422,-0.0674107586613021,
0.181433083394337));
#37917=CARTESIAN_POINT('Ctrl Pts',(0.0527465304496822,-0.0519092684691894,
0.183325));
#37918=CARTESIAN_POINT('',(-0.0320564751923869,-0.0665852265764703,0.183325));
#37919=CARTESIAN_POINT('Origin',(0.,0.,0.183325));
#37920=CARTESIAN_POINT('Ctrl Pts',(-0.0739538094612803,-8.06377484251584E-5,
0.176181422596905));
#37921=CARTESIAN_POINT('Ctrl Pts',(-0.0739806943658403,-0.00343112332502641,
0.17647095926485));
#37922=CARTESIAN_POINT('Ctrl Pts',(-0.0722722019339485,-0.0309470627246392,
0.178852151732548));
#37923=CARTESIAN_POINT('Ctrl Pts',(-0.0539334858338623,-0.0560528624925751,
0.181233344200246));
#37924=CARTESIAN_POINT('Ctrl Pts',(-0.0320564751923869,-0.0665852265764703,
0.183325));
#37925=CARTESIAN_POINT('Origin',(0.,0.,-0.0517230892635719));
#37926=CARTESIAN_POINT('',(-0.0739685414849875,4.87861904026652E-5,0.128276910736428));
#37927=CARTESIAN_POINT('',(-0.0737852559138541,4.5215235579335E-6,0.136181422596905));
#37928=CARTESIAN_POINT('',(-0.0739,-5.47916578054271E-16,-0.0517230892635719));
#37929=CARTESIAN_POINT('Ctrl Pts',(-0.0739685414849875,4.87861904026683E-5,
0.128276910736428));
#37930=CARTESIAN_POINT('Ctrl Pts',(-0.0738070934850369,-0.0209734502005159,
0.130092766620346));
#37931=CARTESIAN_POINT('Ctrl Pts',(-0.0535140180485454,-0.0664837973240077,
0.134000278304017));
#37932=CARTESIAN_POINT('Ctrl Pts',(0.0232529295866107,-0.0838318934784593,
0.139999445787442));
#37933=CARTESIAN_POINT('Ctrl Pts',(0.0827297187445345,-0.0269172735740158,
0.146274413186704));
#37934=CARTESIAN_POINT('Ctrl Pts',(0.0681290995639721,0.0541025477388684,
0.152549380585964));
#37935=CARTESIAN_POINT('Ctrl Pts',(-0.00746970939628905,0.0866723669969857,
0.158824347985226));
#37936=CARTESIAN_POINT('Ctrl Pts',(-0.0650481952386638,0.0490579501895072,
0.16406685803538));
#37937=CARTESIAN_POINT('Ctrl Pts',(-0.0737808029640662,0.0123367831740457,
0.167217712285781));
#37938=CARTESIAN_POINT('Ctrl Pts',(-0.0737836376428848,-5.17978665143075E-6,
0.168276910736428));
#37939=CARTESIAN_POINT('Ctrl Pts',(-0.0737852559138541,4.52152355793177E-6,
0.136181422596905));
#37940=CARTESIAN_POINT('Ctrl Pts',(-0.0737775628068568,-0.0124960594610031,
0.137254357799661));
#37941=CARTESIAN_POINT('Ctrl Pts',(-0.0648773893377903,-0.049376049988601,
0.140418948802169));
#37942=CARTESIAN_POINT('Ctrl Pts',(-0.00691203799135788,-0.0867186372176302,
0.145675195604432));
#37943=CARTESIAN_POINT('Ctrl Pts',(0.0684817521676531,-0.0536662275708332,
0.151950163003693));
#37944=CARTESIAN_POINT('Ctrl Pts',(0.0825479194741534,0.0274661288420571,
0.158225130402955));
#37945=CARTESIAN_POINT('Ctrl Pts',(0.0227200964169887,0.0839526628083412,
0.164500097802216));
#37946=CARTESIAN_POINT('Ctrl Pts',(-0.0537857498481575,0.0662280371199278,
0.170485528533533));
#37947=CARTESIAN_POINT('Ctrl Pts',(-0.073786473830846,0.0207732810360634,
0.174379303465096));
#37948=CARTESIAN_POINT('Ctrl Pts',(-0.0739538094612803,-8.06377484251584E-5,
0.176181422596905));
#37949=CARTESIAN_POINT('Origin',(0.,0.,-0.0517230892635719));
#37950=CARTESIAN_POINT('',(-0.073893021924492,-6.34491728151829E-5,0.088276910736428));
#37951=CARTESIAN_POINT('',(-0.0739797416410642,4.32784787348095E-5,0.0961814225969055));
#37952=CARTESIAN_POINT('',(-0.0739,-5.47916578054271E-16,-0.0517230892635719));
#37953=CARTESIAN_POINT('Ctrl Pts',(-0.073893021924492,-6.34491728151998E-5,
0.0882769107364281));
#37954=CARTESIAN_POINT('Ctrl Pts',(-0.073944557175508,-0.00595548399039915,
0.0887845093554026));
#37955=CARTESIAN_POINT('Ctrl Pts',(-0.0706303381894479,-0.0360694472427554,
0.0913837637741309));
#37956=CARTESIAN_POINT('Ctrl Pts',(-0.0294984946271671,-0.081844073714394,
0.0960746739926129));
#37957=CARTESIAN_POINT('Ctrl Pts',(0.0519368418851493,-0.0697937884462804,
0.102349641391874));
#37958=CARTESIAN_POINT('Ctrl Pts',(0.0868678567944775,0.00474910384924522,
0.108624608791136));
#37959=CARTESIAN_POINT('Ctrl Pts',(0.0440185536514787,0.0750397778351934,
0.114899576190397));
#37960=CARTESIAN_POINT('Ctrl Pts',(-0.0382446064732518,0.078140441559687,
0.121174543589658));
#37961=CARTESIAN_POINT('Ctrl Pts',(-0.0723681031162574,0.0306247471374611,
0.125633655105002));
#37962=CARTESIAN_POINT('Ctrl Pts',(-0.0739930628939785,0.00324173287667585,
0.128001110820592));
#37963=CARTESIAN_POINT('Ctrl Pts',(-0.0739685414849875,4.87861904026683E-5,
0.128276910736428));
#37964=CARTESIAN_POINT('Ctrl Pts',(-0.0739797416410642,4.32784787348099E-5,
0.0961814225969055));
#37965=CARTESIAN_POINT('Ctrl Pts',(-0.073828838222635,-0.0214389635995149,
0.0980377563344713));
#37966=CARTESIAN_POINT('Ctrl Pts',(-0.0527564789060794,-0.0673850352691751,
0.101985745871791));
#37967=CARTESIAN_POINT('Ctrl Pts',(0.0248479838661208,-0.0833736009117604,
0.108025391208864));
#37968=CARTESIAN_POINT('Ctrl Pts',(0.0832275266990493,-0.0253335404239085,
0.114300358608126));
#37969=CARTESIAN_POINT('Ctrl Pts',(0.0670858244351509,0.0553904928249651,
0.120575326007387));
#37970=CARTESIAN_POINT('Ctrl Pts',(-0.00912348063180574,0.0865173309130365,
0.126850293406648));
#37971=CARTESIAN_POINT('Ctrl Pts',(-0.0655303527769235,0.0481026789811179,
0.132052325603154));
#37972=CARTESIAN_POINT('Ctrl Pts',(-0.0737925602939629,0.0118734575885883,
0.135162701999907));
#37973=CARTESIAN_POINT('Ctrl Pts',(-0.0737852559138541,4.52152355793177E-6,
0.136181422596905));
#37974=CARTESIAN_POINT('Origin',(0.,0.,-0.0517230892635719));
#37975=CARTESIAN_POINT('',(-0.0738258018559393,4.09328341953636E-5,0.0482769107364281));
#37976=CARTESIAN_POINT('',(-0.0738797477720541,-6.29004154842697E-5,0.0561814225969054));
#37977=CARTESIAN_POINT('',(-0.0739,-5.47916578054271E-16,-0.0517230892635719));
#37978=CARTESIAN_POINT('Ctrl Pts',(-0.0738258018559393,4.09328341953522E-5,
0.0482769107364281));
#37979=CARTESIAN_POINT('Ctrl Pts',(-0.0737420584453234,-0.0149871305718488,
0.0495679078902133));
#37980=CARTESIAN_POINT('Ctrl Pts',(-0.0619974316400658,-0.054474758919102,
0.0529505608437523));
#37981=CARTESIAN_POINT('Ctrl Pts',(0.00200588979265343,-0.0869742751577483,
0.0584248695970452));
#37982=CARTESIAN_POINT('Ctrl Pts',(0.0736302858054235,-0.0463507894749077,
0.0646998369963064));
#37983=CARTESIAN_POINT('Ctrl Pts',(0.079297411853797,0.0357745193205231,
0.0709748043955678));
#37984=CARTESIAN_POINT('Ctrl Pts',(0.0139779125109316,0.0858677928042342,
0.077249771794829));
#37985=CARTESIAN_POINT('Ctrl Pts',(-0.0575684509810804,0.0612431240737476,
0.0830171405751159));
#37986=CARTESIAN_POINT('Ctrl Pts',(-0.0737321964584969,0.0183237562160622,
0.0866928535556488));
#37987=CARTESIAN_POINT('Ctrl Pts',(-0.073893021924492,-6.34491728151998E-5,
0.0882769107364281));
#37988=CARTESIAN_POINT('Ctrl Pts',(-0.0738797477720541,-6.29004154842593E-5,
0.0561814225969054));
#37989=CARTESIAN_POINT('Ctrl Pts',(-0.0739335770439367,-0.00642783008921347,
0.0567294990695283));
#37990=CARTESIAN_POINT('Ctrl Pts',(-0.0702896161667766,-0.0370223588314532,
0.0593692313419049));
#37991=CARTESIAN_POINT('Ctrl Pts',(-0.027934008198508,-0.0823914539723853,
0.0641006194140353));
#37992=CARTESIAN_POINT('Ctrl Pts',(0.0532596375466719,-0.0687906809299483,
0.0703755868132967));
#37993=CARTESIAN_POINT('Ctrl Pts',(0.0867609319023758,0.00640524336665911,
0.0766505542125579));
#37994=CARTESIAN_POINT('Ctrl Pts',(0.0425795741016805,0.0758656338855472,
0.0829255216118193));
#37995=CARTESIAN_POINT('Ctrl Pts',(-0.0397282592051405,0.0773968661599418,
0.0892004890110804));
#37996=CARTESIAN_POINT('Ctrl Pts',(-0.0726375375548605,0.0296759427852165,
0.093619122672776));
#37997=CARTESIAN_POINT('Ctrl Pts',(-0.0739988712312329,0.00276652021268154,
0.0959461005347176));
#37998=CARTESIAN_POINT('Ctrl Pts',(-0.0739797416410642,4.32784787348099E-5,
0.0961814225969055));
#37999=CARTESIAN_POINT('Origin',(2.39206768658147E-17,-5.43753587379397E-18,
0.183325));
#38000=CARTESIAN_POINT('',(0.0270116869336341,0.092824697112349,0.183325));
#38001=CARTESIAN_POINT('Ctrl Pts',(0.0527465304496837,-0.0519092684691879,
0.183325));
#38002=CARTESIAN_POINT('Ctrl Pts',(0.0546401156765816,-0.0505045722914166,
0.183325));
#38003=CARTESIAN_POINT('Ctrl Pts',(0.0564577449202127,-0.0490079002578489,
0.183325));
#38004=CARTESIAN_POINT('Ctrl Pts',(0.0581912954394417,-0.0474228118599484,
0.183325));
#38005=CARTESIAN_POINT('Ctrl Pts',(0.0613530156193595,-0.0445318629553705,
0.183325));
#38006=CARTESIAN_POINT('Ctrl Pts',(0.0642355283205663,-0.0413475100044657,
0.183325));
#38007=CARTESIAN_POINT('Ctrl Pts',(0.066834120121686,-0.0379215868621348,
0.183325));
#38008=CARTESIAN_POINT('Ctrl Pts',(0.0685601271369542,-0.0356460592571895,
0.183325));
#38009=CARTESIAN_POINT('Ctrl Pts',(0.0701548344174317,-0.0332713934661594,
0.183325));
#38010=CARTESIAN_POINT('Ctrl Pts',(0.0716166500276835,-0.0308145965037307,
0.183325));
#38011=CARTESIAN_POINT('Ctrl Pts',(0.0732633814775101,-0.0280470211710436,
0.183325));
#38012=CARTESIAN_POINT('Ctrl Pts',(0.0747419256656459,-0.0251747141098478,
0.183325));
#38013=CARTESIAN_POINT('Ctrl Pts',(0.0760495595769769,-0.0222174250112788,
0.183325));
#38014=CARTESIAN_POINT('Ctrl Pts',(0.0771636755795777,-0.0196977877638178,
0.183325));
#38015=CARTESIAN_POINT('Ctrl Pts',(0.0781534655055068,-0.0171156032244178,
0.183325));
#38016=CARTESIAN_POINT('Ctrl Pts',(0.0790121194120802,-0.0144979013638344,
0.183325));
#38017=CARTESIAN_POINT('Ctrl Pts',(0.0811176435774726,-0.00807897694847167,
0.183325));
#38018=CARTESIAN_POINT('Ctrl Pts',(0.0824473371994335,-0.00142879370438768,
0.183325));
#38019=CARTESIAN_POINT('Ctrl Pts',(0.0829720082147319,0.00528756526002575,
0.183325));
#38020=CARTESIAN_POINT('Ctrl Pts',(0.0831605422866328,0.00770100619155721,
0.183325));
#38021=CARTESIAN_POINT('Ctrl Pts',(0.0832446865927584,0.0101257041339963,
0.183325));
#38022=CARTESIAN_POINT('Ctrl Pts',(0.0832217255425897,0.0125466916461908,
0.183325));
#38023=CARTESIAN_POINT('Ctrl Pts',(0.0831801213734689,0.0169333888206161,
0.183325));
#38024=CARTESIAN_POINT('Ctrl Pts',(0.082788129105151,0.0212914783977859,
0.183325));
#38025=CARTESIAN_POINT('Ctrl Pts',(0.0820392315336429,0.0255780886223147,
0.183325));
#38026=CARTESIAN_POINT('Ctrl Pts',(0.0811462944344166,0.0306891658176867,
0.183325));
#38027=CARTESIAN_POINT('Ctrl Pts',(0.0797466521321354,0.0356990115058088,
0.183325));
#38028=CARTESIAN_POINT('Ctrl Pts',(0.077891263133679,0.0405655957602974,
0.183325));
#38029=CARTESIAN_POINT('Ctrl Pts',(0.0769495055492577,0.0430357745937942,
0.183325));
#38030=CARTESIAN_POINT('Ctrl Pts',(0.0758888412672695,0.0454706621806907,
0.183325));
#38031=CARTESIAN_POINT('Ctrl Pts',(0.0747230976172314,0.0478488836962904,
0.183325));
#38032=CARTESIAN_POINT('Ctrl Pts',(0.0722755117057051,0.0528421782991648,
0.183325));
#38033=CARTESIAN_POINT('Ctrl Pts',(0.0693611729291524,0.0576008143227626,
0.183325));
#38034=CARTESIAN_POINT('Ctrl Pts',(0.0660414991224629,0.0620762069120578,
0.183325));
#38035=CARTESIAN_POINT('Ctrl Pts',(0.0634288730603047,0.0655983985483629,
0.183325));
#38036=CARTESIAN_POINT('Ctrl Pts',(0.0605647053893801,0.0689452797930669,
0.183325));
#38037=CARTESIAN_POINT('Ctrl Pts',(0.0574711285697693,0.0720908849414506,
0.183325));
#38038=CARTESIAN_POINT('Ctrl Pts',(0.0555574201065491,0.0740367784962025,
0.183325));
#38039=CARTESIAN_POINT('Ctrl Pts',(0.0535622771425319,0.0758988193647838,
0.183325));
#38040=CARTESIAN_POINT('Ctrl Pts',(0.0514951532726063,0.0776691885827886,
0.183325));
#38041=CARTESIAN_POINT('Ctrl Pts',(0.0457945092115925,0.0825514527350495,
0.183325));
#38042=CARTESIAN_POINT('Ctrl Pts',(0.0395430238483871,0.0867452732609154,
0.183325));
#38043=CARTESIAN_POINT('Ctrl Pts',(0.0328518740906454,0.0901282422580833,
0.183325));
#38044=CARTESIAN_POINT('Ctrl Pts',(0.0309405875159093,0.0910945669498233,
0.183325));
#38045=CARTESIAN_POINT('Ctrl Pts',(0.028993174707338,0.0919945319583493,
0.183325));
#38046=CARTESIAN_POINT('Ctrl Pts',(0.0270116869336341,0.0928246971123491,
0.183325));
#38047=CARTESIAN_POINT('',(-0.096675,-1.1839272930757E-17,0.183325));
#38048=CARTESIAN_POINT('Origin',(0.,0.,0.183325));
#38049=CARTESIAN_POINT('',(-0.0568713879600425,0.0783474662532323,0.183325));
#38050=CARTESIAN_POINT('Origin',(0.,0.,0.183325));
#38051=CARTESIAN_POINT('Ctrl Pts',(-0.0568713879600414,0.0783474662532331,
0.183325));
#38052=CARTESIAN_POINT('Ctrl Pts',(-0.0591169345770589,0.076315216152872,
0.183325));
#38053=CARTESIAN_POINT('Ctrl Pts',(-0.0612562739924736,0.0741756319431535,
0.183325));
#38054=CARTESIAN_POINT('Ctrl Pts',(-0.0632787201244711,0.0719302794170955,
0.183325));
#38055=CARTESIAN_POINT('Ctrl Pts',(-0.0669251707984549,0.0678819306861015,
0.183325));
#38056=CARTESIAN_POINT('Ctrl Pts',(-0.0701924279121554,0.0634898239153897,
0.183325));
#38057=CARTESIAN_POINT('Ctrl Pts',(-0.0730590010288785,0.0588183271803977,
0.183325));
#38058=CARTESIAN_POINT('Ctrl Pts',(-0.0746566708643339,0.0562146924165105,
0.183325));
#38059=CARTESIAN_POINT('Ctrl Pts',(-0.0761246913269906,0.0535322363953255,
0.183325));
#38060=CARTESIAN_POINT('Ctrl Pts',(-0.0774597304405968,0.0507837216288562,
0.183325));
#38061=CARTESIAN_POINT('Ctrl Pts',(-0.0796092977453778,0.0463582951237468,
0.183325));
#38062=CARTESIAN_POINT('Ctrl Pts',(-0.0814151665646452,0.0417606422657594,
0.183325));
#38063=CARTESIAN_POINT('Ctrl Pts',(-0.0828578508387229,0.0370391959667551,
0.183325));
#38064=CARTESIAN_POINT('Ctrl Pts',(-0.0836414140099655,0.0344748431825919,
0.183325));
#38065=CARTESIAN_POINT('Ctrl Pts',(-0.0843160631417445,0.0318785210818391,
0.183325));
#38066=CARTESIAN_POINT('Ctrl Pts',(-0.0848776834159108,0.0292657100558518,
0.183325));
#38067=CARTESIAN_POINT('Ctrl Pts',(-0.0863774880178461,0.0222882090983227,
0.183325));
#38068=CARTESIAN_POINT('Ctrl Pts',(-0.0870800845145338,0.01517559244937,
0.183325));
#38069=CARTESIAN_POINT('Ctrl Pts',(-0.08691711176372,0.00808290042294868,
0.183325));
#38070=CARTESIAN_POINT('Ctrl Pts',(-0.086829761851914,0.00428136906337395,
0.183325));
#38071=CARTESIAN_POINT('Ctrl Pts',(-0.0864910968448572,0.000479251015311818,
0.183325));
#38072=CARTESIAN_POINT('Ctrl Pts',(-0.0858921759183976,-0.00326140466639689,
0.183325));
#38073=CARTESIAN_POINT('Ctrl Pts',(-0.0854431276238688,-0.00606600704390875,
0.183325));
#38074=CARTESIAN_POINT('Ctrl Pts',(-0.084848151198669,-0.00883918603235441,
0.183325));
#38075=CARTESIAN_POINT('Ctrl Pts',(-0.0841024998475747,-0.0115704941964249,
0.183325));
#38076=CARTESIAN_POINT('Ctrl Pts',(-0.08282572696136,-0.0162472914726108,
0.183325));
#38077=CARTESIAN_POINT('Ctrl Pts',(-0.0811075596191732,-0.0208019296013592,
0.183325));
#38078=CARTESIAN_POINT('Ctrl Pts',(-0.0789832762820567,-0.0251872000190629,
0.183325));
#38079=CARTESIAN_POINT('Ctrl Pts',(-0.0776463058116779,-0.0279471788555274,
0.183325));
#38080=CARTESIAN_POINT('Ctrl Pts',(-0.0761461905929749,-0.0306420990887643,
0.183325));
#38081=CARTESIAN_POINT('Ctrl Pts',(-0.0745048321361633,-0.0332382132025085,
0.183325));
#38082=CARTESIAN_POINT('Ctrl Pts',(-0.0720489128888603,-0.037122706923962,
0.183325));
#38083=CARTESIAN_POINT('Ctrl Pts',(-0.0692726962881112,-0.0407973756999029,
0.183325));
#38084=CARTESIAN_POINT('Ctrl Pts',(-0.0662082873966704,-0.0442215373549909,
0.183325));
#38085=CARTESIAN_POINT('Ctrl Pts',(-0.0638653650588976,-0.0468395120163549,
0.183325));
#38086=CARTESIAN_POINT('Ctrl Pts',(-0.0613537638211011,-0.0493109066276996,
0.183325));
#38087=CARTESIAN_POINT('Ctrl Pts',(-0.0586860692431017,-0.0516129350947554,
0.183325));
#38088=CARTESIAN_POINT('Ctrl Pts',(-0.0569207005495688,-0.0531363212503061,
0.183325));
#38089=CARTESIAN_POINT('Ctrl Pts',(-0.0550890271379007,-0.0545832784834442,
0.183325));
#38090=CARTESIAN_POINT('Ctrl Pts',(-0.0532033891510083,-0.0559417504951859,
0.183325));
#38091=CARTESIAN_POINT('Ctrl Pts',(-0.0482461350711257,-0.0595131098809348,
0.183325));
#38092=CARTESIAN_POINT('Ctrl Pts',(-0.0429006042715654,-0.0624903801211849,
0.183325));
#38093=CARTESIAN_POINT('Ctrl Pts',(-0.0372392688433482,-0.0647497023123468,
0.183325));
#38094=CARTESIAN_POINT('Ctrl Pts',(-0.0355395009110826,-0.0654280446324383,
0.183325));
#38095=CARTESIAN_POINT('Ctrl Pts',(-0.0338112391786412,-0.0660413200514086,
0.183325));
#38096=CARTESIAN_POINT('Ctrl Pts',(-0.0320564751923869,-0.0665852265764703,
0.183325));
#38097=CARTESIAN_POINT('Ctrl Pts',(-0.0598243716961198,-0.0433849576600519,
0.0201758476192062));
#38098=CARTESIAN_POINT('Ctrl Pts',(-0.0455699607823283,-0.0630406453179218,
0.02226750341896));
#38099=CARTESIAN_POINT('Ctrl Pts',(0.00356195933852505,-0.0869026068573454,
0.0264508150184675));
#38100=CARTESIAN_POINT('Ctrl Pts',(0.0745504773406983,-0.0449472636719899,
0.0327257824177288));
#38101=CARTESIAN_POINT('Ctrl Pts',(0.0785751349489661,0.0372853931394063,
0.0390007498169901));
#38102=CARTESIAN_POINT('Ctrl Pts',(0.0123509105275246,0.0861162136430816,
0.0452757172162514));
#38103=CARTESIAN_POINT('Ctrl Pts',(-0.0649875833194373,0.0578483221531574,
0.0515506846155127));
#38104=CARTESIAN_POINT('Ctrl Pts',(-0.0841078107116264,-0.022221037045425,
0.057825652014774));
#38105=CARTESIAN_POINT('Ctrl Pts',(-0.027934008198508,-0.0823914539723853,
0.0641006194140353));
#38106=CARTESIAN_POINT('Ctrl Pts',(0.0532596375466719,-0.0687906809299483,
0.0703755868132967));
#38107=CARTESIAN_POINT('Ctrl Pts',(0.0867609319023758,0.00640524336665911,
0.0766505542125579));
#38108=CARTESIAN_POINT('Ctrl Pts',(0.0425795741016805,0.0758656338855472,
0.0829255216118193));
#38109=CARTESIAN_POINT('Ctrl Pts',(-0.0397282592051405,0.0773968661599418,
0.0892004890110804));
#38110=CARTESIAN_POINT('Ctrl Pts',(-0.0864632149829576,0.00962767292835096,
0.0954754564103419));
#38111=CARTESIAN_POINT('Ctrl Pts',(-0.0557801733774148,-0.0667620744778611,
0.101750423809603));
#38112=CARTESIAN_POINT('Ctrl Pts',(0.0248479838661208,-0.0833736009117604,
0.108025391208864));
#38113=CARTESIAN_POINT('Ctrl Pts',(0.0832275266990493,-0.0253335404239085,
0.114300358608126));
#38114=CARTESIAN_POINT('Ctrl Pts',(0.0670858244351509,0.0553904928249651,
0.120575326007387));
#38115=CARTESIAN_POINT('Ctrl Pts',(-0.00912348063180574,0.0865173309130365,
0.126850293406648));
#38116=CARTESIAN_POINT('Ctrl Pts',(-0.0771644443233876,0.0401795384078964,
0.13312526080591));
#38117=CARTESIAN_POINT('Ctrl Pts',(-0.0761117357355759,-0.0421386305548231,
0.139400228205171));
#38118=CARTESIAN_POINT('Ctrl Pts',(-0.00691203799135788,-0.0867186372176302,
0.145675195604432));
#38119=CARTESIAN_POINT('Ctrl Pts',(0.0684817521676531,-0.0536662275708332,
0.151950163003693));
#38120=CARTESIAN_POINT('Ctrl Pts',(0.0825479194741534,0.0274661288420571,
0.158225130402955));
#38121=CARTESIAN_POINT('Ctrl Pts',(0.0227200964169887,0.0839526628083412,
0.164500097802216));
#38122=CARTESIAN_POINT('Ctrl Pts',(-0.0574866109557766,0.065370633652616,
0.170775065201478));
#38123=CARTESIAN_POINT('Ctrl Pts',(-0.0861511939033514,-0.0119466489844985,
0.177050032600739));
#38124=CARTESIAN_POINT('Ctrl Pts',(-0.0539334858338623,-0.0560528624925751,
0.181233344200246));
#38125=CARTESIAN_POINT('Ctrl Pts',(-0.0320564751923869,-0.0665852265764703,
0.183325));
#38126=CARTESIAN_POINT('Ctrl Pts',(-0.0659700643681051,-0.0478418471986522,
0.0245588984128041));
#38127=CARTESIAN_POINT('Ctrl Pts',(-0.0502513133164625,-0.0695167422828098,
0.0266505542125579));
#38128=CARTESIAN_POINT('Ctrl Pts',(0.00392787554932748,-0.0958300171919238,
0.0308338658120655));
#38129=CARTESIAN_POINT('Ctrl Pts',(0.0822089668374704,-0.0495646472088848,
0.0371088332113267));
#38130=CARTESIAN_POINT('Ctrl Pts',(0.0866470731468132,0.0411156810453602,
0.043383800610588));
#38131=CARTESIAN_POINT('Ctrl Pts',(0.0136197061399035,0.094962838657611,
0.0496587680098493));
#38132=CARTESIAN_POINT('Ctrl Pts',(-0.0716636871087931,0.063791017403668,
0.0559337354091106));
#38133=CARTESIAN_POINT('Ctrl Pts',(-0.0927481146762511,-0.0245037800256215,
0.062208702808372));
#38134=CARTESIAN_POINT('Ctrl Pts',(-0.0308036384949493,-0.0908554384749611,
0.0684836702076331));
#38135=CARTESIAN_POINT('Ctrl Pts',(0.0587309422157087,-0.0758574728026573,
0.0747586376068946));
#38136=CARTESIAN_POINT('Ctrl Pts',(0.0956737881228386,0.00706324705486688,
0.0810336050061558));
#38137=CARTESIAN_POINT('Ctrl Pts',(0.0469537274628253,0.0836592279845247,
0.0873085724054171));
#38138=CARTESIAN_POINT('Ctrl Pts',(-0.0438095000864985,0.0853477620859351,
0.0935835398046784));
#38139=CARTESIAN_POINT('Ctrl Pts',(-0.0953454870679233,0.0106167133024745,
0.0998585072039397));
#38140=CARTESIAN_POINT('Ctrl Pts',(-0.0615104099523837,-0.073620469814953,
0.106133474603201));
#38141=CARTESIAN_POINT('Ctrl Pts',(0.0274005902375725,-0.091938480301771,
0.112408442002462));
#38142=CARTESIAN_POINT('Ctrl Pts',(0.0917774000439788,-0.0279360274927155,
0.118683409401724));
#38143=CARTESIAN_POINT('Ctrl Pts',(0.0739774782534214,0.0610806979403848,
0.124958376800985));
#38144=CARTESIAN_POINT('Ctrl Pts',(-0.0100607258793897,0.0954051622686722,
0.131233344200246));
#38145=CARTESIAN_POINT('Ctrl Pts',(-0.0850914638067668,0.0443071387111884,
0.137508311599508));
#38146=CARTESIAN_POINT('Ctrl Pts',(-0.0839306116100808,-0.0464674862647287,
0.143783278998769));
#38147=CARTESIAN_POINT('Ctrl Pts',(-0.00762210414044755,-0.0956271485511058,
0.15005824639803));
#38148=CARTESIAN_POINT('Ctrl Pts',(0.0755168081244337,-0.0591793007910665,
0.156333213797291));
#38149=CARTESIAN_POINT('Ctrl Pts',(0.0910279775076395,0.0302876944008205,
0.162608181196553));
#38150=CARTESIAN_POINT('Ctrl Pts',(0.0250541072239211,0.0925770285975157,
0.168883148595814));
#38151=CARTESIAN_POINT('Ctrl Pts',(-0.0633921480081798,0.0720860877863026,
0.175158115995075));
#38152=CARTESIAN_POINT('Ctrl Pts',(-0.0950014124019929,-0.0131739152480164,
0.181433083394337));
#38153=CARTESIAN_POINT('Ctrl Pts',(-0.0594740142049323,-0.0618111121239165,
0.185616394993844));
#38154=CARTESIAN_POINT('Ctrl Pts',(-0.0353496020417627,-0.0734254545208957,
0.187708050793598));
#38155=CARTESIAN_POINT('Ctrl Pts',(-0.0721157570400904,-0.0522987367372524,
0.028941949206402));
#38156=CARTESIAN_POINT('Ctrl Pts',(-0.0549326658505966,-0.0759928392476978,
0.0310336050061558));
#38157=CARTESIAN_POINT('Ctrl Pts',(0.00429379176012989,-0.104757427526502,
0.0352169166056634));
#38158=CARTESIAN_POINT('Ctrl Pts',(0.0898674563342426,-0.0541820307457796,
0.0414918840049246));
#38159=CARTESIAN_POINT('Ctrl Pts',(0.0947190113446605,0.044945968951314,
0.047766851404186));
#38160=CARTESIAN_POINT('Ctrl Pts',(0.0148885017522822,0.103809463672141,
0.0540418188034472));
#38161=CARTESIAN_POINT('Ctrl Pts',(-0.0783397908981488,0.0697337126541784,
0.0603167862027086));
#38162=CARTESIAN_POINT('Ctrl Pts',(-0.101388418640876,-0.0267865230058178,
0.0665917536019698));
#38163=CARTESIAN_POINT('Ctrl Pts',(-0.0336732687913905,-0.099319422977537,
0.0728667210012312));
#38164=CARTESIAN_POINT('Ctrl Pts',(0.0642022468847453,-0.0829242646753663,
0.0791416884004924));
#38165=CARTESIAN_POINT('Ctrl Pts',(0.104586644343302,0.00772125074307456,
0.0854166557997538));
#38166=CARTESIAN_POINT('Ctrl Pts',(0.0513278808239699,0.0914528220835024,
0.0916916231990151));
#38167=CARTESIAN_POINT('Ctrl Pts',(-0.0478907409678564,0.0932986580119281,
0.0979665905982763));
#38168=CARTESIAN_POINT('Ctrl Pts',(-0.104227759152889,0.0116057536765983,
0.104241557997538));
#38169=CARTESIAN_POINT('Ctrl Pts',(-0.0672406465273527,-0.080478865152045,
0.110516525396799));
#38170=CARTESIAN_POINT('Ctrl Pts',(0.0299531966090245,-0.100503359691781,
0.11679149279606));
#38171=CARTESIAN_POINT('Ctrl Pts',(0.100327273388908,-0.0305385145615227,
0.123066460195322));
#38172=CARTESIAN_POINT('Ctrl Pts',(0.0808691320716919,0.0667709030558047,
0.129341427594583));
#38173=CARTESIAN_POINT('Ctrl Pts',(-0.0109979711269736,0.104292993624308,
0.135616394993844));
#38174=CARTESIAN_POINT('Ctrl Pts',(-0.0930184832901458,0.0484347390144806,
0.141891362393105));
#38175=CARTESIAN_POINT('Ctrl Pts',(-0.0917494874845858,-0.0507963419746343,
0.148166329792367));
#38176=CARTESIAN_POINT('Ctrl Pts',(-0.00833217028953726,-0.104535659884581,
0.154441297191628));
#38177=CARTESIAN_POINT('Ctrl Pts',(0.0825518640812145,-0.0646923740112998,
0.160716264590889));
#38178=CARTESIAN_POINT('Ctrl Pts',(0.0995080355411255,0.0331092599595838,
0.166991231990151));
#38179=CARTESIAN_POINT('Ctrl Pts',(0.0273881180308536,0.10120139438669,
0.173266199389412));
#38180=CARTESIAN_POINT('Ctrl Pts',(-0.0692976850605831,0.0788015419199893,
0.179541166788673));
#38181=CARTESIAN_POINT('Ctrl Pts',(-0.103851630900634,-0.0144011815115344,
0.185816134187935));
#38182=CARTESIAN_POINT('Ctrl Pts',(-0.0650145425760024,-0.0675693617552579,
0.189999445787442));
#38183=CARTESIAN_POINT('Ctrl Pts',(-0.0386427288911385,-0.0802656824653211,
0.192091101587196));
#38184=CARTESIAN_POINT('Ctrl Pts',(-0.0782614497120757,-0.0567556262758526,
0.033325));
#38185=CARTESIAN_POINT('Ctrl Pts',(-0.0596140183847307,-0.0824689362125857,
0.0354166557997537));
#38186=CARTESIAN_POINT('Ctrl Pts',(0.00465970797093226,-0.113684837861081,
0.0395999673992613));
#38187=CARTESIAN_POINT('Ctrl Pts',(0.0975259458310149,-0.0587994142826744,
0.0458749347985225));
#38188=CARTESIAN_POINT('Ctrl Pts',(0.102790949542507,0.0487762568572679,
0.0521499021977838));
#38189=CARTESIAN_POINT('Ctrl Pts',(0.0161572973646611,0.11265608868667,
0.0584248695970452));
#38190=CARTESIAN_POINT('Ctrl Pts',(-0.0850158946875046,0.0756764079046889,
0.0646998369963064));
#38191=CARTESIAN_POINT('Ctrl Pts',(-0.110028722605501,-0.0290692659860142,
0.0709748043955679));
#38192=CARTESIAN_POINT('Ctrl Pts',(-0.0365428990878319,-0.107783407480113,
0.0772497717948288));
#38193=CARTESIAN_POINT('Ctrl Pts',(0.0696735515537822,-0.0899910565480753,
0.0835247391940905));
#38194=CARTESIAN_POINT('Ctrl Pts',(0.113499500563764,0.00837925443128228,
0.0897997065933516));
#38195=CARTESIAN_POINT('Ctrl Pts',(0.0557020341851148,0.0992464161824799,
0.096074673992613));
#38196=CARTESIAN_POINT('Ctrl Pts',(-0.0519719818492145,0.101249553937921,
0.102349641391874));
#38197=CARTESIAN_POINT('Ctrl Pts',(-0.113110031237854,0.0125947940507219,
0.108624608791136));
#38198=CARTESIAN_POINT('Ctrl Pts',(-0.0729708831023218,-0.0873372604891369,
0.114899576190397));
#38199=CARTESIAN_POINT('Ctrl Pts',(0.0325058029804763,-0.109068239081792,
0.121174543589658));
#38200=CARTESIAN_POINT('Ctrl Pts',(0.108877146733838,-0.0331410016303297,
0.127449510988919));
#38201=CARTESIAN_POINT('Ctrl Pts',(0.0877607858899622,0.0724611081712244,
0.133724478388181));
#38202=CARTESIAN_POINT('Ctrl Pts',(-0.0119352163745575,0.113180824979943,
0.139999445787442));
#38203=CARTESIAN_POINT('Ctrl Pts',(-0.100945502773525,0.0525623393177726,
0.146274413186703));
#38204=CARTESIAN_POINT('Ctrl Pts',(-0.0995683633590906,-0.05512519768454,
0.152549380585965));
#38205=CARTESIAN_POINT('Ctrl Pts',(-0.00904223643862709,-0.113444171218057,
0.158824347985226));
#38206=CARTESIAN_POINT('Ctrl Pts',(0.0895869200379953,-0.0702054472315332,
0.165099315384487));
#38207=CARTESIAN_POINT('Ctrl Pts',(0.107988093574611,0.0359308255183472,
0.171374282783748));
#38208=CARTESIAN_POINT('Ctrl Pts',(0.0297221288377862,0.109825760175864,
0.17764925018301));
#38209=CARTESIAN_POINT('Ctrl Pts',(-0.0752032221129864,0.0855169960536761,
0.183924217582271));
#38210=CARTESIAN_POINT('Ctrl Pts',(-0.112701849399276,-0.0156284477750525,
0.190199184981533));
#38211=CARTESIAN_POINT('Ctrl Pts',(-0.0705550709470724,-0.0733276113865993,
0.19438249658104));
#38212=CARTESIAN_POINT('Ctrl Pts',(-0.0419358557405144,-0.0871059104097464,
0.196474152380794));
#38213=CARTESIAN_POINT('Ctrl Pts',(-0.096524893308144,5.91499715830822E-6,
0.149330574977699));
#38214=CARTESIAN_POINT('Ctrl Pts',(-0.0965148292875898,-0.0163471792745932,
0.150403510180454));
#38215=CARTESIAN_POINT('Ctrl Pts',(-0.0925673112842537,-0.0327046611907102,
0.151476445383209));
#38216=CARTESIAN_POINT('Ctrl Pts',(-0.0847101987747527,-0.0468971037730737,
0.152549380585965));
#38217=CARTESIAN_POINT('Ctrl Pts',(-0.0693929877189364,-0.0745648555290454,
0.154641036385718));
#38218=CARTESIAN_POINT('Ctrl Pts',(-0.0392176120787817,-0.0940045133735512,
0.156732692185472));
#38219=CARTESIAN_POINT('Ctrl Pts',(-0.00769173151260052,-0.0965178882980501,
0.158824347985226));
#38220=CARTESIAN_POINT('Ctrl Pts',(0.0238341490535804,-0.0990312632225489,
0.16091600378498));
#38221=CARTESIAN_POINT('Ctrl Pts',(0.0567105345457878,-0.0846183552270411,
0.163007659584734));
#38222=CARTESIAN_POINT('Ctrl Pts',(0.0762155895479942,-0.0597225224376405,
0.165099315384487));
#38223=CARTESIAN_POINT('Ctrl Pts',(0.0957206445502008,-0.0348266896482397,
0.167190971184241));
#38224=CARTESIAN_POINT('Ctrl Pts',(0.101854369062406,0.000552067935053632,
0.169282626983995));
#38225=CARTESIAN_POINT('Ctrl Pts',(0.0918769038623711,0.0305572691696201,
0.171374282783748));
#38226=CARTESIAN_POINT('Ctrl Pts',(0.0818994386623363,0.0605624704041863,
0.173465938583502));
#38227=CARTESIAN_POINT('Ctrl Pts',(0.055810783750061,0.0851941152900256,
0.175557594383256));
#38228=CARTESIAN_POINT('Ctrl Pts',(0.025278897802128,0.0934584770459136,
0.17764925018301));
#38229=CARTESIAN_POINT('Ctrl Pts',(-0.00233739644375865,0.100933647311985,
0.179541166788673));
#38230=CARTESIAN_POINT('Ctrl Pts',(-0.0335888415240724,0.0950182145574911,
0.181433083394336));
#38231=CARTESIAN_POINT('Ctrl Pts',(-0.0568713879600425,0.0783474662532323,
0.183325));
#38232=CARTESIAN_POINT('',(0.0666656654670482,-0.0321318641035092,0.033325));
#38233=CARTESIAN_POINT('Ctrl Pts',(0.0666656654670482,-0.0321318641035094,
0.033325));
#38234=CARTESIAN_POINT('Ctrl Pts',(0.0659824885931634,-0.0343884334763996,
0.033325));
#38235=CARTESIAN_POINT('Ctrl Pts',(0.0651870973984133,-0.0366045459221621,
0.033325));
#38236=CARTESIAN_POINT('Ctrl Pts',(0.0642801010966116,-0.0387713539337305,
0.033325));
#38237=CARTESIAN_POINT('Ctrl Pts',(0.0626258865399732,-0.0427232612866675,
0.033325));
#38238=CARTESIAN_POINT('Ctrl Pts',(0.0606012519142644,-0.0465113694703073,
0.033325));
#38239=CARTESIAN_POINT('Ctrl Pts',(0.0582533982229137,-0.0501137477423414,
0.033325));
#38240=CARTESIAN_POINT('Ctrl Pts',(0.0566939280556225,-0.0525064868926687,
0.033325));
#38241=CARTESIAN_POINT('Ctrl Pts',(0.0549968220046632,-0.0548090897547331,
0.033325));
#38242=CARTESIAN_POINT('Ctrl Pts',(0.053177551929251,-0.0570143177582109,
0.033325));
#38243=CARTESIAN_POINT('Ctrl Pts',(0.0511281594918407,-0.0594984885551547,
0.033325));
#38244=CARTESIAN_POINT('Ctrl Pts',(0.048923417608628,-0.0618596889026584,
0.033325));
#38245=CARTESIAN_POINT('Ctrl Pts',(0.0465809977751913,-0.0640886901070536,
0.033325));
#38246=CARTESIAN_POINT('Ctrl Pts',(0.0445852221789506,-0.0659878313900217,
0.033325));
#38247=CARTESIAN_POINT('Ctrl Pts',(0.0424886078928854,-0.0677910510833029,
0.033325));
#38248=CARTESIAN_POINT('Ctrl Pts',(0.0403143005657056,-0.0694828159680428,
0.033325));
#38249=CARTESIAN_POINT('Ctrl Pts',(0.0349826512621487,-0.0736312162225759,
0.033325));
#38250=CARTESIAN_POINT('Ctrl Pts',(0.0291714649030019,-0.0771273603905254,
0.033325));
#38251=CARTESIAN_POINT('Ctrl Pts',(0.0230262842057801,-0.0798880535992034,
0.033325));
#38252=CARTESIAN_POINT('Ctrl Pts',(0.0208180884878706,-0.0808800750257857,
0.033325));
#38253=CARTESIAN_POINT('Ctrl Pts',(0.0185640638716545,-0.0817776312978301,
0.033325));
#38254=CARTESIAN_POINT('Ctrl Pts',(0.0162773829813682,-0.0825731145983514,
0.033325));
#38255=CARTESIAN_POINT('Ctrl Pts',(0.0121340440651408,-0.0840144862082949,
0.033325));
#38256=CARTESIAN_POINT('Ctrl Pts',(0.00789937518293787,-0.0851163747295676,
0.033325));
#38257=CARTESIAN_POINT('Ctrl Pts',(0.0036115325539914,-0.0858581761147571,
0.033325));
#38258=CARTESIAN_POINT('Ctrl Pts',(-0.00150101100008291,-0.0867426516467301,
0.033325));
#38259=CARTESIAN_POINT('Ctrl Pts',(-0.00668928069841552,-0.0871159893456262,
0.033325));
#38260=CARTESIAN_POINT('Ctrl Pts',(-0.0118965134956391,-0.0870119718507496,
0.033325));
#38261=CARTESIAN_POINT('Ctrl Pts',(-0.0145396045993167,-0.0869591745731857,
0.033325));
#38262=CARTESIAN_POINT('Ctrl Pts',(-0.0171896073044249,-0.0867825364379904,
0.033325));
#38263=CARTESIAN_POINT('Ctrl Pts',(-0.0198217339970555,-0.0864878592704142,
0.033325));
#38264=CARTESIAN_POINT('Ctrl Pts',(-0.0253481174327742,-0.0858691584220329,
0.033325));
#38265=CARTESIAN_POINT('Ctrl Pts',(-0.0308111441111724,-0.0847318941000841,
0.033325));
#38266=CARTESIAN_POINT('Ctrl Pts',(-0.0361443503728786,-0.0831174822393533,
0.033325));
#38267=CARTESIAN_POINT('Ctrl Pts',(-0.0403416519334237,-0.0818469194503115,
0.033325));
#38268=CARTESIAN_POINT('Ctrl Pts',(-0.0444588266991117,-0.0802804065246257,
0.033325));
#38269=CARTESIAN_POINT('Ctrl Pts',(-0.0484639623864034,-0.0784300134796681,
0.033325));
#38270=CARTESIAN_POINT('Ctrl Pts',(-0.0509415676276126,-0.0772853472649801,
0.033325));
#38271=CARTESIAN_POINT('Ctrl Pts',(-0.053367724951023,-0.076035724041335,
0.033325));
#38272=CARTESIAN_POINT('Ctrl Pts',(-0.055731883450712,-0.0746874037064015,
0.033325));
#38273=CARTESIAN_POINT('Ctrl Pts',(-0.0622516783351781,-0.0709690523253594,
0.033325));
#38274=CARTESIAN_POINT('Ctrl Pts',(-0.0683093364934852,-0.0664998270329524,
0.033325));
#38275=CARTESIAN_POINT('Ctrl Pts',(-0.0737521082015833,-0.061343066863607,
0.033325));
#38276=CARTESIAN_POINT('Ctrl Pts',(-0.0753068057249169,-0.0598700669485494,
0.033325));
#38277=CARTESIAN_POINT('Ctrl Pts',(-0.0768112297895693,-0.0583406634828853,
0.033325));
#38278=CARTESIAN_POINT('Ctrl Pts',(-0.0782614497120756,-0.0567556262758528,
0.033325));
#38279=CARTESIAN_POINT('Ctrl Pts',(0.0666656654670482,-0.0321318641035092,
0.033325));
#38280=CARTESIAN_POINT('Ctrl Pts',(0.0760414822059936,-0.0123520292445354,
0.0352169166056634));
#38281=CARTESIAN_POINT('Ctrl Pts',(0.0764671442019932,0.0388397324871015,
0.0392004890110805));
#38282=CARTESIAN_POINT('Ctrl Pts',(0.0123509105275246,0.0861162136430816,
0.0452757172162514));
#38283=CARTESIAN_POINT('Ctrl Pts',(-0.0582325826622868,0.0603173335870826,
0.0510026081428899));
#38284=CARTESIAN_POINT('Ctrl Pts',(-0.0737281452942561,0.0178630175061391,
0.0546378432697745));
#38285=CARTESIAN_POINT('Ctrl Pts',(-0.0738797477720541,-6.29004154842593E-5,
0.0561814225969054));
#38286=CARTESIAN_POINT('Origin',(-2.39206768658147E-17,-5.43753587379397E-18,
0.033325));
#38287=CARTESIAN_POINT('',(0.0518589764809551,0.0526484240822814,0.033325));
#38288=CARTESIAN_POINT('Ctrl Pts',(-0.0929447515460691,0.0270916053744145,
0.033325));
#38289=CARTESIAN_POINT('Ctrl Pts',(-0.0917896323636415,0.0298912877885352,
0.033325));
#38290=CARTESIAN_POINT('Ctrl Pts',(-0.0904976311659083,0.032627221089921,
0.0333249999999999));
#38291=CARTESIAN_POINT('Ctrl Pts',(-0.0890666151901405,0.0352888178066413,
0.0333249999999999));
#38292=CARTESIAN_POINT('Ctrl Pts',(-0.0864865082201888,0.0400876490959472,
0.033325));
#38293=CARTESIAN_POINT('Ctrl Pts',(-0.0834548326657697,0.0446455583417202,
0.033325));
#38294=CARTESIAN_POINT('Ctrl Pts',(-0.0800249269923783,0.0489205910950087,
0.033325));
#38295=CARTESIAN_POINT('Ctrl Pts',(-0.0781132858485567,0.051303259681428,
0.033325));
#38296=CARTESIAN_POINT('Ctrl Pts',(-0.0760836906850449,0.0535904891565725,
0.033325));
#38297=CARTESIAN_POINT('Ctrl Pts',(-0.0739470307071451,0.0557748355204373,
0.033325));
#38298=CARTESIAN_POINT('Ctrl Pts',(-0.0705067602284846,0.059291886613499,
0.033325));
#38299=CARTESIAN_POINT('Ctrl Pts',(-0.0667883681472276,0.0625435339072888,
0.033325));
#38300=CARTESIAN_POINT('Ctrl Pts',(-0.0628308692529389,0.0654950879562435,
0.033325));
#38301=CARTESIAN_POINT('Ctrl Pts',(-0.0606814402551841,0.0670981600052135,
0.033325));
#38302=CARTESIAN_POINT('Ctrl Pts',(-0.0584651587268817,0.0686094986793821,
0.033325));
#38303=CARTESIAN_POINT('Ctrl Pts',(-0.0561952079986995,0.0700200058301,
0.033325));
#38304=CARTESIAN_POINT('Ctrl Pts',(-0.0501333136738915,0.0737867595247431,
0.033325));
#38305=CARTESIAN_POINT('Ctrl Pts',(-0.0436751701263957,0.0768486853796021,
0.033325));
#38306=CARTESIAN_POINT('Ctrl Pts',(-0.0369436491597186,0.0790891055682764,
0.033325));
#38307=CARTESIAN_POINT('Ctrl Pts',(-0.0333356887224549,0.0802899259242701,
0.033325));
#38308=CARTESIAN_POINT('Ctrl Pts',(-0.0296423557823287,0.0812543742145633,
0.033325));
#38309=CARTESIAN_POINT('Ctrl Pts',(-0.0259190414490983,0.0819530919554474,
0.033325));
#38310=CARTESIAN_POINT('Ctrl Pts',(-0.0231274480643262,0.0824769627997288,
0.033325));
#38311=CARTESIAN_POINT('Ctrl Pts',(-0.0203161830499112,0.0828528623331501,
0.033325));
#38312=CARTESIAN_POINT('Ctrl Pts',(-0.0174934788191478,0.0830727961543361,
0.033325));
#38313=CARTESIAN_POINT('Ctrl Pts',(-0.0126601868498688,0.0834493869285754,
0.033325));
#38314=CARTESIAN_POINT('Ctrl Pts',(-0.00779291433087069,0.0833692530579157,
0.0333249999999999));
#38315=CARTESIAN_POINT('Ctrl Pts',(-0.00294800581945059,0.0828496701715294,
0.0333249999999999));
#38316=CARTESIAN_POINT('Ctrl Pts',(0.000101264618999113,0.0825226570335005,
0.0333249999999999));
#38317=CARTESIAN_POINT('Ctrl Pts',(0.00314435587318879,0.0820201134909955,
0.0333249999999999));
#38318=CARTESIAN_POINT('Ctrl Pts',(0.00614210873778604,0.0813512661027619,
0.0333249999999999));
#38319=CARTESIAN_POINT('Ctrl Pts',(0.0106275580743664,0.0803504894512721,
0.0333249999999999));
#38320=CARTESIAN_POINT('Ctrl Pts',(0.0150235960594789,0.0789773917259045,
0.0333249999999999));
#38321=CARTESIAN_POINT('Ctrl Pts',(0.0192810923841575,0.0772484640679705,
0.033325));
#38322=CARTESIAN_POINT('Ctrl Pts',(0.0225362012762144,0.0759265961522092,
0.033325));
#38323=CARTESIAN_POINT('Ctrl Pts',(0.0257102610124195,0.0743964750603324,
0.033325));
#38324=CARTESIAN_POINT('Ctrl Pts',(0.0287775749945677,0.0726622576048804,
0.033325));
#38325=CARTESIAN_POINT('Ctrl Pts',(0.0308073950195533,0.0715146250706033,
0.033325));
#38326=CARTESIAN_POINT('Ctrl Pts',(0.0327876490113005,0.0702787831601469,
0.033325));
#38327=CARTESIAN_POINT('Ctrl Pts',(0.0347028232812334,0.0689622789254883,
0.033325));
#38328=CARTESIAN_POINT('Ctrl Pts',(0.0397377314622753,0.0655012477047154,
0.033325));
#38329=CARTESIAN_POINT('Ctrl Pts',(0.0443444553862968,0.0614742134119748,
0.033325));
#38330=CARTESIAN_POINT('Ctrl Pts',(0.0483819446640243,0.0569075936409299,
0.033325));
#38331=CARTESIAN_POINT('Ctrl Pts',(0.0495941607609181,0.0555365113632898,
0.0333249999999999));
#38332=CARTESIAN_POINT('Ctrl Pts',(0.0507547452462496,0.0541166472553641,
0.033325));
#38333=CARTESIAN_POINT('Ctrl Pts',(0.051858976480955,0.0526484240822815,
0.033325));
#38334=CARTESIAN_POINT('Origin',(0.,0.,0.033325));
#38335=CARTESIAN_POINT('Origin',(0.,0.,-0.0517230892635719));
#38336=CARTESIAN_POINT('Ctrl Pts',(0.0518589764809551,0.0526484240822814,
0.033325));
#38337=CARTESIAN_POINT('Ctrl Pts',(0.034560993232641,0.0696870291702574,
0.0354166557997537));
#38338=CARTESIAN_POINT('Ctrl Pts',(-0.0178308073244973,0.085128264632029,
0.0395999673992612));
#38339=CARTESIAN_POINT('Ctrl Pts',(-0.0679537005351042,0.0429705670053581,
0.0445839376447373));
#38340=CARTESIAN_POINT('Ctrl Pts',(-0.0738777383652924,0.0093611306850835,
0.0474762520904596));
#38341=CARTESIAN_POINT('Ctrl Pts',(-0.0738258018559393,4.09328341953522E-5,
0.0482769107364281));
#38342=CARTESIAN_POINT('Ctrl Pts',(0.0678412253220073,0.0688739702050683,
0.0201758476192062));
#38343=CARTESIAN_POINT('Ctrl Pts',(0.045212233027951,0.0911636474294266,
0.02226750341896));
#38344=CARTESIAN_POINT('Ctrl Pts',(-0.0233260256846517,0.111363666891765,
0.0264508150184675));
#38345=CARTESIAN_POINT('Ctrl Pts',(-0.105880745319823,0.0419279921909746,
0.0327257824177288));
#38346=CARTESIAN_POINT('Ctrl Pts',(-0.0933501081980039,-0.0650449563313979,
0.0390007498169901));
#38347=CARTESIAN_POINT('Ctrl Pts',(0.00262407842631599,-0.113778593381263,
0.0452757172162514));
#38348=CARTESIAN_POINT('Ctrl Pts',(0.0963221634673791,-0.0606354881256659,
0.0515506846155127));
#38349=CARTESIAN_POINT('Ctrl Pts',(0.103735822611175,0.0467997517633499,
0.057825652014774));
#38350=CARTESIAN_POINT('Ctrl Pts',(0.0182857197834144,0.112331107839639,
0.0641006194140354));
#38351=CARTESIAN_POINT('Ctrl Pts',(-0.0835478711919389,0.0772822483167664,
0.0703755868132966));
#38352=CARTESIAN_POINT('Ctrl Pts',(-0.11056795310426,-0.026964309214831,
0.076650554212558));
#38353=CARTESIAN_POINT('Ctrl Pts',(-0.0385895394868932,-0.107067331885508,
0.0829255216118192));
#38354=CARTESIAN_POINT('Ctrl Pts',(0.0679430878111881,-0.0913033084985679,
0.0892004890110805));
#38355=CARTESIAN_POINT('Ctrl Pts',(0.113639378289663,0.00621271467693868,
0.0954754564103418));
#38356=CARTESIAN_POINT('Ctrl Pts',(0.0575844881496173,0.0981660422492194,
0.101750423809603));
#38357=CARTESIAN_POINT('Ctrl Pts',(-0.0500310870203194,0.102222289415193,
0.108025391208864));
#38358=CARTESIAN_POINT('Ctrl Pts',(-0.112849420354528,0.0147501067708153,
0.114300358608126));
#38359=CARTESIAN_POINT('Ctrl Pts',(-0.0746231935625905,-0.0859298847748101,
0.120575326007387));
#38360=CARTESIAN_POINT('Ctrl Pts',(0.0304191741242974,-0.109667771340055,
0.126850293406648));
#38361=CARTESIAN_POINT('Ctrl Pts',(0.108225920969254,-0.0352128203351555,
0.13312526080591));
#38362=CARTESIAN_POINT('Ctrl Pts',(0.089125584578444,0.0707762354892434,
0.139400228205171));
#38363=CARTESIAN_POINT('Ctrl Pts',(-0.00977177477518579,0.113383641129007,
0.145675195604432));
#38364=CARTESIAN_POINT('Ctrl Pts',(-0.0999293420097319,0.0544862202834464,
0.151950163003694));
#38365=CARTESIAN_POINT('Ctrl Pts',(-0.100592616842759,-0.0532313773645962,
0.158225130402955));
#38366=CARTESIAN_POINT('Ctrl Pts',(-0.0112216609370024,-0.113221744247947,
0.164500097802216));
#38367=CARTESIAN_POINT('Ctrl Pts',(0.0882648350855844,-0.0719583743977188,
0.170775065201478));
#38368=CARTESIAN_POINT('Ctrl Pts',(0.108586899430732,0.0339831583264558,
0.177050032600739));
#38369=CARTESIAN_POINT('Ctrl Pts',(0.0575098468247979,0.0839498311266844,
0.181233344200246));
#38370=CARTESIAN_POINT('Ctrl Pts',(0.0270116869336335,0.0928246971123492,
0.183325));
#38371=CARTESIAN_POINT('Ctrl Pts',(0.0625138090416566,0.063465454830806,
0.0245588984128041));
#38372=CARTESIAN_POINT('Ctrl Pts',(0.0416618197628477,0.0840047746763702,
0.0266505542125579));
#38373=CARTESIAN_POINT('Ctrl Pts',(-0.0214942862312669,0.102618532805186,
0.0308338658120654));
#38374=CARTESIAN_POINT('Ctrl Pts',(-0.0975661725255505,0.0386354828481611,
0.0371088332113267));
#38375=CARTESIAN_POINT('Ctrl Pts',(-0.0860195376809465,-0.059937124660171,
0.043383800610588));
#38376=CARTESIAN_POINT('Ctrl Pts',(0.00241801554842842,-0.104843820640091,
0.0496587680098493));
#38377=CARTESIAN_POINT('Ctrl Pts',(0.0887582042467272,-0.0558739219087465,
0.0559337354091106));
#38378=CARTESIAN_POINT('Ctrl Pts',(0.095589685692049,0.0431246742824077,
0.062208702808372));
#38379=CARTESIAN_POINT('Ctrl Pts',(0.0168497840259201,0.103510002827837,
0.0684836702076332));
#38380=CARTESIAN_POINT('Ctrl Pts',(-0.0769870479305082,0.0712134500910467,
0.0747586376068947));
#38381=CARTESIAN_POINT('Ctrl Pts',(-0.101885304601719,-0.0248468636761093,
0.0810336050061557));
#38382=CARTESIAN_POINT('Ctrl Pts',(-0.0355591912003177,-0.0986595791618033,
0.0873085724054173));
#38383=CARTESIAN_POINT('Ctrl Pts',(0.0626076725025084,-0.0841334684811387,
0.0935835398046782));
#38384=CARTESIAN_POINT('Ctrl Pts',(0.104715537791268,0.00572484440104077,
0.0998585072039399));
#38385=CARTESIAN_POINT('Ctrl Pts',(0.0530625099835711,0.0904572874445442,
0.106133474603201));
#38386=CARTESIAN_POINT('Ctrl Pts',(-0.0461022601712969,0.0941950067966907,
0.112408442002462));
#38387=CARTESIAN_POINT('Ctrl Pts',(-0.103987613446247,0.0135918146177068,
0.118683409401724));
#38388=CARTESIAN_POINT('Ctrl Pts',(-0.0687632048257988,-0.0791820074340765,
0.124958376800985));
#38389=CARTESIAN_POINT('Ctrl Pts',(0.0280304259450684,-0.101055812052856,
0.131233344200246));
#38390=CARTESIAN_POINT('Ctrl Pts',(0.0997271868943474,-0.0324476380814423,
0.137508311599508));
#38391=CARTESIAN_POINT('Ctrl Pts',(0.0821267562402867,0.0652183395724518,
0.143783278998769));
#38392=CARTESIAN_POINT('Ctrl Pts',(-0.00900441964888684,0.104479883085,
0.15005824639803));
#38393=CARTESIAN_POINT('Ctrl Pts',(-0.0920821193073042,0.0502075420075893,
0.156333213797291));
#38394=CARTESIAN_POINT('Ctrl Pts',(-0.0926933086845182,-0.0490512390334914,
0.162608181196553));
#38395=CARTESIAN_POINT('Ctrl Pts',(-0.0103404495661197,-0.104330699595772,
0.168883148595814));
#38396=CARTESIAN_POINT('Ctrl Pts',(0.0813335994366777,-0.0663076478158446,
0.175158115995075));
#38397=CARTESIAN_POINT('Ctrl Pts',(0.100059818542758,0.0313145386182065,
0.181433083394337));
#38398=CARTESIAN_POINT('Ctrl Pts',(0.0529937300712946,0.0773574428708091,
0.185616394993844));
#38399=CARTESIAN_POINT('Ctrl Pts',(0.0248905209310009,0.0855353859263006,
0.187708050793598));
#38400=CARTESIAN_POINT('Ctrl Pts',(0.0571863927613058,0.0580569394565437,
0.028941949206402));
#38401=CARTESIAN_POINT('Ctrl Pts',(0.0381114064977443,0.0768459019233138,
0.0310336050061558));
#38402=CARTESIAN_POINT('Ctrl Pts',(-0.0196625467778821,0.0938733987186076,
0.0352169166056633));
#38403=CARTESIAN_POINT('Ctrl Pts',(-0.0892515997312777,0.0353429735053478,
0.0414918840049247));
#38404=CARTESIAN_POINT('Ctrl Pts',(-0.0786889671638893,-0.0548292929889441,
0.0477668514041859));
#38405=CARTESIAN_POINT('Ctrl Pts',(0.00221195267054096,-0.0959090478989199,
0.0540418188034473));
#38406=CARTESIAN_POINT('Ctrl Pts',(0.0811942450260753,-0.0511123556918271,
0.0603167862027086));
#38407=CARTESIAN_POINT('Ctrl Pts',(0.0874435487729231,0.0394495968014654,
0.0665917536019698));
#38408=CARTESIAN_POINT('Ctrl Pts',(0.0154138482684258,0.0946888978160358,
0.0728667210012312));
#38409=CARTESIAN_POINT('Ctrl Pts',(-0.0704262246690777,0.0651446518653269,
0.0791416884004924));
#38410=CARTESIAN_POINT('Ctrl Pts',(-0.0932026560991779,-0.0227294181373876,
0.0854166557997538));
#38411=CARTESIAN_POINT('Ctrl Pts',(-0.0325288429137424,-0.0902518264380986,
0.091691623199015));
#38412=CARTESIAN_POINT('Ctrl Pts',(0.0572722571938289,-0.0769636284637097,
0.0979665905982764));
#38413=CARTESIAN_POINT('Ctrl Pts',(0.0957916972928727,0.00523697412514306,
0.104241557997538));
#38414=CARTESIAN_POINT('Ctrl Pts',(0.0485405318175249,0.0827485326398688,
0.110516525396799));
#38415=CARTESIAN_POINT('Ctrl Pts',(-0.0421734333222743,0.0861677241781889,
0.11679149279606));
#38416=CARTESIAN_POINT('Ctrl Pts',(-0.0951258065379651,0.0124335224645981,
0.123066460195321));
#38417=CARTESIAN_POINT('Ctrl Pts',(-0.0629032160890072,-0.0724341300933428,
0.129341427594583));
#38418=CARTESIAN_POINT('Ctrl Pts',(0.0256416777658396,-0.092443852765658,
0.135616394993844));
#38419=CARTESIAN_POINT('Ctrl Pts',(0.0912284528194409,-0.029682455827729,
0.141891362393105));
#38420=CARTESIAN_POINT('Ctrl Pts',(0.0751279279021295,0.05966044365566,
0.148166329792367));
#38421=CARTESIAN_POINT('Ctrl Pts',(-0.00823706452258799,0.0955761250409928,
0.154441297191628));
#38422=CARTESIAN_POINT('Ctrl Pts',(-0.0842348966048762,0.0459288637317318,
0.160716264590889));
#38423=CARTESIAN_POINT('Ctrl Pts',(-0.0847940005262773,-0.0448711007023865,
0.166991231990151));
#38424=CARTESIAN_POINT('Ctrl Pts',(-0.00945923819523702,-0.0954396549435973,
0.173266199389412));
#38425=CARTESIAN_POINT('Ctrl Pts',(0.0744023637877709,-0.0606569212339703,
0.179541166788673));
#38426=CARTESIAN_POINT('Ctrl Pts',(0.0915327376547826,0.0286459189099571,
0.185816134187935));
#38427=CARTESIAN_POINT('Ctrl Pts',(0.0484776133177914,0.0707650546149338,
0.189999445787442));
#38428=CARTESIAN_POINT('Ctrl Pts',(0.0227693549283683,0.078246074740252,
0.192091101587196));
#38429=CARTESIAN_POINT('Ctrl Pts',(0.0518589764809551,0.0526484240822814,
0.033325));
#38430=CARTESIAN_POINT('Ctrl Pts',(0.034560993232641,0.0696870291702574,
0.0354166557997537));
#38431=CARTESIAN_POINT('Ctrl Pts',(-0.0178308073244973,0.085128264632029,
0.0395999673992612));
#38432=CARTESIAN_POINT('Ctrl Pts',(-0.0809370269370047,0.0320504641625344,
0.0458749347985226));
#38433=CARTESIAN_POINT('Ctrl Pts',(-0.071358396646832,-0.0497214613177173,
0.0521499021977838));
#38434=CARTESIAN_POINT('Ctrl Pts',(0.00200588979265343,-0.0869742751577483,
0.0584248695970452));
#38435=CARTESIAN_POINT('Ctrl Pts',(0.0736302858054235,-0.0463507894749077,
0.0646998369963064));
#38436=CARTESIAN_POINT('Ctrl Pts',(0.079297411853797,0.0357745193205231,
0.0709748043955678));
#38437=CARTESIAN_POINT('Ctrl Pts',(0.0139779125109316,0.0858677928042342,
0.077249771794829));
#38438=CARTESIAN_POINT('Ctrl Pts',(-0.0638654014076472,0.0590758536396072,
0.0835247391940904));
#38439=CARTESIAN_POINT('Ctrl Pts',(-0.0845200075966366,-0.0206119725986659,
0.0897997065933516));
#38440=CARTESIAN_POINT('Ctrl Pts',(-0.0294984946271671,-0.081844073714394,
0.0960746739926129));
#38441=CARTESIAN_POINT('Ctrl Pts',(0.0519368418851493,-0.0697937884462804,
0.102349641391874));
#38442=CARTESIAN_POINT('Ctrl Pts',(0.0868678567944775,0.00474910384924522,
0.108624608791136));
#38443=CARTESIAN_POINT('Ctrl Pts',(0.0440185536514787,0.0750397778351934,
0.114899576190397));
#38444=CARTESIAN_POINT('Ctrl Pts',(-0.0382446064732518,0.078140441559687,
0.121174543589658));
#38445=CARTESIAN_POINT('Ctrl Pts',(-0.0862639996296835,0.0112752303114895,
0.127449510988919));
#38446=CARTESIAN_POINT('Ctrl Pts',(-0.0570432273522154,-0.0656862527526091,
0.133724478388181));
#38447=CARTESIAN_POINT('Ctrl Pts',(0.0232529295866107,-0.0838318934784593,
0.139999445787442));
#38448=CARTESIAN_POINT('Ctrl Pts',(0.0827297187445345,-0.0269172735740158,
0.146274413186704));
#38449=CARTESIAN_POINT('Ctrl Pts',(0.0681290995639721,0.0541025477388684,
0.152549380585964));
#38450=CARTESIAN_POINT('Ctrl Pts',(-0.00746970939628905,0.0866723669969857,
0.158824347985226));
#38451=CARTESIAN_POINT('Ctrl Pts',(-0.0763876739024484,0.0416501854558747,
0.165099315384487));
#38452=CARTESIAN_POINT('Ctrl Pts',(-0.0768946923680362,-0.0406909623712818,
0.171374282783749));
#38453=CARTESIAN_POINT('Ctrl Pts',(-0.00857802682435435,-0.0865486102914224,
0.17764925018301));
#38454=CARTESIAN_POINT('Ctrl Pts',(0.0674711281388642,-0.0550061946520962,
0.183924217582271));
#38455=CARTESIAN_POINT('Ctrl Pts',(0.0830056567668076,0.0259772992017078,
0.190199184981532));
#38456=CARTESIAN_POINT('Ctrl Pts',(0.0439614965642881,0.0641726663590585,
0.19438249658104));
#38457=CARTESIAN_POINT('Ctrl Pts',(0.0206481889257357,0.0709567635542034,
0.196474152380794));
#38458=CARTESIAN_POINT('Ctrl Pts',(0.0270116869336335,0.0928246971123492,
0.183325));
#38459=CARTESIAN_POINT('Ctrl Pts',(0.0575098468247979,0.0839498311266844,
0.181233344200246));
#38460=CARTESIAN_POINT('Ctrl Pts',(0.083048373127765,0.0589664947265702,
0.179141688400492));
#38461=CARTESIAN_POINT('Ctrl Pts',(0.0924306255550574,0.0288179044058174,
0.177050032600739));
#38462=CARTESIAN_POINT('Ctrl Pts',(0.10181287798235,-0.00133068591493571,
0.174958376800985));
#38463=CARTESIAN_POINT('Ctrl Pts',(0.095038856533967,-0.0366445301563275,
0.172866721001231));
#38464=CARTESIAN_POINT('Ctrl Pts',(0.0750707631393444,-0.0611786805853946,
0.170775065201477));
#38465=CARTESIAN_POINT('Ctrl Pts',(0.055102669744722,-0.0857128310144614,
0.168683409401724));
#38466=CARTESIAN_POINT('Ctrl Pts',(0.02194050440386,-0.0994672876312039,
0.16659175360197));
#38467=CARTESIAN_POINT('Ctrl Pts',(-0.00953573758419697,-0.0963461214590169,
0.164500097802216));
#38468=CARTESIAN_POINT('Ctrl Pts',(-0.0410119795722545,-0.0932249552868299,
0.162408442002462));
#38469=CARTESIAN_POINT('Ctrl Pts',(-0.070802298207507,-0.073228166325713,
0.160316786202709));
#38470=CARTESIAN_POINT('Ctrl Pts',(-0.0855869117196286,-0.0452768389038139,
0.158225130402955));
#38471=CARTESIAN_POINT('Ctrl Pts',(-0.092884710370865,-0.0314798492569381,
0.157192673053848));
#38472=CARTESIAN_POINT('Ctrl Pts',(-0.0965263909752696,-0.0157447479797163,
0.156160215704741));
#38473=CARTESIAN_POINT('Ctrl Pts',(-0.0965227763075221,-6.77612820726425E-6,
0.155127758355634));
#38474=CARTESIAN_POINT('Origin',(0.,0.,0.1025));
#38475=CARTESIAN_POINT('Origin',(0.,0.,0.183325));
#38476=CARTESIAN_POINT('Origin',(0.,0.,0.0975096189432334));
#38477=CARTESIAN_POINT('',(0.,0.,0.0840192378864668));
#38478=CARTESIAN_POINT('',(-0.0400285208940887,4.90207999875487E-18,0.11));
#38479=CARTESIAN_POINT('',(-0.0207846096908265,-2.54538057293978E-18,0.0975096189432334));
#38480=CARTESIAN_POINT('Origin',(0.,0.,0.11));
#38481=CARTESIAN_POINT('Origin',(0.,0.0519615242270663,0.2));
#38482=CARTESIAN_POINT('',(3.18172571617472E-18,0.0519615242270663,0.2));
#38483=CARTESIAN_POINT('',(0.045,0.0259807621135332,0.2));
#38484=CARTESIAN_POINT('',(0.01125,0.045466333698683,0.2));
#38485=CARTESIAN_POINT('',(0.,0.0519615242270663,0.11));
#38486=CARTESIAN_POINT('',(3.18172571617472E-18,0.0519615242270663,0.2));
#38487=CARTESIAN_POINT('',(0.045,0.0259807621135332,0.11));
#38488=CARTESIAN_POINT('',(0.045,0.0259807621135332,0.11));
#38489=CARTESIAN_POINT('',(0.045,0.0259807621135332,0.2));
#38490=CARTESIAN_POINT('Origin',(-0.045,0.0259807621135332,0.2));
#38491=CARTESIAN_POINT('',(-0.045,0.0259807621135332,0.2));
#38492=CARTESIAN_POINT('',(-0.03375,0.0324759526419164,0.2));
#38493=CARTESIAN_POINT('',(-0.045,0.0259807621135332,0.11));
#38494=CARTESIAN_POINT('',(-0.045,0.0259807621135332,0.2));
#38495=CARTESIAN_POINT('',(3.18172571617472E-18,0.0519615242270663,0.11));
#38496=CARTESIAN_POINT('Origin',(-0.045,-0.0259807621135332,0.2));
#38497=CARTESIAN_POINT('',(-0.045,-0.0259807621135332,0.2));
#38498=CARTESIAN_POINT('',(-0.045,-0.0129903810567666,0.2));
#38499=CARTESIAN_POINT('',(-0.045,-0.0259807621135332,0.11));
#38500=CARTESIAN_POINT('',(-0.045,-0.0259807621135332,0.2));
#38501=CARTESIAN_POINT('',(-0.045,0.0259807621135332,0.11));
#38502=CARTESIAN_POINT('Origin',(-6.93889390390723E-18,-0.0519615242270663,
0.2));
#38503=CARTESIAN_POINT('',(-9.54517714852416E-18,-0.0519615242270663,0.2));
#38504=CARTESIAN_POINT('',(-0.01125,-0.045466333698683,0.2));
#38505=CARTESIAN_POINT('',(-6.93889390390723E-18,-0.0519615242270663,0.11));
#38506=CARTESIAN_POINT('',(-9.54517714852416E-18,-0.0519615242270663,0.2));
#38507=CARTESIAN_POINT('',(-0.045,-0.0259807621135332,0.11));
#38508=CARTESIAN_POINT('Origin',(0.045,-0.0259807621135332,0.2));
#38509=CARTESIAN_POINT('',(0.045,-0.0259807621135332,0.2));
#38510=CARTESIAN_POINT('',(0.03375,-0.0324759526419165,0.2));
#38511=CARTESIAN_POINT('',(0.045,-0.0259807621135332,0.11));
#38512=CARTESIAN_POINT('',(0.045,-0.0259807621135332,0.2));
#38513=CARTESIAN_POINT('',(-9.54517714852416E-18,-0.0519615242270663,0.11));
#38514=CARTESIAN_POINT('Origin',(0.045,0.0259807621135332,0.2));
#38515=CARTESIAN_POINT('',(0.045,0.0129903810567666,0.2));
#38516=CARTESIAN_POINT('',(0.045,-0.0259807621135332,0.11));
#38517=CARTESIAN_POINT('Origin',(0.,0.,0.11));
#38518=CARTESIAN_POINT('Origin',(0.07,0.,0.));
#38519=CARTESIAN_POINT('',(-0.07,-8.57252759403147E-18,8.67361737988404E-18));
#38520=CARTESIAN_POINT('Origin',(0.,0.,0.));
#38521=CARTESIAN_POINT('Origin',(0.,0.,0.0125));
#38522=CARTESIAN_POINT('',(-0.085,-1.04094977927525E-17,0.0125));
#38523=CARTESIAN_POINT('Origin',(0.,0.,0.19));
#38524=CARTESIAN_POINT('',(-0.08,-9.79717439317883E-18,0.2));
#38525=CARTESIAN_POINT('Origin',(0.,0.,0.2));
#38526=CARTESIAN_POINT('',(-0.09,-1.10218211923262E-17,0.19));
#38527=CARTESIAN_POINT('Origin',(0.,0.,0.2));
#38528=CARTESIAN_POINT('',(0.,0.,0.));
#38529=CARTESIAN_POINT('Origin',(0.,0.,-0.19));
#38530=CARTESIAN_POINT('',(-0.12155579423589,0.000100027207062599,-0.324010734985006));
#38531=CARTESIAN_POINT('',(-0.121567991859644,0.000104017427664388,-0.330489265014994));
#38532=CARTESIAN_POINT('',(-0.1215,-1.48794586096403E-17,-0.19));
#38533=CARTESIAN_POINT('',(-0.0374782951795791,-0.115758143579925,-0.36));
#38534=CARTESIAN_POINT('Ctrl Pts',(-0.12155579423589,0.000100027207062599,
-0.324010734985006));
#38535=CARTESIAN_POINT('Ctrl Pts',(-0.121620634124682,0.0074842758651267,
-0.32444665059017));
#38536=CARTESIAN_POINT('Ctrl Pts',(-0.121004234176155,0.0148576610554614,
-0.324882566195334));
#38537=CARTESIAN_POINT('Ctrl Pts',(-0.119667279374296,0.022097896271274,
-0.325318481800499));
#38538=CARTESIAN_POINT('Ctrl Pts',(-0.11243718511193,0.0612522364323941,
-0.327675862103401));
#38539=CARTESIAN_POINT('Ctrl Pts',(-0.0841343262472267,0.0965125801032592,
-0.330033242406302));
#38540=CARTESIAN_POINT('Ctrl Pts',(-0.0474717895588589,0.112047042615882,
-0.332390622709205));
#38541=CARTESIAN_POINT('Ctrl Pts',(-0.0108092528704911,0.127581505128506,
-0.334748003012107));
#38542=CARTESIAN_POINT('Ctrl Pts',(0.0342129616415417,0.123390086482887,
-0.337105383315009));
#38543=CARTESIAN_POINT('Ctrl Pts',(0.0673711970604704,0.101343025426172,
-0.339462763617911));
#38544=CARTESIAN_POINT('Ctrl Pts',(0.100529432479399,0.079295964369458,
-0.341820143920814));
#38545=CARTESIAN_POINT('Ctrl Pts',(0.121823688805224,0.0393932609016481,
-0.344177524223715));
#38546=CARTESIAN_POINT('Ctrl Pts',(0.121689461571731,-0.000417576977033936,
-0.346534904526618));
#38547=CARTESIAN_POINT('Ctrl Pts',(0.121555234338239,-0.0402284148557158,
-0.34889228482952));
#38548=CARTESIAN_POINT('Ctrl Pts',(0.0999925235454301,-0.0799473871452696,
-0.351249665132422));
#38549=CARTESIAN_POINT('Ctrl Pts',(0.0666859483039566,-0.101778801767896,
-0.353607045435324));
#38550=CARTESIAN_POINT('Ctrl Pts',(0.036578032614443,-0.121513595455792,
-0.355738030290216));
#38551=CARTESIAN_POINT('Ctrl Pts',(-0.00312637396201031,-0.126631583500994,
-0.357869015145108));
#38552=CARTESIAN_POINT('Ctrl Pts',(-0.0374782951795791,-0.115758143579925,
-0.36));
#38553=CARTESIAN_POINT('',(-0.1215,-1.48794586096403E-17,-0.36));
#38554=CARTESIAN_POINT('Origin',(0.,0.,-0.36));
#38555=CARTESIAN_POINT('',(-0.1215,-1.48794586096403E-17,-0.3835));
#38556=CARTESIAN_POINT('',(-0.1215,-1.48794586096403E-17,-0.19));
#38557=CARTESIAN_POINT('Origin',(0.,0.,-0.3835));
#38558=CARTESIAN_POINT('',(0.0677908815531582,-0.100829789141135,-0.36));
#38559=CARTESIAN_POINT('Origin',(0.,0.,-0.36));
#38560=CARTESIAN_POINT('Ctrl Pts',(0.0677908815531583,-0.100829789141135,
-0.36));
#38561=CARTESIAN_POINT('Ctrl Pts',(0.100979247033071,-0.07851625886049,
-0.357642619697098));
#38562=CARTESIAN_POINT('Ctrl Pts',(0.12202917251289,-0.0387425950814313,
-0.355285239394196));
#38563=CARTESIAN_POINT('Ctrl Pts',(0.121678176144516,0.00100886688157746,
-0.352927859091294));
#38564=CARTESIAN_POINT('Ctrl Pts',(0.121327179776142,0.0407603288445865,
-0.350570478788391));
#38565=CARTESIAN_POINT('Ctrl Pts',(0.0995752615595766,0.0804895889915456,
-0.348213098485489));
#38566=CARTESIAN_POINT('Ctrl Pts',(0.0661601753453354,0.102160099321753,
-0.345855718182587));
#38567=CARTESIAN_POINT('Ctrl Pts',(0.0327450891310943,0.123830609651961,
-0.343498337879685));
#38568=CARTESIAN_POINT('Ctrl Pts',(-0.012333165080822,0.127442370165417,
-0.341140957576783));
#38569=CARTESIAN_POINT('Ctrl Pts',(-0.0488096494985592,0.111460993500232,
-0.338783577273881));
#38570=CARTESIAN_POINT('Ctrl Pts',(-0.0852861339162964,0.0954796168350458,
-0.336426196970979));
#38571=CARTESIAN_POINT('Ctrl Pts',(-0.113160848539854,0.0599051029912176,
-0.334068816668076));
#38572=CARTESIAN_POINT('Ctrl Pts',(-0.11992145607908,0.0206722787223513,
-0.331711436365174));
#38573=CARTESIAN_POINT('Ctrl Pts',(-0.121089789820009,0.0138922619739541,
-0.331304045915114));
#38574=CARTESIAN_POINT('Ctrl Pts',(-0.12162755094405,0.00700298981783844,
-0.330896655465054));
#38575=CARTESIAN_POINT('Ctrl Pts',(-0.121567991859644,0.000104017427664388,
-0.330489265014994));
#38576=CARTESIAN_POINT('Origin',(0.,0.,-0.19));
#38577=CARTESIAN_POINT('',(-0.121316684751533,-2.98164701347942E-5,-0.279010734985006));
#38578=CARTESIAN_POINT('',(-0.1213134883411,-2.23347955230942E-5,-0.285489265014994));
#38579=CARTESIAN_POINT('',(-0.1215,-1.48794586096403E-17,-0.19));
#38580=CARTESIAN_POINT('Ctrl Pts',(-0.121316684751533,-2.98164701347942E-5,
-0.279010734985006));
#38581=CARTESIAN_POINT('Ctrl Pts',(-0.121267388452722,0.0219598511007976,
-0.280302368772757));
#38582=CARTESIAN_POINT('Ctrl Pts',(-0.115545772107405,0.0439734214389766,
-0.281594002560508));
#38583=CARTESIAN_POINT('Ctrl Pts',(-0.104309833231411,0.0626737375079338,
-0.282885636348259));
#38584=CARTESIAN_POINT('Ctrl Pts',(-0.0838029517592271,0.0968039663522564,
-0.285243016651162));
#38585=CARTESIAN_POINT('Ctrl Pts',(-0.0449276135031733,0.119897595955311,
-0.287600396954064));
#38586=CARTESIAN_POINT('Ctrl Pts',(-0.00514607383054742,0.1215814300281,
-0.289957777256966));
#38587=CARTESIAN_POINT('Ctrl Pts',(0.0346354658420782,0.123265264100889,
-0.292315157559868));
#38588=CARTESIAN_POINT('Ctrl Pts',(0.075323206931276,0.103539302643412,
-0.29467253786277));
#38589=CARTESIAN_POINT('Ctrl Pts',(0.0986407780548691,0.0712639068871239,
-0.297029918165672));
#38590=CARTESIAN_POINT('Ctrl Pts',(0.121958349178462,0.0389885111308361,
-0.299387298468575));
#38591=CARTESIAN_POINT('Ctrl Pts',(0.127905750336451,-0.00583631892426194,
-0.301744678771477));
#38592=CARTESIAN_POINT('Ctrl Pts',(0.113811504451575,-0.0430753921798633,
-0.304102059074379));
#38593=CARTESIAN_POINT('Ctrl Pts',(0.0997172585667,-0.0803144654354648,
-0.306459439377281));
#38594=CARTESIAN_POINT('Ctrl Pts',(0.0655813656389605,-0.109967781891569,
-0.308816819680183));
#38595=CARTESIAN_POINT('Ctrl Pts',(0.0267371682304334,-0.118716443260442,
-0.311174199983086));
#38596=CARTESIAN_POINT('Ctrl Pts',(-0.0121070291780935,-0.127465104629315,
-0.313531580285988));
#38597=CARTESIAN_POINT('Ctrl Pts',(-0.0556595310674075,-0.115309110910955,
-0.315888960588889));
#38598=CARTESIAN_POINT('Ctrl Pts',(-0.0843571171820498,-0.0877069457260886,
-0.318246340891792));
#38599=CARTESIAN_POINT('Ctrl Pts',(-0.107748081534174,-0.0652088422514121,
-0.32016780558953));
#38600=CARTESIAN_POINT('Ctrl Pts',(-0.121269987635155,-0.0324488720470692,
-0.322089270287268));
#38601=CARTESIAN_POINT('Ctrl Pts',(-0.12155579423589,0.000100027207062599,
-0.324010734985006));
#38602=CARTESIAN_POINT('Ctrl Pts',(-0.121567991859644,0.000104017427664388,
-0.330489265014994));
#38603=CARTESIAN_POINT('Ctrl Pts',(-0.121282910041409,-0.0329181757874598,
-0.328539275162152));
#38604=CARTESIAN_POINT('Ctrl Pts',(-0.107312657409089,-0.0661626105376077,
-0.32658928530931));
#38605=CARTESIAN_POINT('Ctrl Pts',(-0.0833038297687421,-0.0887116572214725,
-0.324639295456468));
#38606=CARTESIAN_POINT('Ctrl Pts',(-0.0542790954642872,-0.115971634202525,
-0.322281915153566));
#38607=CARTESIAN_POINT('Ctrl Pts',(-0.0105831264004852,-0.127600453470727,
-0.319924534850663));
#38608=CARTESIAN_POINT('Ctrl Pts',(0.0281540805652533,-0.118386890783788,
-0.317567154547761));
#38609=CARTESIAN_POINT('Ctrl Pts',(0.0668912875309918,-0.10917332809685,
-0.315209774244859));
#38610=CARTESIAN_POINT('Ctrl Pts',(0.100669732398667,-0.0791173834547723,
-0.312852393941957));
#38611=CARTESIAN_POINT('Ctrl Pts',(0.114317861247938,-0.0417133069274287,
-0.310495013639055));
#38612=CARTESIAN_POINT('Ctrl Pts',(0.127965990097209,-0.00430923040008524,
-0.308137633336153));
#38613=CARTESIAN_POINT('Ctrl Pts',(0.121483802928076,0.0404429780125239,
-0.30578025303325));
#38614=CARTESIAN_POINT('Ctrl Pts',(0.0977823489008379,0.0724378514980737,
-0.303422872730348));
#38615=CARTESIAN_POINT('Ctrl Pts',(0.0740808948735994,0.104432724983624,
-0.301065492427446));
#38616=CARTESIAN_POINT('Ctrl Pts',(0.0331601739882546,0.123670263542114,
-0.298708112124544));
#38617=CARTESIAN_POINT('Ctrl Pts',(-0.00659845091904251,0.121511023160459,
-0.296350731821642));
#38618=CARTESIAN_POINT('Ctrl Pts',(-0.0463570758263398,0.119351782778803,
-0.29399335151874));
#38619=CARTESIAN_POINT('Ctrl Pts',(-0.0849536047555895,0.095795763457001,
-0.291635971215837));
#38620=CARTESIAN_POINT('Ctrl Pts',(-0.105051198646726,0.0614230580704297,
-0.289278590912935));
#38621=CARTESIAN_POINT('Ctrl Pts',(-0.115819696333789,0.0430058086992691,
-0.288015482280288));
#38622=CARTESIAN_POINT('Ctrl Pts',(-0.12127728535159,0.0214831680352748,
-0.286752373647641));
#38623=CARTESIAN_POINT('Ctrl Pts',(-0.1213134883411,-2.23347955230942E-5,
-0.285489265014994));
#38624=CARTESIAN_POINT('Origin',(0.,0.,-0.19));
#38625=CARTESIAN_POINT('',(-0.121652121442684,-5.9196348637991E-5,-0.234010734985006));
#38626=CARTESIAN_POINT('',(-0.121642193667188,-6.59388428620122E-5,-0.240489265014994));
#38627=CARTESIAN_POINT('',(-0.1215,-1.48794586096403E-17,-0.19));
#38628=CARTESIAN_POINT('Ctrl Pts',(-0.121652121442684,-5.9196348637991E-5,
-0.234010734985006));
#38629=CARTESIAN_POINT('Ctrl Pts',(-0.121432098146049,0.0362408929853419,
-0.236158086955344));
#38630=CARTESIAN_POINT('Ctrl Pts',(-0.104092725076878,0.0727236629989947,
-0.238305438925682));
#38631=CARTESIAN_POINT('Ctrl Pts',(-0.0756934135126743,0.0952840140834343,
-0.240452790896021));
#38632=CARTESIAN_POINT('Ctrl Pts',(-0.0445164203498382,0.12005094936356,
-0.242810171198923));
#38633=CARTESIAN_POINT('Ctrl Pts',(-1.01824319385865E-5,0.128038828451523,
-0.245167551501825));
#38634=CARTESIAN_POINT('Ctrl Pts',(0.0378337200468045,0.11565961062334,
-0.247524931804727));
#38635=CARTESIAN_POINT('Ctrl Pts',(0.0756776225255475,0.103280392795157,
-0.249882312107629));
#38636=CARTESIAN_POINT('Ctrl Pts',(0.106859189565134,0.0705340780508277,
-0.252239692410531));
#38637=CARTESIAN_POINT('Ctrl Pts',(0.117372096756334,0.032129847839524,
-0.254597072713433));
#38638=CARTESIAN_POINT('Ctrl Pts',(0.127885003947534,-0.00627438237177978,
-0.256954453016336));
#38639=CARTESIAN_POINT('Ctrl Pts',(0.117729251290347,-0.0503365280500584,
-0.259311833319238));
#38640=CARTESIAN_POINT('Ctrl Pts',(0.0914666612543121,-0.0802644782613266,
-0.26166921362214));
#38641=CARTESIAN_POINT('Ctrl Pts',(0.0652040712182769,-0.110192428472595,
-0.264026593925042));
#38642=CARTESIAN_POINT('Ctrl Pts',(0.0228346438033933,-0.125986183216853,
-0.266383974227944));
#38643=CARTESIAN_POINT('Ctrl Pts',(-0.0166098666488376,-0.120551428846724,
-0.268741354530847));
#38644=CARTESIAN_POINT('Ctrl Pts',(-0.0560543771010683,-0.115116674476596,
-0.271098734833749));
#38645=CARTESIAN_POINT('Ctrl Pts',(-0.0925739705906463,-0.0884534109920819,
-0.273456115136651));
#38646=CARTESIAN_POINT('Ctrl Pts',(-0.109764554991278,-0.0525383652070299,
-0.275813495439553));
#38647=CARTESIAN_POINT('Ctrl Pts',(-0.117536235019243,-0.0363015557114269,
-0.276879241954704));
#38648=CARTESIAN_POINT('Ctrl Pts',(-0.121357359871034,-0.0181738227707557,
-0.277944988469855));
#38649=CARTESIAN_POINT('Ctrl Pts',(-0.121316684751533,-2.98164701347942E-5,
-0.279010734985006));
#38650=CARTESIAN_POINT('Ctrl Pts',(-0.1213134883411,-2.23347955230942E-5,
-0.285489265014994));
#38651=CARTESIAN_POINT('Ctrl Pts',(-0.121344852156353,-0.0186532441995837,
-0.284394993344739));
#38652=CARTESIAN_POINT('Ctrl Pts',(-0.117307295164673,-0.0372712911205606,
-0.283300721674484));
#38653=CARTESIAN_POINT('Ctrl Pts',(-0.109128983929891,-0.0538461772364694,
-0.282206450004229));
#38654=CARTESIAN_POINT('Ctrl Pts',(-0.0915105164688954,-0.0895533157054566,
-0.279849069701327));
#38655=CARTESIAN_POINT('Ctrl Pts',(-0.0546749226938819,-0.11577820119209,
-0.277491689398425));
#38656=CARTESIAN_POINT('Ctrl Pts',(-0.0151682872483324,-0.12074124246499,
-0.275134309095522));
#38657=CARTESIAN_POINT('Ctrl Pts',(0.0243383481972172,-0.12570428373789,
-0.27277692879262));
#38658=CARTESIAN_POINT('Ctrl Pts',(0.0665160253133027,-0.109405480797056,
-0.270419548489718));
#38659=CARTESIAN_POINT('Ctrl Pts',(0.0924191474222124,-0.0791658908688873,
-0.268062168186816));
#38660=CARTESIAN_POINT('Ctrl Pts',(0.118322269531122,-0.048926300940719,
-0.265704787883913));
#38661=CARTESIAN_POINT('Ctrl Pts',(0.127950836632856,-0.00474592402521655,
-0.263347407581011));
#38662=CARTESIAN_POINT('Ctrl Pts',(0.116979816901966,0.0335299595321455,
-0.260990027278109));
#38663=CARTESIAN_POINT('Ctrl Pts',(0.106008797171075,0.0718058430895075,
-0.258632646975207));
#38664=CARTESIAN_POINT('Ctrl Pts',(0.0744381906075608,0.104177233288729,
-0.256275266672305));
#38665=CARTESIAN_POINT('Ctrl Pts',(0.0364490799724483,0.116103391967299,
-0.253917886369403));
#38666=CARTESIAN_POINT('Ctrl Pts',(-0.0015400306626643,0.128029550645869,
-0.2515605060665));
#38667=CARTESIAN_POINT('Ctrl Pts',(-0.0459476453693751,0.119510477803787,
-0.249203125763598));
#38668=CARTESIAN_POINT('Ctrl Pts',(-0.0768264879290973,0.0943728019139746,
-0.246845745460696));
#38669=CARTESIAN_POINT('Ctrl Pts',(-0.104580567132348,0.0717789159455437,
-0.244726918645462));
#38670=CARTESIAN_POINT('Ctrl Pts',(-0.121405405335243,0.0357596639627758,
-0.242608091830228));
#38671=CARTESIAN_POINT('Ctrl Pts',(-0.121642193667188,-6.59388428620122E-5,
-0.240489265014994));
#38672=CARTESIAN_POINT('Origin',(0.,0.,-0.19));
#38673=CARTESIAN_POINT('',(-0.121452836205038,0.000103164027536851,-0.189010734985006));
#38674=CARTESIAN_POINT('',(-0.121466423015182,0.000104460321887741,-0.195489265014994));
#38675=CARTESIAN_POINT('',(-0.1215,-1.48794586096403E-17,-0.19));
#38676=CARTESIAN_POINT('Ctrl Pts',(-0.121452836205038,0.000103164027536851,
-0.189010734985006));
#38677=CARTESIAN_POINT('Ctrl Pts',(-0.121544980016008,0.0110647321231586,
-0.189656424835029));
#38678=CARTESIAN_POINT('Ctrl Pts',(-0.120180324762459,0.0220037716634773,
-0.190302114685052));
#38679=CARTESIAN_POINT('Ctrl Pts',(-0.117266460944003,0.0325132779165323,
-0.190947804535075));
#38680=CARTESIAN_POINT('Ctrl Pts',(-0.106628094597184,0.0708829425988793,
-0.193305184837977));
#38681=CARTESIAN_POINT('Ctrl Pts',(-0.075339670468586,0.103527175985459,
-0.19566256514088));
#38682=CARTESIAN_POINT('Ctrl Pts',(-0.0374555115366707,0.115782644476787,
-0.198019945443782));
#38683=CARTESIAN_POINT('Ctrl Pts',(0.000428647395244536,0.128038112968116,
-0.200377325746684));
#38684=CARTESIAN_POINT('Ctrl Pts',(0.0449085411304768,0.119904816564194,
-0.202734706049586));
#38685=CARTESIAN_POINT('Ctrl Pts',(0.0760044228399103,0.09503611844497,
-0.205092086352488));
#38686=CARTESIAN_POINT('Ctrl Pts',(0.107100304549344,0.0701674203257461,
-0.20744946665539));
#38687=CARTESIAN_POINT('Ctrl Pts',(0.124812174232979,0.0285633204912204,
-0.209806846958292));
#38688=CARTESIAN_POINT('Ctrl Pts',(0.121184107483162,-0.0110882007938326,
-0.212164227261195));
#38689=CARTESIAN_POINT('Ctrl Pts',(0.117556040733344,-0.0507397220788855,
-0.214521607564097));
#38690=CARTESIAN_POINT('Ctrl Pts',(0.0925880375500753,-0.0884386648144661,
-0.216878987866999));
#38691=CARTESIAN_POINT('Ctrl Pts',(0.0574953761353696,-0.107251190394802,
-0.219236368169901));
#38692=CARTESIAN_POINT('Ctrl Pts',(0.0224027147206637,-0.126063715975137,
-0.221593748472803));
#38693=CARTESIAN_POINT('Ctrl Pts',(-0.0228146049254789,-0.125989824400228,
-0.223951128775705));
#38694=CARTESIAN_POINT('Ctrl Pts',(-0.057845594568456,-0.107062707165432,
-0.226308509078608));
#38695=CARTESIAN_POINT('Ctrl Pts',(-0.0928765842114331,-0.0881355899306356,
-0.22866588938151));
#38696=CARTESIAN_POINT('Ctrl Pts',(-0.117721243851244,-0.0503552470359518,
-0.231023269684412));
#38697=CARTESIAN_POINT('Ctrl Pts',(-0.121219699467264,-0.0106920798524657,
-0.233380649987314));
#38698=CARTESIAN_POINT('Ctrl Pts',(-0.121531390711429,-0.00715833145493331,
-0.233590678319878));
#38699=CARTESIAN_POINT('Ctrl Pts',(-0.121673641494709,-0.00360963770154739,
-0.233800706652442));
#38700=CARTESIAN_POINT('Ctrl Pts',(-0.121652121442684,-5.9196348637991E-5,
-0.234010734985006));
#38701=CARTESIAN_POINT('Ctrl Pts',(-0.121642193667188,-6.59388428620122E-5,
-0.240489265014994));
#38702=CARTESIAN_POINT('Ctrl Pts',(-0.121668853081737,-0.00409945514332142,
-0.240250711527326));
#38703=CARTESIAN_POINT('Ctrl Pts',(-0.121485243156111,-0.00813051675591712,
-0.240012158039658));
#38704=CARTESIAN_POINT('Ctrl Pts',(-0.121083287896919,-0.0121396872446064,
-0.23977360455199));
#38705=CARTESIAN_POINT('Ctrl Pts',(-0.117111174892285,-0.0517582215758337,
-0.237416224249088));
#38706=CARTESIAN_POINT('Ctrl Pts',(-0.0918168784702831,-0.0892390113007461,
-0.235058843946185));
#38707=CARTESIAN_POINT('Ctrl Pts',(-0.0565622442669608,-0.107746214874363,
-0.232701463643283));
#38708=CARTESIAN_POINT('Ctrl Pts',(-0.0213076100636385,-0.12625341844798,
-0.230344083340381));
#38709=CARTESIAN_POINT('Ctrl Pts',(0.0239073619210042,-0.125787035870301,
-0.227986703037479));
#38710=CARTESIAN_POINT('Ctrl Pts',(0.058772738544517,-0.106556556759136,
-0.225629322734577));
#38711=CARTESIAN_POINT('Ctrl Pts',(0.0936381151680299,-0.0873260776479714,
-0.223271942431675));
#38712=CARTESIAN_POINT('Ctrl Pts',(0.118153896430413,-0.0493315020033205,
-0.220914562128773));
#38713=CARTESIAN_POINT('Ctrl Pts',(0.121307935605703,-0.00963946391216232,
-0.21855718182587));
#38714=CARTESIAN_POINT('Ctrl Pts',(0.124461974780992,0.0300525741789959,
-0.216199801522968));
#38715=CARTESIAN_POINT('Ctrl Pts',(0.106254271869187,0.0714420747166612,
-0.213842421220066));
#38716=CARTESIAN_POINT('Ctrl Pts',(0.0748634727914798,0.0959374531295166,
-0.211485040917164));
#38717=CARTESIAN_POINT('Ctrl Pts',(0.0434726737137725,0.120432831542372,
-0.209127660614262));
#38718=CARTESIAN_POINT('Ctrl Pts',(-0.00110122152983763,0.128034087830417,
-0.20677028031136));
#38719=CARTESIAN_POINT('Ctrl Pts',(-0.0388362420289081,0.115326843441258,
-0.204412900008457));
#38720=CARTESIAN_POINT('Ctrl Pts',(-0.0765712625279784,0.1026195990521,
-0.202055519705555));
#38721=CARTESIAN_POINT('Ctrl Pts',(-0.107467408282509,0.0696038539857373,
-0.199698139402653));
#38722=CARTESIAN_POINT('Ctrl Pts',(-0.117646562232706,0.0311098198818689,
-0.197340759099751));
#38723=CARTESIAN_POINT('Ctrl Pts',(-0.120311475668384,0.021032040414268,
-0.196723594404832));
#38724=CARTESIAN_POINT('Ctrl Pts',(-0.121556450581511,0.0105787800990859,
-0.196106429709913));
#38725=CARTESIAN_POINT('Ctrl Pts',(-0.121466423015182,0.000104460321887741,
-0.195489265014994));
#38726=CARTESIAN_POINT('Origin',(0.,0.,-0.19));
#38727=CARTESIAN_POINT('',(-0.121366189046343,-7.72277758326612E-5,-0.144010734985006));
#38728=CARTESIAN_POINT('',(-0.121356940814226,-7.17826249269161E-5,-0.150489265014994));
#38729=CARTESIAN_POINT('',(-0.1215,-1.48794586096403E-17,-0.19));
#38730=CARTESIAN_POINT('Ctrl Pts',(-0.121366189046343,-7.72277758326612E-5,
-0.144010734985006));
#38731=CARTESIAN_POINT('Ctrl Pts',(-0.121214006322019,0.0254575835671733,
-0.145512143017616));
#38732=CARTESIAN_POINT('Ctrl Pts',(-0.113325331544467,0.0510784255672011,
-0.147013551050226));
#38733=CARTESIAN_POINT('Ctrl Pts',(-0.0984073400571069,0.0715858330918497,
-0.148514959082836));
#38734=CARTESIAN_POINT('Ctrl Pts',(-0.0749844073650329,0.10378478068783,
-0.150872339385738));
#38735=CARTESIAN_POINT('Ctrl Pts',(-0.0342324172038069,0.123377808882716,
-0.15322971968864));
#38736=CARTESIAN_POINT('Ctrl Pts',(0.00554340599624446,0.121564002764019,
-0.155587099991543));
#38737=CARTESIAN_POINT('Ctrl Pts',(0.0453192291962959,0.119750196645322,
-0.157944480294445));
#38738=CARTESIAN_POINT('Ctrl Pts',(0.0841188854351726,0.0965295562130407,
-0.160301860597347));
#38739=CARTESIAN_POINT('Ctrl Pts',(0.104514111104929,0.0623324689329835,
-0.162659240900249));
#38740=CARTESIAN_POINT('Ctrl Pts',(0.124909336774685,0.0281353816529263,
-0.165016621203151));
#38741=CARTESIAN_POINT('Ctrl Pts',(0.126900131875321,-0.0170381524749071,
-0.167374001506053));
#38742=CARTESIAN_POINT('Ctrl Pts',(0.109592259115638,-0.0528968131577431,
-0.169731381808956));
#38743=CARTESIAN_POINT('Ctrl Pts',(0.0922843863559539,-0.0887554738405791,
-0.172088762111858));
#38744=CARTESIAN_POINT('Ctrl Pts',(0.0556778457359505,-0.115299261078418,
-0.17444614241476));
#38745=CARTESIAN_POINT('Ctrl Pts',(0.0162157838364738,-0.120605076431635,
-0.176803522717662));
#38746=CARTESIAN_POINT('Ctrl Pts',(-0.0232462780630026,-0.125910891784852,
-0.179160903020564));
#38747=CARTESIAN_POINT('Ctrl Pts',(-0.0655638612419521,-0.109978735253448,
-0.181518283323466));
#38748=CARTESIAN_POINT('Ctrl Pts',(-0.0917284985489071,-0.0799651089986894,
-0.183875663626369));
#38749=CARTESIAN_POINT('Ctrl Pts',(-0.110726604126622,-0.0581722580728937,
-0.185587354079248));
#38750=CARTESIAN_POINT('Ctrl Pts',(-0.121208567719907,-0.0289553870046511,
-0.187299044532127));
#38751=CARTESIAN_POINT('Ctrl Pts',(-0.121452836205038,0.000103164027536851,
-0.189010734985006));
#38752=CARTESIAN_POINT('Ctrl Pts',(-0.121466423015182,0.000104460321887741,
-0.195489265014994));
#38753=CARTESIAN_POINT('Ctrl Pts',(-0.121212572823547,-0.0294299166594152,
-0.193749049407011));
#38754=CARTESIAN_POINT('Ctrl Pts',(-0.110344552537344,-0.0591317305671495,
-0.192008833799028));
#38755=CARTESIAN_POINT('Ctrl Pts',(-0.0907664982302483,-0.081055396453563,
-0.190268618191044));
#38756=CARTESIAN_POINT('Ctrl Pts',(-0.0642451181317306,-0.110754255543751,
-0.187911237888142));
#38757=CARTESIAN_POINT('Ctrl Pts',(-0.0217401957888325,-0.126179650582752,
-0.18555385758524));
#38758=CARTESIAN_POINT('Ctrl Pts',(0.0176556515372683,-0.120402709563575,
-0.183196477282338));
#38759=CARTESIAN_POINT('Ctrl Pts',(0.057051498863369,-0.114625768544397,
-0.180839096979436));
#38760=CARTESIAN_POINT('Ctrl Pts',(0.0933382711726726,-0.087646491467041,
-0.178481716676534));
#38761=CARTESIAN_POINT('Ctrl Pts',(0.110216457309932,-0.0515835927033183,
-0.176124336373631));
#38762=CARTESIAN_POINT('Ctrl Pts',(0.127094643447192,-0.0155206939395955,
-0.173766956070729));
#38763=CARTESIAN_POINT('Ctrl Pts',(0.124564243412408,0.0296258265104934,
-0.171409575767827));
#38764=CARTESIAN_POINT('Ctrl Pts',(0.103761877546585,0.06357678244565,-0.169052195464925));
#38765=CARTESIAN_POINT('Ctrl Pts',(0.0829595116807615,0.0975277383808065,
-0.166694815162023));
#38766=CARTESIAN_POINT('Ctrl Pts',(0.0438851799838995,0.12028312980103,
-0.164337434859121));
#38767=CARTESIAN_POINT('Ctrl Pts',(0.00409052634720552,0.121621552759611,
-0.161980054556218));
#38768=CARTESIAN_POINT('Ctrl Pts',(-0.0357041272894885,0.122959975718192,
-0.159622674253316));
#38769=CARTESIAN_POINT('Ctrl Pts',(-0.0762191028660145,0.102881430215129,
-0.157265293950414));
#38770=CARTESIAN_POINT('Ctrl Pts',(-0.0992556394140983,0.0704049184341864,
-0.154907913647512));
#38771=CARTESIAN_POINT('Ctrl Pts',(-0.113648785991654,0.0501137087110959,
-0.153435030770006));
#38772=CARTESIAN_POINT('Ctrl Pts',(-0.121218863464572,0.0249826971880121,
-0.1519621478925));
#38773=CARTESIAN_POINT('Ctrl Pts',(-0.121356940814226,-7.17826249269161E-5,
-0.150489265014994));
#38774=CARTESIAN_POINT('Origin',(0.,0.,-0.19));
#38775=CARTESIAN_POINT('',(-0.121690333780732,-6.67349754346347E-8,-0.0990107349850059));
#38776=CARTESIAN_POINT('',(-0.121689496210452,-8.68452866517571E-6,-0.105489265014994));
#38777=CARTESIAN_POINT('',(-0.1215,-1.48794586096403E-17,-0.19));
#38778=CARTESIAN_POINT('Ctrl Pts',(-0.121690333780732,-6.67349754346347E-8,
-0.0990107349850059));
#38779=CARTESIAN_POINT('Ctrl Pts',(-0.121689956805147,0.0398128076349811,
-0.101367861200203));
#38780=CARTESIAN_POINT('Ctrl Pts',(-0.100266142222434,0.0796260065197837,
-0.1037249874154));
#38781=CARTESIAN_POINT('Ctrl Pts',(-0.0670395400323943,0.101559020964777,
-0.106082113630597));
#38782=CARTESIAN_POINT('Ctrl Pts',(-0.0338093561626619,0.123494399691016,
-0.108439493933499));
#38783=CARTESIAN_POINT('Ctrl Pts',(0.011226160027391,0.127545738961227,
-0.110796874236402));
#38784=CARTESIAN_POINT('Ctrl Pts',(0.0478376930952209,0.111893215660743,
-0.113154254539304));
#38785=CARTESIAN_POINT('Ctrl Pts',(0.0844492261630509,0.0962406923602585,
-0.115511634842206));
#38786=CARTESIAN_POINT('Ctrl Pts',(0.112636776108658,0.0608843064890792,
-0.117869015145108));
#38787=CARTESIAN_POINT('Ctrl Pts',(0.119738884453224,0.0217056621430117,
-0.12022639544801));
#38788=CARTESIAN_POINT('Ctrl Pts',(0.126840992797791,-0.0174729822030555,
-0.122583775750912));
#38789=CARTESIAN_POINT('Ctrl Pts',(0.112857659541317,-0.0604738850240109,
-0.124941156053815));
#38790=CARTESIAN_POINT('Ctrl Pts',(0.0840700051746493,-0.0879816465636836,
-0.127298536356717));
#38791=CARTESIAN_POINT('Ctrl Pts',(0.0552823508079815,-0.115489408103357,
-0.129655916659619));
#38792=CARTESIAN_POINT('Ctrl Pts',(0.0116903753311198,-0.127504028361747,
-0.132013296962521));
#38793=CARTESIAN_POINT('Ctrl Pts',(-0.0271250162488584,-0.118628705137298,
-0.134370677265423));
#38794=CARTESIAN_POINT('Ctrl Pts',(-0.0659404078288361,-0.109753381912849,
-0.136728057568325));
#38795=CARTESIAN_POINT('Ctrl Pts',(-0.0999792155119305,-0.079988115205563,
-0.139085437871228));
#38796=CARTESIAN_POINT('Ctrl Pts',(-0.113951681742017,-0.0427030483533834,
-0.14144281817413));
#38797=CARTESIAN_POINT('Ctrl Pts',(-0.11902512857867,-0.0291647222368194,
-0.142298790444422));
#38798=CARTESIAN_POINT('Ctrl Pts',(-0.121452950399159,-0.014634956229408,
-0.143154762714714));
#38799=CARTESIAN_POINT('Ctrl Pts',(-0.121366189046343,-7.72277758326612E-5,
-0.144010734985006));
#38800=CARTESIAN_POINT('Ctrl Pts',(-0.121356940814226,-7.17826249269161E-5,
-0.150489265014994));
#38801=CARTESIAN_POINT('Ctrl Pts',(-0.121439859192964,-0.0151175294576353,
-0.149604767589598));
#38802=CARTESIAN_POINT('Ctrl Pts',(-0.118842607042299,-0.0301356769858909,
-0.148720270164202));
#38803=CARTESIAN_POINT('Ctrl Pts',(-0.113433312185074,-0.044061527265631,
-0.147835772738805));
#38804=CARTESIAN_POINT('Ctrl Pts',(-0.0990163508883235,-0.0811769831256851,
-0.145478392435903));
#38805=CARTESIAN_POINT('Ctrl Pts',(-0.0646243307751811,-0.110533416786971,
-0.143121012133001));
#38806=CARTESIAN_POINT('Ctrl Pts',(-0.0257056668506945,-0.118944328174207,
-0.140763631830099));
#38807=CARTESIAN_POINT('Ctrl Pts',(0.0132129970737924,-0.127355239561444,
-0.138406251527197));
#38808=CARTESIAN_POINT('Ctrl Pts',(0.0566583048096238,-0.11482062867463,
-0.136048871224295));
#38809=CARTESIAN_POINT('Ctrl Pts',(0.0851152312342714,-0.0869708680151885,
-0.133691490921392));
#38810=CARTESIAN_POINT('Ctrl Pts',(0.113572157658919,-0.0591211073557473,
-0.13133411061849));
#38811=CARTESIAN_POINT('Ctrl Pts',(0.127040702772383,-0.0159561969236791,
-0.128976730315588));
#38812=CARTESIAN_POINT('Ctrl Pts',(0.119470984035321,0.0231347893671651,
-0.126619350012686));
#38813=CARTESIAN_POINT('Ctrl Pts',(0.11190126529826,0.0622257756580095,
-0.124261969709784));
#38814=CARTESIAN_POINT('Ctrl Pts',(0.0832932827106712,0.0972428378076296,
-0.121904589406882));
#38815=CARTESIAN_POINT('Ctrl Pts',(0.0464973428307525,0.112456799234482,
-0.11954720910398));
#38816=CARTESIAN_POINT('Ctrl Pts',(0.00970140295083383,0.127670760661335,
-0.117189828801077));
#38817=CARTESIAN_POINT('Ctrl Pts',(-0.035282494221415,0.12308162136542,
-0.114832448498175));
#38818=CARTESIAN_POINT('Ctrl Pts',(-0.0682482114436531,0.100750761441342,
-0.112475068195273));
#38819=CARTESIAN_POINT('Ctrl Pts',(-0.100811478378532,0.0786925199145164,
-0.11014646713518));
#38820=CARTESIAN_POINT('Ctrl Pts',(-0.121648213577836,0.0393231005841258,
-0.107817866075087));
#38821=CARTESIAN_POINT('Ctrl Pts',(-0.121689496210452,-8.6845286651757E-6,
-0.105489265014994));
#38822=CARTESIAN_POINT('Origin',(0.,0.,-0.19));
#38823=CARTESIAN_POINT('',(-0.121366197770921,7.70029837308187E-5,-0.0540107349850059));
#38824=CARTESIAN_POINT('',(-0.121376290077639,8.23099624828544E-5,-0.060489265014994));
#38825=CARTESIAN_POINT('',(-0.1215,-1.48794586096403E-17,-0.19));
#38826=CARTESIAN_POINT('Ctrl Pts',(-0.121366197770921,7.70029837308187E-5,
-0.0540107349850059));
#38827=CARTESIAN_POINT('Ctrl Pts',(-0.121453181762923,0.0146263535592494,
-0.0548661990798879));
#38828=CARTESIAN_POINT('Ctrl Pts',(-0.119028488418249,0.0291477473845937,
-0.0557216631747699));
#38829=CARTESIAN_POINT('Ctrl Pts',(-0.113961010341666,0.042679265103465,
-0.0565771272696519));
#38830=CARTESIAN_POINT('Ctrl Pts',(-0.0999966919388308,0.0799677188558563,
-0.0589345075725541));
#38831=CARTESIAN_POINT('Ctrl Pts',(-0.0659637531736886,0.1097393107365,
-0.0612918878754562));
#38832=CARTESIAN_POINT('Ctrl Pts',(-0.0271501406182937,0.118622678817329,
-0.0636492681783583));
#38833=CARTESIAN_POINT('Ctrl Pts',(0.0116634719371012,0.127506046898158,
-0.0660066484812605));
#38834=CARTESIAN_POINT('Ctrl Pts',(0.0552577582827487,0.115501191179173,
-0.0683640287841626));
#38835=CARTESIAN_POINT('Ctrl Pts',(0.0840512087018202,0.0879996720036106,
-0.0707214090870648));
#38836=CARTESIAN_POINT('Ctrl Pts',(0.112844659120892,0.0604981528280479,
-0.0730787893899669));
#38837=CARTESIAN_POINT('Ctrl Pts',(0.126837273613388,0.0174999701959076,
-0.0754361696928691));
#38838=CARTESIAN_POINT('Ctrl Pts',(0.119743536518744,-0.0216802440500727,
-0.0777935499957713));
#38839=CARTESIAN_POINT('Ctrl Pts',(0.112649799424101,-0.0608604582960528,
-0.0801509302986735));
#38840=CARTESIAN_POINT('Ctrl Pts',(0.0844697107423188,-0.096222704155873,
-0.0825083106015756));
#38841=CARTESIAN_POINT('Ctrl Pts',(0.0478614929616094,-0.111882991089053,
-0.0848656909044778));
#38842=CARTESIAN_POINT('Ctrl Pts',(0.0112532751809,-0.127543278022233,-0.0872230712073799));
#38843=CARTESIAN_POINT('Ctrl Pts',(-0.0337830716987367,-0.123501606028772,
-0.0895804515102821));
#38844=CARTESIAN_POINT('Ctrl Pts',(-0.0670179132089846,-0.10157331338049,
-0.0919378318131843));
#38845=CARTESIAN_POINT('Ctrl Pts',(-0.100256336900943,-0.0796426572147265,
-0.0942954662037915));
#38846=CARTESIAN_POINT('Ctrl Pts',(-0.121690710837589,-0.0398215244059149,
-0.0966531005943987));
#38847=CARTESIAN_POINT('Ctrl Pts',(-0.121690333780732,-6.67349754346347E-8,
-0.0990107349850059));
#38848=CARTESIAN_POINT('Ctrl Pts',(-0.121689496210452,-8.6845286651757E-6,
-0.105489265014994));
#38849=CARTESIAN_POINT('Ctrl Pts',(-0.121690006423613,-0.000494787113293386,
-0.105460485772185));
#38850=CARTESIAN_POINT('Ctrl Pts',(-0.121687340224093,-0.000980883949462602,
-0.105431706529376));
#38851=CARTESIAN_POINT('Ctrl Pts',(-0.121681480491707,-0.00146694228632414,
-0.105402927286567));
#38852=CARTESIAN_POINT('Ctrl Pts',(-0.121201495045295,-0.0412812055376695,
-0.103045546983664));
#38853=CARTESIAN_POINT('Ctrl Pts',(-0.0992939868802457,-0.0808371514881188,
-0.100688166680762));
#38854=CARTESIAN_POINT('Ctrl Pts',(-0.0657995057974866,-0.102366791614373,
-0.0983307863778601));
#38855=CARTESIAN_POINT('Ctrl Pts',(-0.0323050247147275,-0.123896431740628,
-0.0959734060749579));
#38856=CARTESIAN_POINT('Ctrl Pts',(0.0127764292857409,-0.127399766042687,
-0.0936160257720558));
#38857=CARTESIAN_POINT('Ctrl Pts',(0.0491949030024557,-0.111303165164919,
-0.0912586454691537));
#38858=CARTESIAN_POINT('Ctrl Pts',(0.0856133767191708,-0.0952065642871499,
-0.0889012651662515));
#38859=CARTESIAN_POINT('Ctrl Pts',(0.113368870152132,-0.0595100282295526,
-0.0865438848633493));
#38860=CARTESIAN_POINT('Ctrl Pts',(0.119993991851324,-0.0202479052800325,
-0.0841865045604471));
#38861=CARTESIAN_POINT('Ctrl Pts',(0.126619113550515,0.0190142176694876,
-0.081829124257545));
#38862=CARTESIAN_POINT('Ctrl Pts',(0.112113863515937,0.0618419275109303,
-0.0794717439546429));
#38863=CARTESIAN_POINT('Ctrl Pts',(0.0829938194035347,0.0889975450679775,
-0.0771143636517407));
#38864=CARTESIAN_POINT('Ctrl Pts',(0.0538737752911323,0.116153162625025,
-0.0747569833488385));
#38865=CARTESIAN_POINT('Ctrl Pts',(0.0101389371009058,0.127636687897676,
-0.0723996030459363));
#38866=CARTESIAN_POINT('Ctrl Pts',(-0.0285656586709824,0.118290015279103,
-0.0700422227430341));
#38867=CARTESIAN_POINT('Ctrl Pts',(-0.0672702544428707,0.10894334266053,
-0.0676848424401319));
#38868=CARTESIAN_POINT('Ctrl Pts',(-0.100944607796421,0.0787664721507315,
-0.0653274621372298));
#38869=CARTESIAN_POINT('Ctrl Pts',(-0.114462590277186,0.0413141787233953,
-0.0629700818343277));
#38870=CARTESIAN_POINT('Ctrl Pts',(-0.119204526097562,0.0281763919263629,
-0.0621431428945498));
#38871=CARTESIAN_POINT('Ctrl Pts',(-0.121466186405048,0.0141433520392691,
-0.0613162039547719));
#38872=CARTESIAN_POINT('Ctrl Pts',(-0.121376290077639,8.23099624828544E-5,
-0.060489265014994));
#38873=CARTESIAN_POINT('Origin',(0.,0.,-0.19));
#38874=CARTESIAN_POINT('',(-0.12142737051279,-0.000153818344799855,-0.00901073498500596));
#38875=CARTESIAN_POINT('',(-0.121436917850398,-0.000108937277296349,-0.015489265014994));
#38876=CARTESIAN_POINT('',(-0.1215,-1.48794586096403E-17,-0.19));
#38877=CARTESIAN_POINT('Ctrl Pts',(-0.12142737051279,-0.000153818344799855,
-0.00901073498500596));
#38878=CARTESIAN_POINT('Ctrl Pts',(-0.121186248580763,0.0289004463450801,
-0.010721917262475));
#38879=CARTESIAN_POINT('Ctrl Pts',(-0.110736371434051,0.058159765361451,
-0.012433099539944));
#38880=CARTESIAN_POINT('Ctrl Pts',(-0.0917563917866803,0.0799663543477724,
-0.014144281817413));
#38881=CARTESIAN_POINT('Ctrl Pts',(-0.0656089551521823,0.110007819846043,
-0.0165016621203151));
#38882=CARTESIAN_POINT('Ctrl Pts',(-0.023272481971744,0.12590496306751,
-0.0188590424232173));
#38883=CARTESIAN_POINT('Ctrl Pts',(0.0161960346634556,0.120596967837864,
-0.0212164227261194));
#38884=CARTESIAN_POINT('Ctrl Pts',(0.0556645512986556,0.115288972608218,
-0.0235738030290216));
#38885=CARTESIAN_POINT('Ctrl Pts',(0.092265111388617,0.0887758389274579,
-0.0259311833319238));
#38886=CARTESIAN_POINT('Ctrl Pts',(0.109577856214941,0.0529262964459767,
-0.028288563634826));
#38887=CARTESIAN_POINT('Ctrl Pts',(0.126890601041264,0.0170767539644958,
-0.0306459439377282));
#38888=CARTESIAN_POINT('Ctrl Pts',(0.124915530603951,-0.0281091973177056,
-0.0330033242406303));
#38889=CARTESIAN_POINT('Ctrl Pts',(0.104529032480174,-0.0623134685653849,
-0.0353607045435324));
#38890=CARTESIAN_POINT('Ctrl Pts',(0.0841425343563973,-0.0965177398130642,
-0.0377180848464346));
#38891=CARTESIAN_POINT('Ctrl Pts',(0.0453446085461563,-0.119740331026221,
-0.0400754651493368));
#38892=CARTESIAN_POINT('Ctrl Pts',(0.00556841104745733,-0.121561109575771,
-0.0424328454522389));
#38893=CARTESIAN_POINT('Ctrl Pts',(-0.0342077864512416,-0.12338188812532,
-0.0447902257551411));
#38894=CARTESIAN_POINT('Ctrl Pts',(-0.0749622556383988,-0.103800854011263,
-0.0471476060580432));
#38895=CARTESIAN_POINT('Ctrl Pts',(-0.0983916412117136,-0.0716076791421647,
-0.0495049863609454));
#38896=CARTESIAN_POINT('Ctrl Pts',(-0.113318793140995,-0.0510970084353631,
-0.0510069025689656));
#38897=CARTESIAN_POINT('Ctrl Pts',(-0.121213482223646,-0.0254669158975791,
-0.0525088187769857));
#38898=CARTESIAN_POINT('Ctrl Pts',(-0.121366197770921,7.70029837308187E-5,
-0.0540107349850059));
#38899=CARTESIAN_POINT('Ctrl Pts',(-0.121376290077639,8.23099624828544E-5,
-0.060489265014994));
#38900=CARTESIAN_POINT('Ctrl Pts',(-0.121209916175962,-0.0259408936475976,
-0.0589588236518697));
#38901=CARTESIAN_POINT('Ctrl Pts',(-0.112988979946086,-0.0520600104833506,
-0.0574283822887454));
#38902=CARTESIAN_POINT('Ctrl Pts',(-0.0975294472722496,-0.0727774231105138,
-0.0558979409256212));
#38903=CARTESIAN_POINT('Ctrl Pts',(-0.0737167101785676,-0.104689015172212,
-0.053540560622719));
#38904=CARTESIAN_POINT('Ctrl Pts',(-0.0327296243832231,-0.123784482950735,
-0.0511831803198168));
#38905=CARTESIAN_POINT('Ctrl Pts',(0.00702127041893494,-0.121487324712238,
-0.0488258000169147));
#38906=CARTESIAN_POINT('Ctrl Pts',(0.046772165221093,-0.119190166473741,
-0.0464684197140125));
#38907=CARTESIAN_POINT('Ctrl Pts',(0.0852868690300645,-0.0955003822182252,
-0.0441110394111104));
#38908=CARTESIAN_POINT('Ctrl Pts',(0.105264570463262,-0.0610573524762343,
-0.0417536591082082));
#38909=CARTESIAN_POINT('Ctrl Pts',(0.12524227189646,-0.0266143227342432,
-0.039396278805306));
#38910=CARTESIAN_POINT('Ctrl Pts',(0.126682970953884,0.0185819524942231,
-0.0370388985024038));
#38911=CARTESIAN_POINT('Ctrl Pts',(0.10894056031447,0.0542266326955117,
-0.0346815181995016));
#38912=CARTESIAN_POINT('Ctrl Pts',(0.0911981496750572,0.0898713128967998,
-0.0323241378965995));
#38913=CARTESIAN_POINT('Ctrl Pts',(0.0542726293388079,0.115964398070911,
-0.0299667575936974));
#38914=CARTESIAN_POINT('Ctrl Pts',(0.0147484614780834,0.120791518932237,
-0.0276093772907952));
#38915=CARTESIAN_POINT('Ctrl Pts',(-0.0247757063826414,0.125618639793563,
-0.0252519969878931));
#38916=CARTESIAN_POINT('Ctrl Pts',(-0.0668985217678414,0.109179796342103,
-0.0228946166849909));
#38917=CARTESIAN_POINT('Ctrl Pts',(-0.0926952692470915,0.078847151123733,
-0.0205372363820887));
#38918=CARTESIAN_POINT('Ctrl Pts',(-0.111108539616056,0.0571962357181767,
-0.0188545792597238));
#38919=CARTESIAN_POINT('Ctrl Pts',(-0.121203912684722,0.0284666277043547,
-0.0171719221373589));
#38920=CARTESIAN_POINT('Ctrl Pts',(-0.121436917850398,-0.000108937277296349,
-0.015489265014994));
#38921=CARTESIAN_POINT('Origin',(0.,0.,-0.466687266823562));
#38922=CARTESIAN_POINT('',(-0.0957194724394942,6.07309540377199E-5,-0.0391872668235621));
#38923=CARTESIAN_POINT('',(-0.095775248172958,-8.59169925714678E-5,-0.0303127331764374));
#38924=CARTESIAN_POINT('',(-0.095825,-3.71055914695333E-15,-0.466687266823562));
#38925=CARTESIAN_POINT('',(-0.0660853196898438,0.0695807828091147,-2.60208521396521E-17));
#38926=CARTESIAN_POINT('Ctrl Pts',(-0.0957194724394942,6.07309540377222E-5,
-0.0391872668235621));
#38927=CARTESIAN_POINT('Ctrl Pts',(-0.0955990282640391,-0.0200853268797188,
-0.037685350615542));
#38928=CARTESIAN_POINT('Ctrl Pts',(-0.079599763565718,-0.072026908170814,
-0.0338260541046197));
#38929=CARTESIAN_POINT('Ctrl Pts',(0.00516325821538433,-0.112752444638587,
-0.0276093772907953));
#38930=CARTESIAN_POINT('Ctrl Pts',(0.0969610666293677,-0.0578066470336301,
-0.0205372363820888));
#38931=CARTESIAN_POINT('Ctrl Pts',(0.101634180818392,0.0491055451050618,
-0.0134650954733823));
#38932=CARTESIAN_POINT('Ctrl Pts',(0.0178076722256624,0.109828753243069,
-0.00661935001268602));
#38933=CARTESIAN_POINT('Ctrl Pts',(-0.0453521829837652,0.0890152473756348,
-0.00213098485489195));
#38934=CARTESIAN_POINT('Ctrl Pts',(-0.0660853196898438,0.0695807828091147,
-3.4477629085039E-17));
#38935=CARTESIAN_POINT('',(0.0442442935173268,0.0849992536211503,0.));
#38936=CARTESIAN_POINT('Origin',(0.,0.,0.));
#38937=CARTESIAN_POINT('Ctrl Pts',(-0.095775248172958,-8.59169925714618E-5,
-0.0303127331764374));
#38938=CARTESIAN_POINT('Ctrl Pts',(-0.0958489363990951,-0.00912298142099969,
-0.0296380099959002));
#38939=CARTESIAN_POINT('Ctrl Pts',(-0.0905597458604163,-0.0496463906961603,
-0.0266059065124609));
#38940=CARTESIAN_POINT('Ctrl Pts',(-0.0334457163768884,-0.107772616556743,
-0.0212164227261194));
#38941=CARTESIAN_POINT('Ctrl Pts',(0.0715887019827832,-0.0873619805387618,
-0.014144281817413));
#38942=CARTESIAN_POINT('Ctrl Pts',(0.112228173818235,0.0118018015396153,
-0.00707214090870642));
#38943=CARTESIAN_POINT('Ctrl Pts',(0.0722220004899157,0.0704361389289412,
-0.00235738030290216));
#38944=CARTESIAN_POINT('Ctrl Pts',(0.0442442935173268,0.0849992536211503,
0.));
#38945=CARTESIAN_POINT('Origin',(0.,0.,-0.466687266823562));
#38946=CARTESIAN_POINT('',(-0.0959751130414699,-5.26327519415071E-8,-0.0841872668235621));
#38947=CARTESIAN_POINT('',(-0.0957274320715207,6.49164786371351E-5,-0.0753127331764374));
#38948=CARTESIAN_POINT('',(-0.095825,-3.71055914695333E-15,-0.466687266823562));
#38949=CARTESIAN_POINT('Ctrl Pts',(-0.09597511304147,-5.26327519511634E-8,
-0.0841872668235621));
#38950=CARTESIAN_POINT('Ctrl Pts',(-0.0959751130735191,-3.43738508333871E-6,
-0.0841870127358571));
#38951=CARTESIAN_POINT('Ctrl Pts',(-0.0959735887129596,-0.0314099491378808,
-0.08182937834525));
#38952=CARTESIAN_POINT('Ctrl Pts',(-0.0621635455577987,-0.0942160343945172,
-0.0771143636517407));
#38953=CARTESIAN_POINT('Ctrl Pts',(0.0443946751765518,-0.103778829919784,
-0.0700422227430341));
#38954=CARTESIAN_POINT('Ctrl Pts',(0.111070156606965,-0.0201100099317029,
-0.0629700818343277));
#38955=CARTESIAN_POINT('Ctrl Pts',(0.077962939724412,0.0816258135429839,
-0.0558979409256211));
#38956=CARTESIAN_POINT('Ctrl Pts',(-0.0251832945736545,0.110029895006483,
-0.0488258000169148));
#38957=CARTESIAN_POINT('Ctrl Pts',(-0.0886060442232168,0.0545484618118582,
-0.0432555753162283));
#38958=CARTESIAN_POINT('Ctrl Pts',(-0.0957880752463548,0.0115355582700803,
-0.0400427309184441));
#38959=CARTESIAN_POINT('Ctrl Pts',(-0.0957194724394942,6.07309540377222E-5,
-0.0391872668235621));
#38960=CARTESIAN_POINT('Ctrl Pts',(-0.0957274320715207,6.49164786371299E-5,
-0.0753127331764374));
#38961=CARTESIAN_POINT('Ctrl Pts',(-0.0955962157823984,-0.0204591451340034,
-0.0737822918133132));
#38962=CARTESIAN_POINT('Ctrl Pts',(-0.0791254621839689,-0.07278913840738,
-0.0698944701472868));
#38963=CARTESIAN_POINT('Ctrl Pts',(0.00651252049231818,-0.112687006408486,
-0.0636492681783584));
#38964=CARTESIAN_POINT('Ctrl Pts',(0.0976402116650261,-0.0566358069940454,
-0.0565771272696518));
#38965=CARTESIAN_POINT('Ctrl Pts',(0.101048976780522,0.0503008121113309,
-0.0495049863609453));
#38966=CARTESIAN_POINT('Ctrl Pts',(0.0136813721824698,0.112038340180693,
-0.0424328454522389));
#38967=CARTESIAN_POINT('Ctrl Pts',(-0.0764747035464821,0.076854043937596,
-0.0360354277240695));
#38968=CARTESIAN_POINT('Ctrl Pts',(-0.0955914809301527,0.0224511489692956,
-0.0319953902988024));
#38969=CARTESIAN_POINT('Ctrl Pts',(-0.095775248172958,-8.59169925714618E-5,
-0.0303127331764374));
#38970=CARTESIAN_POINT('Origin',(0.,0.,-0.466687266823562));
#38971=CARTESIAN_POINT('',(-0.0957194655585664,-6.0908243783317E-5,-0.129187266823562));
#38972=CARTESIAN_POINT('',(-0.0959744524639226,-6.84934123261483E-6,-0.120312733176437));
#38973=CARTESIAN_POINT('',(-0.095825,-3.71055914695333E-15,-0.466687266823562));
#38974=CARTESIAN_POINT('Ctrl Pts',(-0.0957194655585664,-6.09082437833235E-5,
-0.129187266823562));
#38975=CARTESIAN_POINT('Ctrl Pts',(-0.0957878927736574,-0.0115423430508919,
-0.12833129455327));
#38976=CARTESIAN_POINT('Ctrl Pts',(-0.0885997276627033,-0.0545612978206964,
-0.125117941980076));
#38977=CARTESIAN_POINT('Ctrl Pts',(-0.0251602537774947,-0.11003600414835,
-0.11954720910398));
#38978=CARTESIAN_POINT('Ctrl Pts',(0.0779805128909062,-0.081608819302419,
-0.112475068195273));
#38979=CARTESIAN_POINT('Ctrl Pts',(0.111065769910699,0.0201334402733364,
-0.105402927286567));
#38980=CARTESIAN_POINT('Ctrl Pts',(0.0443726347616168,0.10378839523891,
-0.0983307863778601));
#38981=CARTESIAN_POINT('Ctrl Pts',(-0.0621797921696317,0.0942030708531262,
-0.0912588995568586));
#38982=CARTESIAN_POINT('Ctrl Pts',(-0.0959748157271878,0.0313996896429778,
-0.0865443930387592));
#38983=CARTESIAN_POINT('Ctrl Pts',(-0.09597511304147,-5.26327519511634E-8,
-0.0841872668235621));
#38984=CARTESIAN_POINT('Ctrl Pts',(-0.0959744524639226,-6.84934123261998E-6,
-0.120312733176437));
#38985=CARTESIAN_POINT('Ctrl Pts',(-0.0959748548604342,-0.00039023024799691,
-0.120283953933628));
#38986=CARTESIAN_POINT('Ctrl Pts',(-0.0958005075262998,-0.0321769314557355,
-0.117897794387917));
#38987=CARTESIAN_POINT('Ctrl Pts',(-0.0610334100648855,-0.094952004625933,
-0.113154254539304));
#38988=CARTESIAN_POINT('Ctrl Pts',(0.0456315363448654,-0.103241066588768,
-0.106082113630597));
#38989=CARTESIAN_POINT('Ctrl Pts',(0.111302404448902,-0.0187812994845884,
-0.0990099727218907));
#38990=CARTESIAN_POINT('Ctrl Pts',(0.0769822665584455,0.082551176948899,
-0.0919378318131844));
#38991=CARTESIAN_POINT('Ctrl Pts',(-0.0264965203447265,0.109721764831659,
-0.0848656909044777));
#38992=CARTESIAN_POINT('Ctrl Pts',(-0.0889296549406001,0.053773055187859,
-0.0793239913588955));
#38993=CARTESIAN_POINT('Ctrl Pts',(-0.0957983317881795,0.0111546231206798,
-0.0761396721162153));
#38994=CARTESIAN_POINT('Ctrl Pts',(-0.0957274320715207,6.49164786371299E-5,
-0.0753127331764374));
#38995=CARTESIAN_POINT('Origin',(0.,0.,-0.466687266823562));
#38996=CARTESIAN_POINT('',(-0.0957878027106809,8.13637278885715E-5,-0.174187266823562));
#38997=CARTESIAN_POINT('',(-0.0957121716339357,-5.66137451362067E-5,-0.165312733176438));
#38998=CARTESIAN_POINT('',(-0.095825,-3.71055914695333E-15,-0.466687266823562));
#38999=CARTESIAN_POINT('Ctrl Pts',(-0.0957878027106809,8.13637278885707E-5,
-0.174187266823562));
#39000=CARTESIAN_POINT('Ctrl Pts',(-0.0955951522778602,-0.0228366251828878,
-0.172475576370683));
#39001=CARTESIAN_POINT('Ctrl Pts',(-0.0759427696888102,-0.077614637258398,
-0.168406505614902));
#39002=CARTESIAN_POINT('Ctrl Pts',(0.0150412165657262,-0.111869218970413,
-0.161980054556218));
#39003=CARTESIAN_POINT('Ctrl Pts',(0.101654099403055,-0.0490653075613788,
-0.154907913647512));
#39004=CARTESIAN_POINT('Ctrl Pts',(0.09694377988408,0.0578175049768839,
-0.147835772738805));
#39005=CARTESIAN_POINT('Ctrl Pts',(0.00514187719049035,0.112758686937953,
-0.140763631830099));
#39006=CARTESIAN_POINT('Ctrl Pts',(-0.0796090601597848,0.0720115357319004,
-0.134547463191685));
#39007=CARTESIAN_POINT('Ctrl Pts',(-0.0955994416115853,0.0200779666281811,
-0.130688674856172));
#39008=CARTESIAN_POINT('Ctrl Pts',(-0.0957194655585664,-6.09082437833235E-5,
-0.129187266823562));
#39009=CARTESIAN_POINT('Ctrl Pts',(-0.0957121716339357,-5.66137451362076E-5,
-0.165312733176438));
#39010=CARTESIAN_POINT('Ctrl Pts',(-0.0957775679602116,-0.0119229404138125,
-0.164428235751041));
#39011=CARTESIAN_POINT('Ctrl Pts',(-0.0882696983379308,-0.0553358580165303,
-0.161186358022743));
#39012=CARTESIAN_POINT('Ctrl Pts',(-0.0238437133266645,-0.110328764767113,
-0.155587099991542));
#39013=CARTESIAN_POINT('Ctrl Pts',(0.0789500302236065,-0.0806712564157815,
-0.148514959082836));
#39014=CARTESIAN_POINT('Ctrl Pts',(0.110817273075402,0.0214590532670084,
-0.14144281817413));
#39015=CARTESIAN_POINT('Ctrl Pts',(0.0431293735332865,0.104311151550646,
-0.134370677265423));
#39016=CARTESIAN_POINT('Ctrl Pts',(-0.0628716275040662,0.0934972072317672,
-0.127327315599526));
#39017=CARTESIAN_POINT('Ctrl Pts',(-0.0959418935481174,0.0310134659545147,
-0.122641334236531));
#39018=CARTESIAN_POINT('Ctrl Pts',(-0.0959744524639226,-6.84934123261998E-6,
-0.120312733176437));
#39019=CARTESIAN_POINT('Origin',(0.,0.,-0.466687266823562));
#39020=CARTESIAN_POINT('',(-0.095944975615187,-4.66871613868081E-5,-0.219187266823562));
#39021=CARTESIAN_POINT('',(-0.0957985183985989,8.23860933714532E-5,-0.210312733176438));
#39022=CARTESIAN_POINT('',(-0.095825,-3.71055914695333E-15,-0.466687266823562));
#39023=CARTESIAN_POINT('Ctrl Pts',(-0.095944975615187,-4.66871613868159E-5,
-0.219187266823562));
#39024=CARTESIAN_POINT('Ctrl Pts',(-0.0959619481171234,-0.00284686035185996,
-0.218977238490998));
#39025=CARTESIAN_POINT('Ctrl Pts',(-0.0945905159566559,-0.037059626206742,
-0.216409829855532));
#39026=CARTESIAN_POINT('Ctrl Pts',(-0.0536556310458891,-0.0993077717118213,
-0.211485040917164));
#39027=CARTESIAN_POINT('Ctrl Pts',(0.0533307801909408,-0.0994826028270216,
-0.204412900008458));
#39028=CARTESIAN_POINT('Ctrl Pts',(0.112406308710366,-0.0102850426384537,
-0.197340759099751));
#39029=CARTESIAN_POINT('Ctrl Pts',(0.0704991503786541,0.0881523120934825,
-0.190268618191045));
#39030=CARTESIAN_POINT('Ctrl Pts',(-0.0347424747368677,0.107396093029428,
-0.183196477282338));
#39031=CARTESIAN_POINT('Ctrl Pts',(-0.0908547496053409,0.0488523265191771,
-0.177836026826511));
#39032=CARTESIAN_POINT('Ctrl Pts',(-0.0958604749797034,0.00872656753663759,
-0.174832956673585));
#39033=CARTESIAN_POINT('Ctrl Pts',(-0.0957878027106809,8.13637278885707E-5,
-0.174187266823562));
#39034=CARTESIAN_POINT('Ctrl Pts',(-0.0957985183985989,8.23860933714523E-5,
-0.210312733176438));
#39035=CARTESIAN_POINT('Ctrl Pts',(-0.0955983110355252,-0.0232108787151331,
-0.208572517568454));
#39036=CARTESIAN_POINT('Ctrl Pts',(-0.0754156206185855,-0.078369269952436,
-0.204474921657569));
#39037=CARTESIAN_POINT('Ctrl Pts',(0.0163767894818392,-0.111681510260943,
-0.198019945443782));
#39038=CARTESIAN_POINT('Ctrl Pts',(0.102233084705024,-0.0478472083859376,
-0.190947804535075));
#39039=CARTESIAN_POINT('Ctrl Pts',(0.0962460332646973,0.058971688456773,
-0.183875663626369));
#39040=CARTESIAN_POINT('Ctrl Pts',(0.0037942348732942,0.112812068280055,
-0.176803522717662));
#39041=CARTESIAN_POINT('Ctrl Pts',(-0.0800771402773893,0.0712468149779357,
-0.170615879234352));
#39042=CARTESIAN_POINT('Ctrl Pts',(-0.0956032723579649,0.0197034317534234,
-0.166785616053944));
#39043=CARTESIAN_POINT('Ctrl Pts',(-0.0957121716339357,-5.66137451362076E-5,
-0.165312733176438));
#39044=CARTESIAN_POINT('Origin',(0.,0.,-0.466687266823562));
#39045=CARTESIAN_POINT('',(-0.0956804223565074,-2.35157469208761E-5,-0.264187266823562));
#39046=CARTESIAN_POINT('',(-0.0959371457461587,-5.20048528196981E-5,-0.255312733176438));
#39047=CARTESIAN_POINT('',(-0.095825,-3.71055914695333E-15,-0.466687266823562));
#39048=CARTESIAN_POINT('Ctrl Pts',(-0.0956804223565074,-2.35157469208793E-5,
-0.264187266823562));
#39049=CARTESIAN_POINT('Ctrl Pts',(-0.0957125021369695,-0.0143333873827806,
-0.263121520308411));
#39050=CARTESIAN_POINT('Ctrl Pts',(-0.0860327810025941,-0.0602547865702146,
-0.259698393490358));
#39051=CARTESIAN_POINT('Ctrl Pts',(-0.0154067542351519,-0.111819444898135,
-0.253917886369403));
#39052=CARTESIAN_POINT('Ctrl Pts',(0.0848414033458655,-0.0744506412347145,
-0.246845745460696));
#39053=CARTESIAN_POINT('Ctrl Pts',(0.108870415651418,0.0298025713485215,
-0.23977360455199));
#39054=CARTESIAN_POINT('Ctrl Pts',(0.0350932882052845,0.107281969135566,
-0.232701463643283));
#39055=CARTESIAN_POINT('Ctrl Pts',(-0.0670833532499771,0.0889435362384874,
-0.225839351067141));
#39056=CARTESIAN_POINT('Ctrl Pts',(-0.0957714469534591,0.0285825808256805,
-0.221334618793901));
#39057=CARTESIAN_POINT('Ctrl Pts',(-0.095944975615187,-4.66871613868159E-5,
-0.219187266823562));
#39058=CARTESIAN_POINT('Ctrl Pts',(-0.0959371457461587,-5.20048528197068E-5,
-0.255312733176438));
#39059=CARTESIAN_POINT('Ctrl Pts',(-0.0959581715766043,-0.00323317110377817,
-0.25507417968877));
#39060=CARTESIAN_POINT('Ctrl Pts',(-0.0943823518025523,-0.0378294848809537,
-0.2524782458982));
#39061=CARTESIAN_POINT('Ctrl Pts',(-0.0524652380640034,-0.0999417689982206,
-0.247524931804727));
#39062=CARTESIAN_POINT('Ctrl Pts',(0.0545156184897837,-0.0988382847881933,
-0.240452790896021));
#39063=CARTESIAN_POINT('Ctrl Pts',(0.112521167612446,-0.00894124253760813,
-0.233380649987314));
#39064=CARTESIAN_POINT('Ctrl Pts',(0.0694408433772929,0.0889883596604602,
-0.226308509078608));
#39065=CARTESIAN_POINT('Ctrl Pts',(-0.0360231939491006,0.106973307408655,
-0.219236368169901));
#39066=CARTESIAN_POINT('Ctrl Pts',(-0.091137108833105,0.0480783572787451,
-0.213904442869178));
#39067=CARTESIAN_POINT('Ctrl Pts',(-0.0958695216211795,0.00834330537444174,
-0.210929897871357));
#39068=CARTESIAN_POINT('Ctrl Pts',(-0.0957985183985989,8.23860933714523E-5,
-0.210312733176438));
#39069=CARTESIAN_POINT('Origin',(0.,0.,-0.466687266823562));
#39070=CARTESIAN_POINT('',(-0.0958690039724624,7.88897705069557E-5,-0.309187266823562));
#39071=CARTESIAN_POINT('',(-0.0956779014015301,-1.7615076390011E-5,-0.300312733176438));
#39072=CARTESIAN_POINT('',(-0.095825,-3.71055914695333E-15,-0.466687266823562));
#39073=CARTESIAN_POINT('Ctrl Pts',(-0.0958690039724624,7.88897705069598E-5,
-0.309187266823562));
#39074=CARTESIAN_POINT('Ctrl Pts',(-0.0956435931287137,-0.0255918778922679,
-0.307265802125824));
#39075=CARTESIAN_POINT('Ctrl Pts',(-0.0718951791629235,-0.0831279477414135,
-0.302986957125184));
#39076=CARTESIAN_POINT('Ctrl Pts',(0.0248005137658673,-0.110116804519884,
-0.296350731821642));
#39077=CARTESIAN_POINT('Ctrl Pts',(0.105567722156006,-0.0399555934234326,
-0.289278590912935));
#39078=CARTESIAN_POINT('Ctrl Pts',(0.0914958773173812,0.0661021680587838,
-0.282206450004229));
#39079=CARTESIAN_POINT('Ctrl Pts',(-0.00477332737082577,0.112774766988728,
-0.275134309095522));
#39080=CARTESIAN_POINT('Ctrl Pts',(-0.0828930919733463,0.0663682535192907,
-0.269127914701967));
#39081=CARTESIAN_POINT('Ctrl Pts',(-0.0956415431973834,0.0173193640471915,
-0.265478900611313));
#39082=CARTESIAN_POINT('Ctrl Pts',(-0.0956804223565074,-2.35157469208793E-5,
-0.264187266823562));
#39083=CARTESIAN_POINT('Ctrl Pts',(-0.09567790140153,-1.76150763900179E-5,
-0.300312733176438));
#39084=CARTESIAN_POINT('Ctrl Pts',(-0.0957026375134359,-0.0147114989746946,
-0.299218461506183));
#39085=CARTESIAN_POINT('Ctrl Pts',(-0.0856582592510746,-0.0610282955341015,
-0.295766809533026));
#39086=CARTESIAN_POINT('Ctrl Pts',(-0.0140695777255182,-0.111995438526656,
-0.289957777256965));
#39087=CARTESIAN_POINT('Ctrl Pts',(0.0857248891793926,-0.0734316658894842,
-0.28288563634826));
#39088=CARTESIAN_POINT('Ctrl Pts',(0.108506554426889,0.0311012876396027,
-0.275813495439553));
#39089=CARTESIAN_POINT('Ctrl Pts',(0.0338089402553138,0.107693595438131,
-0.268741354530847));
#39090=CARTESIAN_POINT('Ctrl Pts',(-0.0677174862885282,0.0882169577300349,
-0.261907767109808));
#39091=CARTESIAN_POINT('Ctrl Pts',(-0.0957503947839486,0.0282030436150841,
-0.257431559991672));
#39092=CARTESIAN_POINT('Ctrl Pts',(-0.0959371457461587,-5.20048528197068E-5,
-0.255312733176438));
#39093=CARTESIAN_POINT('Origin',(0.,0.,-0.466687266823562));
#39094=CARTESIAN_POINT('',(-0.0958726565381089,-8.61752489211661E-5,-0.354187266823562));
#39095=CARTESIAN_POINT('',(-0.0958786240325138,8.20367901696907E-5,-0.345312733176438));
#39096=CARTESIAN_POINT('',(-0.095825,-3.71055914695333E-15,-0.466687266823562));
#39097=CARTESIAN_POINT('Ctrl Pts',(-0.095872656538109,-8.6175248921171E-5,
-0.354187266823562));
#39098=CARTESIAN_POINT('Ctrl Pts',(-0.0959221857987575,-0.00567877154923316,
-0.353767464246139));
#39099=CARTESIAN_POINT('Ctrl Pts',(-0.0929422356532186,-0.0426364993896563,
-0.350990281365814));
#39100=CARTESIAN_POINT('Ctrl Pts',(-0.0447352950033125,-0.103710198939767,
-0.345855718182587));
#39101=CARTESIAN_POINT('Ctrl Pts',(0.0618562700166257,-0.0943788386242131,
-0.338783577273881));
#39102=CARTESIAN_POINT('Ctrl Pts',(0.112874708577635,-0.000401788756397879,
-0.331711436365174));
#39103=CARTESIAN_POINT('Ctrl Pts',(0.06249144654252,0.0940099781523149,
-0.324639295456468));
#39104=CARTESIAN_POINT('Ctrl Pts',(-0.0440333363121848,0.103927081651485,
-0.317567154547761));
#39105=CARTESIAN_POINT('Ctrl Pts',(-0.0928049870134241,0.0431662527422258,
-0.312416478336793));
#39106=CARTESIAN_POINT('Ctrl Pts',(-0.0959201420987464,0.00590272209691865,
-0.309623182428726));
#39107=CARTESIAN_POINT('Ctrl Pts',(-0.0958690039724624,7.88897705069598E-5,
-0.309187266823562));
#39108=CARTESIAN_POINT('Ctrl Pts',(-0.0958786240325138,8.20367901696933E-5,
-0.345312733176438));
#39109=CARTESIAN_POINT('Ctrl Pts',(-0.0956537848124931,-0.0259620098340212,
-0.343362743323596));
#39110=CARTESIAN_POINT('Ctrl Pts',(-0.07131568583194,-0.0838783814842911,
-0.339055373167851));
#39111=CARTESIAN_POINT('Ctrl Pts',(0.0261155403145056,-0.109807778273315,
-0.332390622709205));
#39112=CARTESIAN_POINT('Ctrl Pts',(0.106037008942776,-0.0386939290059783,
-0.325318481800498));
#39113=CARTESIAN_POINT('Ctrl Pts',(0.0906998339925985,0.0671920060838559,
-0.318246340891792));
#39114=CARTESIAN_POINT('Ctrl Pts',(-0.00612061239846709,0.112708972315148,
-0.311174199983085));
#39115=CARTESIAN_POINT('Ctrl Pts',(-0.0833117710540488,0.0655980927825272,
-0.305196330744634));
#39116=CARTESIAN_POINT('Ctrl Pts',(-0.0956493487145368,0.0169434121562133,
-0.301575841809085));
#39117=CARTESIAN_POINT('Ctrl Pts',(-0.09567790140153,-1.76150763900179E-5,
-0.300312733176438));
#39118=CARTESIAN_POINT('Ctrl Pts',(0.0534655244842089,-0.079522753452257,
-0.374823468161444));
#39119=CARTESIAN_POINT('Ctrl Pts',(0.0796406283699102,-0.0619244486033452,
-0.372466087858542));
#39120=CARTESIAN_POINT('Ctrl Pts',(0.112844070495072,0.00081318648518734,
-0.367751327252737));
#39121=CARTESIAN_POINT('Ctrl Pts',(0.0613779578258757,0.0948145779316648,
-0.360679186344031));
#39122=CARTESIAN_POINT('Ctrl Pts',(-0.0452794177261462,0.103360181665046,
-0.353607045435324));
#39123=CARTESIAN_POINT('Ctrl Pts',(-0.111232369054601,0.0191891251444319,
-0.346534904526618));
#39124=CARTESIAN_POINT('Ctrl Pts',(-0.0772712803160827,-0.0822934176220715,
-0.339462763617911));
#39125=CARTESIAN_POINT('Ctrl Pts',(0.0261155403145056,-0.109807778273315,
-0.332390622709205));
#39126=CARTESIAN_POINT('Ctrl Pts',(0.106037008942776,-0.0386939290059783,
-0.325318481800498));
#39127=CARTESIAN_POINT('Ctrl Pts',(0.0906998339925985,0.0671920060838559,
-0.318246340891792));
#39128=CARTESIAN_POINT('Ctrl Pts',(-0.00612061239846709,0.112708972315148,
-0.311174199983085));
#39129=CARTESIAN_POINT('Ctrl Pts',(-0.0974419058465003,0.0569742673395502,
-0.304102059074378));
#39130=CARTESIAN_POINT('Ctrl Pts',(-0.101224411638868,-0.0499460644092083,
-0.297029918165673));
#39131=CARTESIAN_POINT('Ctrl Pts',(-0.0140695777255182,-0.111995438526656,
-0.289957777256965));
#39132=CARTESIAN_POINT('Ctrl Pts',(0.0857248891793926,-0.0734316658894842,
-0.28288563634826));
#39133=CARTESIAN_POINT('Ctrl Pts',(0.108506554426889,0.0311012876396027,
-0.275813495439553));
#39134=CARTESIAN_POINT('Ctrl Pts',(0.0338089402553138,0.107693595438131,
-0.268741354530847));
#39135=CARTESIAN_POINT('Ctrl Pts',(-0.0712616691093911,0.0875370483988087,
-0.261669213622139));
#39136=CARTESIAN_POINT('Ctrl Pts',(-0.112312792499519,-0.0112603696058821,
-0.254597072713434));
#39137=CARTESIAN_POINT('Ctrl Pts',(-0.0524652380640034,-0.0999417689982206,
-0.247524931804727));
#39138=CARTESIAN_POINT('Ctrl Pts',(0.0545156184897837,-0.0988382847881933,
-0.240452790896021));
#39139=CARTESIAN_POINT('Ctrl Pts',(0.112521167612446,-0.00894124253760813,
-0.233380649987314));
#39140=CARTESIAN_POINT('Ctrl Pts',(0.0694408433772929,0.0889883596604602,
-0.226308509078608));
#39141=CARTESIAN_POINT('Ctrl Pts',(-0.0360231939491006,0.106973307408655,
-0.219236368169901));
#39142=CARTESIAN_POINT('Ctrl Pts',(-0.109125000539913,0.0288564241744764,
-0.212164227261195));
#39143=CARTESIAN_POINT('Ctrl Pts',(-0.0841919557899689,-0.0751842638507629,
-0.205092086352488));
#39144=CARTESIAN_POINT('Ctrl Pts',(0.0163767894818392,-0.111681510260943,
-0.198019945443782));
#39145=CARTESIAN_POINT('Ctrl Pts',(0.102233084705024,-0.0478472083859376,
-0.190947804535075));
#39146=CARTESIAN_POINT('Ctrl Pts',(0.0962460332646973,0.058971688456773,
-0.183875663626369));
#39147=CARTESIAN_POINT('Ctrl Pts',(0.0037942348732942,0.112812068280055,
-0.176803522717662));
#39148=CARTESIAN_POINT('Ctrl Pts',(-0.0920661980803001,0.0653052380866966,
-0.169731381808956));
#39149=CARTESIAN_POINT('Ctrl Pts',(-0.105216931285724,-0.0408699930240835,
-0.162659240900249));
#39150=CARTESIAN_POINT('Ctrl Pts',(-0.0238437133266645,-0.110328764767113,
-0.155587099991542));
#39151=CARTESIAN_POINT('Ctrl Pts',(0.0789500302236065,-0.0806712564157815,
-0.148514959082836));
#39152=CARTESIAN_POINT('Ctrl Pts',(0.110817273075402,0.0214590532670084,
-0.14144281817413));
#39153=CARTESIAN_POINT('Ctrl Pts',(0.0431293735332865,0.104311151550646,
-0.134370677265423));
#39154=CARTESIAN_POINT('Ctrl Pts',(-0.0633047486032753,0.0934530213523478,
-0.127298536356717));
#39155=CARTESIAN_POINT('Ctrl Pts',(-0.112867656235649,-0.00136068312712246,
-0.12022639544801));
#39156=CARTESIAN_POINT('Ctrl Pts',(-0.0610334100648855,-0.094952004625933,
-0.113154254539304));
#39157=CARTESIAN_POINT('Ctrl Pts',(0.0456315363448654,-0.103241066588768,
-0.106082113630597));
#39158=CARTESIAN_POINT('Ctrl Pts',(0.111302404448902,-0.0187812994845884,
-0.0990099727218907));
#39159=CARTESIAN_POINT('Ctrl Pts',(0.0769822665584455,0.082551176948899,
-0.0919378318131844));
#39160=CARTESIAN_POINT('Ctrl Pts',(-0.0264965203447265,0.109721764831659,
-0.0848656909044777));
#39161=CARTESIAN_POINT('Ctrl Pts',(-0.106171703310255,0.038321798989649,
-0.0777935499957714));
#39162=CARTESIAN_POINT('Ctrl Pts',(-0.090464948553087,-0.0675061866584397,
-0.0707214090870648));
#39163=CARTESIAN_POINT('Ctrl Pts',(0.00651252049231818,-0.112687006408486,
-0.0636492681783584));
#39164=CARTESIAN_POINT('Ctrl Pts',(0.0976402116650261,-0.0566358069940454,
-0.0565771272696518));
#39165=CARTESIAN_POINT('Ctrl Pts',(0.101048976780522,0.0503008121113309,
-0.0495049863609453));
#39166=CARTESIAN_POINT('Ctrl Pts',(0.0136813721824698,0.112038340180693,
-0.0424328454522389));
#39167=CARTESIAN_POINT('Ctrl Pts',(-0.0859832891579445,0.0731432247798018,
-0.0353607045435324));
#39168=CARTESIAN_POINT('Ctrl Pts',(-0.108391384716252,-0.0314987328094481,
-0.0282885636348259));
#39169=CARTESIAN_POINT('Ctrl Pts',(-0.0334457163768884,-0.107772616556743,
-0.0212164227261194));
#39170=CARTESIAN_POINT('Ctrl Pts',(0.0715887019827832,-0.0873619805387618,
-0.014144281817413));
#39171=CARTESIAN_POINT('Ctrl Pts',(0.112228173818235,0.0118018015396153,
-0.00707214090870642));
#39172=CARTESIAN_POINT('Ctrl Pts',(0.0722220004899157,0.0704361389289412,
-0.00235738030290216));
#39173=CARTESIAN_POINT('Ctrl Pts',(0.0442442935173268,0.0849992536211503,
0.));
#39174=CARTESIAN_POINT('Ctrl Pts',(0.0582406435071917,-0.0866250986818831,
-0.369882312107629));
#39175=CARTESIAN_POINT('Ctrl Pts',(0.0867535012576304,-0.0674550520223937,
-0.367524931804727));
#39176=CARTESIAN_POINT('Ctrl Pts',(0.122922412994284,0.000885813889333945,
-0.362810171198922));
#39177=CARTESIAN_POINT('Ctrl Pts',(0.0668597529982539,0.103282668333945,
-0.355738030290216));
#39178=CARTESIAN_POINT('Ctrl Pts',(-0.0493234182483436,0.112591498002988,
-0.34866588938151));
#39179=CARTESIAN_POINT('Ctrl Pts',(-0.121166767090871,0.0209029464787511,
-0.341593748472803));
#39180=CARTESIAN_POINT('Ctrl Pts',(-0.0841725417200849,-0.0896432167261558,
-0.334521607564097));
#39181=CARTESIAN_POINT('Ctrl Pts',(0.0284479744307761,-0.119614943095186,
-0.32744946665539));
#39182=CARTESIAN_POINT('Ctrl Pts',(0.115507398383964,-0.0421497656082171,
-0.320377325746683));
#39183=CARTESIAN_POINT('Ctrl Pts',(0.0988004279147136,0.0731930661976151,
-0.313305184837978));
#39184=CARTESIAN_POINT('Ctrl Pts',(-0.00666725723134143,0.1227752489103,
-0.30623304392927));
#39185=CARTESIAN_POINT('Ctrl Pts',(-0.10614464845928,0.0620627596047666,
-0.299160903020565));
#39186=CARTESIAN_POINT('Ctrl Pts',(-0.110264977840549,-0.0544068530124132,
-0.292088762111858));
#39187=CARTESIAN_POINT('Ctrl Pts',(-0.0153261614566349,-0.121997987910679,
-0.285016621203151));
#39188=CARTESIAN_POINT('Ctrl Pts',(0.0933811602627245,-0.07999000321173,
-0.277944480294445));
#39189=CARTESIAN_POINT('Ctrl Pts',(0.118197504196123,0.0338790093898305,
-0.270872339385739));
#39190=CARTESIAN_POINT('Ctrl Pts',(0.0368284881848912,0.117311938121404,
-0.263800198477032));
#39191=CARTESIAN_POINT('Ctrl Pts',(-0.0776261994316225,0.0953551672531074,
-0.256728057568326));
#39192=CARTESIAN_POINT('Ctrl Pts',(-0.122343685437775,-0.0122660570208953,
-0.249655916659619));
#39193=CARTESIAN_POINT('Ctrl Pts',(-0.0571510193920957,-0.108867779674033,
-0.242583775750913));
#39194=CARTESIAN_POINT('Ctrl Pts',(0.0593845236284047,-0.107665740956336,
-0.235511634842206));
#39195=CARTESIAN_POINT('Ctrl Pts',(0.122570670972563,-0.00973980381129516,
-0.2284394939335));
#39196=CARTESIAN_POINT('Ctrl Pts',(0.0756427519039894,0.0969360981917489,
-0.221367353024793));
#39197=CARTESIAN_POINT('Ctrl Pts',(-0.0392405015572163,0.116527319645258,
-0.214295212116087));
#39198=CARTESIAN_POINT('Ctrl Pts',(-0.118871185038956,0.0314336524227755,
-0.20722307120738));
#39199=CARTESIAN_POINT('Ctrl Pts',(-0.0917113173515221,-0.0818991294020917,
-0.200150930298673));
#39200=CARTESIAN_POINT('Ctrl Pts',(0.0178394351725813,-0.12165602204788,
-0.193078789389967));
#39201=CARTESIAN_POINT('Ctrl Pts',(0.111363737630675,-0.05212054372052,
-0.186006648481261));
#39202=CARTESIAN_POINT('Ctrl Pts',(0.104841969969006,0.0642385746247095,
-0.178934507572554));
#39203=CARTESIAN_POINT('Ctrl Pts',(0.00413310601120864,0.122887552593788,
-0.171862366663848));
#39204=CARTESIAN_POINT('Ctrl Pts',(-0.100288824867713,0.0711377869618198,
-0.164790225755141));
#39205=CARTESIAN_POINT('Ctrl Pts',(-0.114614077857638,-0.0445201785041887,
-0.157718084846435));
#39206=CARTESIAN_POINT('Ctrl Pts',(-0.0259732457717892,-0.120182459994161,
-0.150645943937728));
#39207=CARTESIAN_POINT('Ctrl Pts',(0.0860012243308889,-0.0878761768731265,
-0.143573803029022));
#39208=CARTESIAN_POINT('Ctrl Pts',(0.120714598012218,0.0233756066808019,
-0.136501662120315));
#39209=CARTESIAN_POINT('Ctrl Pts',(0.0469813490632185,0.113627401019514,
-0.129429521211609));
#39210=CARTESIAN_POINT('Ctrl Pts',(-0.0689586295334048,0.101799508258067,
-0.122357380302902));
#39211=CARTESIAN_POINT('Ctrl Pts',(-0.122948105227214,-0.00148220861382132,
-0.115285239394196));
#39212=CARTESIAN_POINT('Ctrl Pts',(-0.0664844329483225,-0.103432368896811,
-0.108213098485489));
#39213=CARTESIAN_POINT('Ctrl Pts',(0.0497069853253135,-0.112461744507428,
-0.101140957576783));
#39214=CARTESIAN_POINT('Ctrl Pts',(0.121243057494299,-0.0204586970470439,
-0.0940688166680762));
#39215=CARTESIAN_POINT('Ctrl Pts',(0.0838577155327499,0.0899239970833903,
-0.0869966757593699));
#39216=CARTESIAN_POINT('Ctrl Pts',(-0.0288629805929245,0.119521247611216,
-0.0799245348506631));
#39217=CARTESIAN_POINT('Ctrl Pts',(-0.11565412259016,0.0417443998734104,
-0.0728523939419568));
#39218=CARTESIAN_POINT('Ctrl Pts',(-0.0985445643600286,-0.0735353069035231,
-0.0657802530332502));
#39219=CARTESIAN_POINT('Ctrl Pts',(0.00709416746558592,-0.122751321182076,
-0.0587081121245439));
#39220=CARTESIAN_POINT('Ctrl Pts',(0.106360665389696,-0.0616940706502668,
-0.0516359712158373));
#39221=CARTESIAN_POINT('Ctrl Pts',(0.110073874524117,0.0547932839817835,
-0.0445638303071308));
#39222=CARTESIAN_POINT('Ctrl Pts',(0.0149032844558327,0.122044721202136,
-0.0374916893984243));
#39223=CARTESIAN_POINT('Ctrl Pts',(-0.0936626384896434,0.0796758008167494,
-0.0304195484897179));
#39224=CARTESIAN_POINT('Ctrl Pts',(-0.118072048435149,-0.0343119512280323,
-0.0233474075810114));
#39225=CARTESIAN_POINT('Ctrl Pts',(-0.0364328240139933,-0.117398016783178,
-0.0162752666723049));
#39226=CARTESIAN_POINT('Ctrl Pts',(0.0779824403023166,-0.0951644637123691,
-0.00920312576359843));
#39227=CARTESIAN_POINT('Ctrl Pts',(0.122251509283174,0.0128558453852698,
-0.00213098485489189));
#39228=CARTESIAN_POINT('Ctrl Pts',(0.0786723000379761,0.0767269394055061,
0.00258377575091239));
#39229=CARTESIAN_POINT('Ctrl Pts',(0.0481958449080824,0.0925907166587118,
0.00494115605381455));
#39230=CARTESIAN_POINT('Ctrl Pts',(0.0630157625301746,-0.0937274439115092,
-0.364941156053815));
#39231=CARTESIAN_POINT('Ctrl Pts',(0.0938663741453508,-0.0729856554414422,
-0.362583775750912));
#39232=CARTESIAN_POINT('Ctrl Pts',(0.133000755493496,0.000958441293480677,
-0.357869015145108));
#39233=CARTESIAN_POINT('Ctrl Pts',(0.0723415481706322,0.111750758736225,
-0.350796874236402));
#39234=CARTESIAN_POINT('Ctrl Pts',(-0.053367418770541,0.121822814340931,
-0.343724733327695));
#39235=CARTESIAN_POINT('Ctrl Pts',(-0.131101165127142,0.0226167678130703,
-0.336652592418989));
#39236=CARTESIAN_POINT('Ctrl Pts',(-0.091073803124087,-0.09699301583024,
-0.329580451510282));
#39237=CARTESIAN_POINT('Ctrl Pts',(0.0307804085470464,-0.129422107917057,
-0.322508310601576));
#39238=CARTESIAN_POINT('Ctrl Pts',(0.124977787825153,-0.0456056022104559,
-0.315436169692869));
#39239=CARTESIAN_POINT('Ctrl Pts',(0.106901021836829,0.0791941263113741,
-0.308364028784163));
#39240=CARTESIAN_POINT('Ctrl Pts',(-0.00721390206421565,0.132841525505452,
-0.301291887875456));
#39241=CARTESIAN_POINT('Ctrl Pts',(-0.11484739107206,0.0671512518699828,
-0.29421974696675));
#39242=CARTESIAN_POINT('Ctrl Pts',(-0.119305544042229,-0.0588676416156181,
-0.287147606058043));
#39243=CARTESIAN_POINT('Ctrl Pts',(-0.0165827451877516,-0.132000537294701,
-0.280075465149337));
#39244=CARTESIAN_POINT('Ctrl Pts',(0.101037431346056,-0.0865483405339757,
-0.27300332424063));
#39245=CARTESIAN_POINT('Ctrl Pts',(0.127888453965356,0.0366567311400581,
-0.265931183331924));
#39246=CARTESIAN_POINT('Ctrl Pts',(0.0398480361144687,0.126930280804678,
-0.258859042423217));
#39247=CARTESIAN_POINT('Ctrl Pts',(-0.0839907297538541,0.103173286107406,
-0.251786901514511));
#39248=CARTESIAN_POINT('Ctrl Pts',(-0.132374578376031,-0.0132717444359084,
-0.244714760605805));
#39249=CARTESIAN_POINT('Ctrl Pts',(-0.0618368007201881,-0.117793790349846,
-0.237642619697098));
#39250=CARTESIAN_POINT('Ctrl Pts',(0.0642534287670256,-0.116493197124479,
-0.230570478788392));
#39251=CARTESIAN_POINT('Ctrl Pts',(0.13262017433268,-0.0105383650849823,
-0.223498337879685));
#39252=CARTESIAN_POINT('Ctrl Pts',(0.0818446604306858,0.104883836723038,
-0.216426196970978));
#39253=CARTESIAN_POINT('Ctrl Pts',(-0.0424578091653319,0.12608133188186,
-0.209354056062272));
#39254=CARTESIAN_POINT('Ctrl Pts',(-0.128617369537998,0.0340108806710746,
-0.202281915153565));
#39255=CARTESIAN_POINT('Ctrl Pts',(-0.0992306789130754,-0.0886139949534205,
-0.195209774244859));
#39256=CARTESIAN_POINT('Ctrl Pts',(0.0193020808633235,-0.131630533834817,
-0.188137633336152));
#39257=CARTESIAN_POINT('Ctrl Pts',(0.120494390556325,-0.0563938790551023,
-0.181065492427446));
#39258=CARTESIAN_POINT('Ctrl Pts',(0.113437906673315,0.0695054607926461,
-0.173993351518739));
#39259=CARTESIAN_POINT('Ctrl Pts',(0.00447197714912307,0.132963036907521,
-0.166921210610033));
#39260=CARTESIAN_POINT('Ctrl Pts',(-0.108511451655127,0.076970335836943,
-0.159849069701326));
#39261=CARTESIAN_POINT('Ctrl Pts',(-0.124011224429552,-0.048170363984294,
-0.15277692879262));
#39262=CARTESIAN_POINT('Ctrl Pts',(-0.0281027782169139,-0.130036155221209,
-0.145704787883913));
#39263=CARTESIAN_POINT('Ctrl Pts',(0.0930524184381714,-0.0950810973304716,
-0.138632646975207));
#39264=CARTESIAN_POINT('Ctrl Pts',(0.130611922949033,0.0252921600945957,
-0.1315605060665));
#39265=CARTESIAN_POINT('Ctrl Pts',(0.0508333245931506,0.122943650488382,
-0.124488365157794));
#39266=CARTESIAN_POINT('Ctrl Pts',(-0.0746125104635343,0.110145995163786,
-0.117416224249088));
#39267=CARTESIAN_POINT('Ctrl Pts',(-0.13302855421878,-0.00160373410052023,
-0.110344083340381));
#39268=CARTESIAN_POINT('Ctrl Pts',(-0.0719354558317593,-0.11191273316769,
-0.103271942431675));
#39269=CARTESIAN_POINT('Ctrl Pts',(0.0537824343057615,-0.121682422426087,
-0.0961998015229681));
#39270=CARTESIAN_POINT('Ctrl Pts',(0.131183710539696,-0.0221360946094997,
-0.0891276606142618));
#39271=CARTESIAN_POINT('Ctrl Pts',(0.0907331645070544,0.0972968172178819,
-0.0820555197055552));
#39272=CARTESIAN_POINT('Ctrl Pts',(-0.0312294408411226,0.129320730390771,
-0.0749833787968487));
#39273=CARTESIAN_POINT('Ctrl Pts',(-0.125136541870065,0.0451670007571721,
-0.0679112378881423));
#39274=CARTESIAN_POINT('Ctrl Pts',(-0.106624180166971,-0.0795644271486066,
-0.0608390969794357));
#39275=CARTESIAN_POINT('Ctrl Pts',(0.00767581443885381,-0.132815635955666,
-0.0537669560707293));
#39276=CARTESIAN_POINT('Ctrl Pts',(0.115081119114366,-0.066752334306488,
-0.0466948151620227));
#39277=CARTESIAN_POINT('Ctrl Pts',(0.119098772267712,0.0592857558522358,
-0.0396226742533163));
#39278=CARTESIAN_POINT('Ctrl Pts',(0.0161251967291956,0.132051102223579,
-0.0325505333446097));
#39279=CARTESIAN_POINT('Ctrl Pts',(-0.101341987821342,0.0862083768536969,
-0.0254783924359033));
#39280=CARTESIAN_POINT('Ctrl Pts',(-0.127752712154045,-0.0371251696466164,
-0.0184062515271968));
#39281=CARTESIAN_POINT('Ctrl Pts',(-0.0394199316510981,-0.127023417009613,
-0.0113341106184904));
#39282=CARTESIAN_POINT('Ctrl Pts',(0.0843761786218501,-0.102966946885977,
-0.00426196970978389));
#39283=CARTESIAN_POINT('Ctrl Pts',(0.132274844748113,0.0139098892309243,
0.00281017119892267));
#39284=CARTESIAN_POINT('Ctrl Pts',(0.0851225995860365,0.083017739882071,
0.00752493180472693));
#39285=CARTESIAN_POINT('Ctrl Pts',(0.0521473962988379,0.100182179696273,
0.00988231210762909));
#39286=CARTESIAN_POINT('Ctrl Pts',(0.0677908815531574,-0.100829789141135,
-0.36));
#39287=CARTESIAN_POINT('Ctrl Pts',(0.100979247033071,-0.0785162588604907,
-0.357642619697098));
#39288=CARTESIAN_POINT('Ctrl Pts',(0.143079097992708,0.00103106869762737,
-0.352927859091293));
#39289=CARTESIAN_POINT('Ctrl Pts',(0.0778233433430106,0.120218849138505,
-0.345855718182587));
#39290=CARTESIAN_POINT('Ctrl Pts',(-0.0574114192927385,0.131054130678874,
-0.338783577273881));
#39291=CARTESIAN_POINT('Ctrl Pts',(-0.141035563163412,0.0243305891473894,
-0.331711436365174));
#39292=CARTESIAN_POINT('Ctrl Pts',(-0.0979750645280892,-0.104342814934324,
-0.324639295456468));
#39293=CARTESIAN_POINT('Ctrl Pts',(0.0331128426633168,-0.139229272738928,
-0.317567154547761));
#39294=CARTESIAN_POINT('Ctrl Pts',(0.134448177266342,-0.0490614388126946,
-0.310495013639055));
#39295=CARTESIAN_POINT('Ctrl Pts',(0.115001615758944,0.0851951864251332,
-0.303422872730348));
#39296=CARTESIAN_POINT('Ctrl Pts',(-0.00776054689708998,0.142907802100605,
-0.296350731821642));
#39297=CARTESIAN_POINT('Ctrl Pts',(-0.123550133684839,0.072239744135199,
-0.289278590912935));
#39298=CARTESIAN_POINT('Ctrl Pts',(-0.128346110243909,-0.0633284302188229,
-0.282206450004229));
#39299=CARTESIAN_POINT('Ctrl Pts',(-0.0178393289188684,-0.142003086678724,
-0.275134309095522));
#39300=CARTESIAN_POINT('Ctrl Pts',(0.108693702429388,-0.0931066778562214,
-0.268062168186816));
#39301=CARTESIAN_POINT('Ctrl Pts',(0.13757940373459,0.0394344528902857,
-0.260990027278109));
#39302=CARTESIAN_POINT('Ctrl Pts',(0.0428675840440462,0.136548623487951,
-0.253917886369403));
#39303=CARTESIAN_POINT('Ctrl Pts',(-0.0903552600760858,0.110991404961705,
-0.246845745460696));
#39304=CARTESIAN_POINT('Ctrl Pts',(-0.142405471314287,-0.0142774318509216,
-0.23977360455199));
#39305=CARTESIAN_POINT('Ctrl Pts',(-0.0665225820482806,-0.126719801025659,
-0.232701463643283));
#39306=CARTESIAN_POINT('Ctrl Pts',(0.0691223339056467,-0.125320653292622,
-0.225629322734577));
#39307=CARTESIAN_POINT('Ctrl Pts',(0.142669677692796,-0.0113369263586695,
-0.21855718182587));
#39308=CARTESIAN_POINT('Ctrl Pts',(0.0880465689573824,0.112831575254327,
-0.211485040917164));
#39309=CARTESIAN_POINT('Ctrl Pts',(-0.0456751167734476,0.135635344118462,
-0.204412900008457));
#39310=CARTESIAN_POINT('Ctrl Pts',(-0.138363554037041,0.0365881089193739,
-0.197340759099751));
#39311=CARTESIAN_POINT('Ctrl Pts',(-0.106750040474629,-0.0953288605047495,
-0.190268618191044));
#39312=CARTESIAN_POINT('Ctrl Pts',(0.0207647265540655,-0.141605045621754,
-0.183196477282338));
#39313=CARTESIAN_POINT('Ctrl Pts',(0.129625043481976,-0.0606672143896846,
-0.176124336373631));
#39314=CARTESIAN_POINT('Ctrl Pts',(0.122033843377623,0.0747723469605826,
-0.169052195464925));
#39315=CARTESIAN_POINT('Ctrl Pts',(0.00481084828703748,0.143038521221254,
-0.161980054556218));
#39316=CARTESIAN_POINT('Ctrl Pts',(-0.11673407844254,0.0828028847120661,
-0.154907913647512));
#39317=CARTESIAN_POINT('Ctrl Pts',(-0.133408371001466,-0.0518205494643991,
-0.147835772738805));
#39318=CARTESIAN_POINT('Ctrl Pts',(-0.0302323106620386,-0.139889850448257,
-0.140763631830099));
#39319=CARTESIAN_POINT('Ctrl Pts',(0.100103612545454,-0.102286017787817,
-0.133691490921393));
#39320=CARTESIAN_POINT('Ctrl Pts',(0.140509247885848,0.0272087135083893,
-0.126619350012686));
#39321=CARTESIAN_POINT('Ctrl Pts',(0.0546853001230828,0.13225989995725,
-0.11954720910398));
#39322=CARTESIAN_POINT('Ctrl Pts',(-0.080266391393664,0.118492482069505,
-0.112475068195273));
#39323=CARTESIAN_POINT('Ctrl Pts',(-0.143109003210345,-0.00172525958721913,
-0.105402927286567));
#39324=CARTESIAN_POINT('Ctrl Pts',(-0.0773864787151963,-0.120393097438568,
-0.09833078637786));
#39325=CARTESIAN_POINT('Ctrl Pts',(0.0578578832862097,-0.130903100344747,
-0.0912586454691537));
#39326=CARTESIAN_POINT('Ctrl Pts',(0.141124363585093,-0.0238134921719552,
-0.0841865045604471));
#39327=CARTESIAN_POINT('Ctrl Pts',(0.0976086134813589,0.104669637352373,
-0.0771143636517408));
#39328=CARTESIAN_POINT('Ctrl Pts',(-0.0335959010893207,0.139120213170328,
-0.070042222743034));
#39329=CARTESIAN_POINT('Ctrl Pts',(-0.134618961149971,0.0485896016409335,
-0.0629700818343278));
#39330=CARTESIAN_POINT('Ctrl Pts',(-0.114703795973912,-0.0855935473936899,
-0.0558979409256211));
#39331=CARTESIAN_POINT('Ctrl Pts',(0.00825746141212148,-0.142879950729257,
-0.0488258000169147));
#39332=CARTESIAN_POINT('Ctrl Pts',(0.123801572839036,-0.0718105979627093,
-0.0417536591082082));
#39333=CARTESIAN_POINT('Ctrl Pts',(0.128123670011307,0.0637782277226883,
-0.0346815181995017));
#39334=CARTESIAN_POINT('Ctrl Pts',(0.0173471090025586,0.142057483245022,
-0.0276093772907953));
#39335=CARTESIAN_POINT('Ctrl Pts',(-0.109021337153041,0.0927409528906444,
-0.0205372363820887));
#39336=CARTESIAN_POINT('Ctrl Pts',(-0.137433375872942,-0.0399383880652005,
-0.0134650954733823));
#39337=CARTESIAN_POINT('Ctrl Pts',(-0.042407039288203,-0.136648817236048,
-0.00639295456467579));
#39338=CARTESIAN_POINT('Ctrl Pts',(0.0907699169413835,-0.110769430059584,
0.000679186344030648));
#39339=CARTESIAN_POINT('Ctrl Pts',(0.142298180213051,0.0149639330765786,
0.00775132725273722));
#39340=CARTESIAN_POINT('Ctrl Pts',(0.0915728991340969,0.0893085403586358,
0.0124660878585415));
#39341=CARTESIAN_POINT('Ctrl Pts',(0.0560989476895935,0.107773642733835,
0.0148234681614436));
#39342=CARTESIAN_POINT('',(0.067790881553158,-0.100829789141135,0.));
#39343=CARTESIAN_POINT('Ctrl Pts',(0.0679337041871709,-0.100943471330425,
-3.46944695195361E-18));
#39344=CARTESIAN_POINT('Ctrl Pts',(0.0708938339990077,-0.0985098219994332,
-1.14419870693534E-17));
#39345=CARTESIAN_POINT('Ctrl Pts',(0.0737254124732044,-0.095933412712593,
-1.18874367802339E-17));
#39346=CARTESIAN_POINT('Ctrl Pts',(0.0764147067527201,-0.0932157449020129,
-2.08166817117217E-17));
#39347=CARTESIAN_POINT('Ctrl Pts',(0.0810554232312816,-0.0885260663168612,
-3.46280728413895E-17));
#39348=CARTESIAN_POINT('Ctrl Pts',(0.0852732595024775,-0.0834158971715837,
-1.58022670735932E-16));
#39349=CARTESIAN_POINT('Ctrl Pts',(0.0890425996765434,-0.0779563683780291,
-1.92554305833426E-16));
#39350=CARTESIAN_POINT('Ctrl Pts',(0.0911975676765645,-0.0748351033019154,
-2.12296373459876E-16));
#39351=CARTESIAN_POINT('Ctrl Pts',(0.0932003266707534,-0.0716070928834988,
-2.27733886033849E-16));
#39352=CARTESIAN_POINT('Ctrl Pts',(0.095044588107307,-0.0682903407639059,
-2.22044604925031E-16));
#39353=CARTESIAN_POINT('Ctrl Pts',(0.0974021926190729,-0.0640503834527701,
-2.14771734308641E-16));
#39354=CARTESIAN_POINT('Ctrl Pts',(0.0995023637806551,-0.059663325250277,
-3.65192981336413E-17));
#39355=CARTESIAN_POINT('Ctrl Pts',(0.101333546343106,-0.0551577136988226,
-2.42861286636753E-17));
#39356=CARTESIAN_POINT('Ctrl Pts',(0.102909365942388,-0.0512804208853562,
-1.37589051047546E-17));
#39357=CARTESIAN_POINT('Ctrl Pts',(0.10428670233071,-0.0473107226566473,
-9.1622380330981E-17));
#39358=CARTESIAN_POINT('Ctrl Pts',(0.105448892200982,-0.0432949101284721,
-7.97972798949331E-17));
#39359=CARTESIAN_POINT('Ctrl Pts',(0.10781920041327,-0.0351045845560159,
-5.56797639952959E-17));
#39360=CARTESIAN_POINT('Ctrl Pts',(0.109307890077238,-0.0267026497107712,
-1.7069954850417E-18));
#39361=CARTESIAN_POINT('Ctrl Pts',(0.109844464838531,-0.0182481465350914,
3.46944695195361E-18));
#39362=CARTESIAN_POINT('Ctrl Pts',(0.110056959160744,-0.0148999944199391,
5.51942154351163E-18));
#39363=CARTESIAN_POINT('Ctrl Pts',(0.110119567432312,-0.0115436805931865,
-1.07413084515683E-16));
#39364=CARTESIAN_POINT('Ctrl Pts',(0.110025634756424,-0.0081898243220706,
-1.07552855510562E-16));
#39365=CARTESIAN_POINT('Ctrl Pts',(0.109955686614167,-0.0056923332909582,
-1.07656937730521E-16));
#39366=CARTESIAN_POINT('Ctrl Pts',(0.109798760766269,-0.00319835463005472,
-7.98666086115723E-17));
#39367=CARTESIAN_POINT('Ctrl Pts',(0.109553523057914,-0.000720906621662368,
-7.45931094670027E-17));
#39368=CARTESIAN_POINT('Ctrl Pts',(0.10915585786158,0.00329639909887405,
-6.60418671366053E-17));
#39369=CARTESIAN_POINT('Ctrl Pts',(0.108526039512516,0.00727699845794002,
-2.05422639447697E-16));
#39370=CARTESIAN_POINT('Ctrl Pts',(0.107655189039225,0.011202835378149,
-1.795438797636E-16));
#39371=CARTESIAN_POINT('Ctrl Pts',(0.10653757163122,0.0162411098208689,
-1.45609070770046E-16));
#39372=CARTESIAN_POINT('Ctrl Pts',(0.105023066541607,0.0211894402745884,
5.65088878727566E-18));
#39373=CARTESIAN_POINT('Ctrl Pts',(0.103137300132718,0.0260130755751589,
1.73472347597681E-17));
#39374=CARTESIAN_POINT('Ctrl Pts',(0.102077221044583,0.0287246706522717,
2.39223077457933E-17));
#39375=CARTESIAN_POINT('Ctrl Pts',(0.100898998715108,0.0313981896100301,
-1.25490791261462E-16));
#39376=CARTESIAN_POINT('Ctrl Pts',(0.0996086648583684,0.0340221728306018,
-1.14491749414469E-16));
#39377=CARTESIAN_POINT('Ctrl Pts',(0.0960746445368277,0.0412088477957264,
-8.43671136841687E-17));
#39378=CARTESIAN_POINT('Ctrl Pts',(0.0917319904347132,0.0479689262291156,
-1.24597282830284E-17));
#39379=CARTESIAN_POINT('Ctrl Pts',(0.0866841056713385,0.0541743462277911,
3.55618312575245E-17));
#39380=CARTESIAN_POINT('Ctrl Pts',(0.0843006841303288,0.0571043124194059,
5.82358075480046E-17));
#39381=CARTESIAN_POINT('Ctrl Pts',(0.0817595064060622,0.0599101019712312,
-1.67333414005662E-16));
#39382=CARTESIAN_POINT('Ctrl Pts',(0.0790693991906201,0.0625747390717374,
-1.91686944095437E-16));
#39383=CARTESIAN_POINT('Ctrl Pts',(0.0768099707579552,0.0648127750849705,
-2.12141540850814E-16));
#39384=CARTESIAN_POINT('Ctrl Pts',(0.074443867642926,0.066951872301998,
-1.58281656477731E-16));
#39385=CARTESIAN_POINT('Ctrl Pts',(0.0719929118045308,0.0689684036035129,
-1.48318857196017E-16));
#39386=CARTESIAN_POINT('Ctrl Pts',(0.0662253120462789,0.0737137136841467,
-1.24874355329207E-16));
#39387=CARTESIAN_POINT('Ctrl Pts',(0.0599703372361051,0.077803458929088,
-6.83407560972934E-17));
#39388=CARTESIAN_POINT('Ctrl Pts',(0.0533026344467906,0.0811056968029858,
-2.59124319224036E-17));
#39389=CARTESIAN_POINT('Ctrl Pts',(0.0503616242249232,0.0825622577279471,
-7.19802022201604E-18));
#39390=CARTESIAN_POINT('Ctrl Pts',(0.0473401493969273,0.0838649828103428,
-4.46769184301788E-17));
#39391=CARTESIAN_POINT('Ctrl Pts',(0.0442442935173274,0.08499925362115,
-5.11743425413158E-17));
#39392=CARTESIAN_POINT('Ctrl Pts',(-0.121436917850398,-0.000108937277296349,
-0.015489265014994));
#39393=CARTESIAN_POINT('Ctrl Pts',(-0.121530349830317,-0.0115673596937236,
-0.0148145418344567));
#39394=CARTESIAN_POINT('Ctrl Pts',(-0.120038008132328,-0.0230010134756723,
-0.0141398186539195));
#39395=CARTESIAN_POINT('Ctrl Pts',(-0.116860313322169,-0.0339435694343665,
-0.0134650954733823));
#39396=CARTESIAN_POINT('Ctrl Pts',(-0.105757930344696,-0.0721751977888158,
-0.0111077151704802));
#39397=CARTESIAN_POINT('Ctrl Pts',(-0.0740824848164492,-0.104412007512432,
-0.00875033486757794));
#39398=CARTESIAN_POINT('Ctrl Pts',(-0.0360486026807276,-0.116217181178163,
-0.00639295456467575));
#39399=CARTESIAN_POINT('Ctrl Pts',(-0.00166737589937806,-0.126888622803458,
-0.00426196970978384));
#39400=CARTESIAN_POINT('Ctrl Pts',(0.0379096430528989,-0.120864366850511,
-0.00213098485489197));
#39401=CARTESIAN_POINT('Ctrl Pts',(0.0679337041871702,-0.100943471330426,
-5.55111512312578E-17));
#39402=CARTESIAN_POINT('',(0.044346210742013,0.0851009385824475,-0.36));
#39403=CARTESIAN_POINT('Ctrl Pts',(0.0443462107420133,0.0851009385824474,
-0.36));
#39404=CARTESIAN_POINT('Ctrl Pts',(0.0472347321895696,0.084064207117159,
-0.36));
#39405=CARTESIAN_POINT('Ctrl Pts',(0.0500631488172158,0.0828839262856036,
-0.36));
#39406=CARTESIAN_POINT('Ctrl Pts',(0.0528199889486038,0.0815610794408787,
-0.36));
#39407=CARTESIAN_POINT('Ctrl Pts',(0.0566500870458777,0.0797232386733711,
-0.36));
#39408=CARTESIAN_POINT('Ctrl Pts',(0.0603421530117647,0.0776104895128595,
-0.36));
#39409=CARTESIAN_POINT('Ctrl Pts',(0.0638846748154451,0.0752514261108165,
-0.36));
#39410=CARTESIAN_POINT('Ctrl Pts',(0.0667830113424857,0.0733213435293509,
-0.36));
#39411=CARTESIAN_POINT('Ctrl Pts',(0.0695819521300187,0.0712250066688477,
-0.36));
#39412=CARTESIAN_POINT('Ctrl Pts',(0.0722611521682996,0.068988466672373,
-0.36));
#39413=CARTESIAN_POINT('Ctrl Pts',(0.0755956043605516,0.0662049359214967,
-0.36));
#39414=CARTESIAN_POINT('Ctrl Pts',(0.07874992295072,0.0632012229690666,
-0.36));
#39415=CARTESIAN_POINT('Ctrl Pts',(0.0817119391237418,0.0600052355364048,
-0.36));
#39416=CARTESIAN_POINT('Ctrl Pts',(0.0837123729791141,0.0578467863287764,
-0.36));
#39417=CARTESIAN_POINT('Ctrl Pts',(0.0856265812167712,0.0555985564829102,
-0.36));
#39418=CARTESIAN_POINT('Ctrl Pts',(0.0874451964215827,0.0532745140054675,
-0.36));
#39419=CARTESIAN_POINT('Ctrl Pts',(0.0924541421900231,0.0468734882677171,
-0.36));
#39420=CARTESIAN_POINT('Ctrl Pts',(0.0967196599911628,0.0399291210553705,
-0.36));
#39421=CARTESIAN_POINT('Ctrl Pts',(0.100166287100098,0.0326075249336015,
-0.36));
#39422=CARTESIAN_POINT('Ctrl Pts',(0.101810250072491,0.0291152896140918,
-0.36));
#39423=CARTESIAN_POINT('Ctrl Pts',(0.103267542217023,0.0255365320439791,
-0.36));
#39424=CARTESIAN_POINT('Ctrl Pts',(0.1045271934455,0.0218862937333124,-0.36));
#39425=CARTESIAN_POINT('Ctrl Pts',(0.105493737083066,0.0190854274815981,
-0.36));
#39426=CARTESIAN_POINT('Ctrl Pts',(0.106343760940565,0.0162412541306297,
-0.36));
#39427=CARTESIAN_POINT('Ctrl Pts',(0.107068167562164,0.0133774795105766,
-0.36));
#39428=CARTESIAN_POINT('Ctrl Pts',(0.108109295300662,0.00926162095151662,
-0.36));
#39429=CARTESIAN_POINT('Ctrl Pts',(0.108894004138168,0.00509779462631024,
-0.36));
#39430=CARTESIAN_POINT('Ctrl Pts',(0.109410905526584,0.000907155601495218,
-0.36));
#39431=CARTESIAN_POINT('Ctrl Pts',(0.110126047073022,-0.00489066220269337,
-0.36));
#39432=CARTESIAN_POINT('Ctrl Pts',(0.110329285359757,-0.0107397847686723,
-0.36));
#39433=CARTESIAN_POINT('Ctrl Pts',(0.110052890307653,-0.0165912014529204,
-0.36));
#39434=CARTESIAN_POINT('Ctrl Pts',(0.109857463749946,-0.0207284760227993,
-0.36));
#39435=CARTESIAN_POINT('Ctrl Pts',(0.10942034541147,-0.0248732583397424,
-0.36));
#39436=CARTESIAN_POINT('Ctrl Pts',(0.108756338773778,-0.0289741209316136,
-0.36));
#39437=CARTESIAN_POINT('Ctrl Pts',(0.107635003956189,-0.0358994131581975,
-0.36));
#39438=CARTESIAN_POINT('Ctrl Pts',(0.105869233631456,-0.0427137508429052,
-0.36));
#39439=CARTESIAN_POINT('Ctrl Pts',(0.10351308543783,-0.0493365135573982,
-0.36));
#39440=CARTESIAN_POINT('Ctrl Pts',(0.102033997330004,-0.0534939980477481,
-0.36));
#39441=CARTESIAN_POINT('Ctrl Pts',(0.100321758575276,-0.0575761332536055,
-0.36));
#39442=CARTESIAN_POINT('Ctrl Pts',(0.0983851040604554,-0.0615629288935909,
-0.36));
#39443=CARTESIAN_POINT('Ctrl Pts',(0.0970401561620803,-0.0643316377036621,
-0.36));
#39444=CARTESIAN_POINT('Ctrl Pts',(0.095585606598187,-0.0670559753448776,
-0.36));
#39445=CARTESIAN_POINT('Ctrl Pts',(0.0940333458586794,-0.0697137697496087,
-0.36));
#39446=CARTESIAN_POINT('Ctrl Pts',(0.0895102198836054,-0.0774583055756314,
-0.36));
#39447=CARTESIAN_POINT('Ctrl Pts',(0.0841489978738535,-0.0846669728616559,
-0.36));
#39448=CARTESIAN_POINT('Ctrl Pts',(0.0780314158881196,-0.0911818299894396,
-0.36));
#39449=CARTESIAN_POINT('Ctrl Pts',(0.0748243951975507,-0.0945971142722862,
-0.36));
#39450=CARTESIAN_POINT('Ctrl Pts',(0.0714086645011581,-0.0978215835525157,
-0.36));
#39451=CARTESIAN_POINT('Ctrl Pts',(0.0677908815531574,-0.100829789141135,
-0.36));
#39452=CARTESIAN_POINT('Ctrl Pts',(0.044346210742013,0.0851009385824475,
-0.36));
#39453=CARTESIAN_POINT('Ctrl Pts',(0.0190593750035626,0.0980677190231918,
-0.357869015145108));
#39454=CARTESIAN_POINT('Ctrl Pts',(-0.0473907229385778,0.100665673128455,
-0.353380649987314));
#39455=CARTESIAN_POINT('Ctrl Pts',(-0.0930472695895792,0.0423974729753036,
-0.34848489437946));
#39456=CARTESIAN_POINT('Ctrl Pts',(-0.0959255972774781,0.00552313991188578,
-0.345720123626498));
#39457=CARTESIAN_POINT('Ctrl Pts',(-0.0958786240325138,8.20367901696933E-5,
-0.345312733176438));
#39458=CARTESIAN_POINT('Origin',(-1.13809670924099E-17,0.,-0.36));
#39459=CARTESIAN_POINT('',(-0.0659593141366104,0.0695111466142514,-0.36));
#39460=CARTESIAN_POINT('Ctrl Pts',(-0.0374782951795791,-0.115758143579925,
-0.36));
#39461=CARTESIAN_POINT('Ctrl Pts',(-0.0409945590109367,-0.11423469221382,
-0.36));
#39462=CARTESIAN_POINT('Ctrl Pts',(-0.0444266010530333,-0.11253857797051,
-0.36));
#39463=CARTESIAN_POINT('Ctrl Pts',(-0.047760806536058,-0.110667458896572,
-0.36));
#39464=CARTESIAN_POINT('Ctrl Pts',(-0.0535144001878152,-0.107438606061826,
-0.36));
#39465=CARTESIAN_POINT('Ctrl Pts',(-0.058977397035532,-0.103688991136846,
-0.36));
#39466=CARTESIAN_POINT('Ctrl Pts',(-0.0641055674959587,-0.0994799284445121,
-0.36));
#39467=CARTESIAN_POINT('Ctrl Pts',(-0.067037390860062,-0.0970735676502313,
-0.36));
#39468=CARTESIAN_POINT('Ctrl Pts',(-0.0698523243294171,-0.0945226424495796,
-0.36));
#39469=CARTESIAN_POINT('Ctrl Pts',(-0.0725393605821344,-0.0918427255808781,
-0.36));
#39470=CARTESIAN_POINT('Ctrl Pts',(-0.07597432835866,-0.088416858855616,
-0.36));
#39471=CARTESIAN_POINT('Ctrl Pts',(-0.0792023809783025,-0.0847786310744104,
-0.36));
#39472=CARTESIAN_POINT('Ctrl Pts',(-0.0822045421129473,-0.080952298760896,
-0.36));
#39473=CARTESIAN_POINT('Ctrl Pts',(-0.0847880355765678,-0.0776595692642917,
-0.36));
#39474=CARTESIAN_POINT('Ctrl Pts',(-0.0872062056573671,-0.0742233052644298,
-0.36));
#39475=CARTESIAN_POINT('Ctrl Pts',(-0.0894302752531271,-0.0706834112835403,
-0.36));
#39476=CARTESIAN_POINT('Ctrl Pts',(-0.0939663173730785,-0.0634637144592644,
-0.36));
#39477=CARTESIAN_POINT('Ctrl Pts',(-0.0977132205242399,-0.0557975981886947,
-0.36));
#39478=CARTESIAN_POINT('Ctrl Pts',(-0.100559382367918,-0.0478185100843481,
-0.36));
#39479=CARTESIAN_POINT('Ctrl Pts',(-0.101686523476363,-0.0446586201328015,
-0.36));
#39480=CARTESIAN_POINT('Ctrl Pts',(-0.102671833564592,-0.0414495698489802,
-0.36));
#39481=CARTESIAN_POINT('Ctrl Pts',(-0.103505988409046,-0.0381997328206336,
-0.36));
#39482=CARTESIAN_POINT('Ctrl Pts',(-0.104127151899229,-0.0357797023856622,
-0.36));
#39483=CARTESIAN_POINT('Ctrl Pts',(-0.104663738393444,-0.0333390738383591,
-0.36));
#39484=CARTESIAN_POINT('Ctrl Pts',(-0.105110877135444,-0.0308899932766151,
-0.36));
#39485=CARTESIAN_POINT('Ctrl Pts',(-0.105835927921372,-0.0269187252577624,
-0.36));
#39486=CARTESIAN_POINT('Ctrl Pts',(-0.106327704363669,-0.0229187515367,
-0.36));
#39487=CARTESIAN_POINT('Ctrl Pts',(-0.106572694858759,-0.0189049809525404,
-0.36));
#39488=CARTESIAN_POINT('Ctrl Pts',(-0.106887108737049,-0.0137538212086797,
-0.36));
#39489=CARTESIAN_POINT('Ctrl Pts',(-0.106795218220299,-0.00857972307390588,
-0.36));
#39490=CARTESIAN_POINT('Ctrl Pts',(-0.106312078018921,-0.00342315543767976,
-0.36));
#39491=CARTESIAN_POINT('Ctrl Pts',(-0.106040482163523,-0.000524405977197053,
-0.36));
#39492=CARTESIAN_POINT('Ctrl Pts',(-0.105644824844572,0.00237030729199937,
-0.36));
#39493=CARTESIAN_POINT('Ctrl Pts',(-0.105127745376361,0.00524830605462617,
-0.36));
#39494=CARTESIAN_POINT('Ctrl Pts',(-0.103711546170997,0.0131306912802027,
-0.36));
#39495=CARTESIAN_POINT('Ctrl Pts',(-0.101400453867158,0.0208258966356713,
-0.36));
#39496=CARTESIAN_POINT('Ctrl Pts',(-0.0982585663341195,0.0281823183509716,
-0.36));
#39497=CARTESIAN_POINT('Ctrl Pts',(-0.0967750858904105,0.0316557424107343,
-0.36));
#39498=CARTESIAN_POINT('Ctrl Pts',(-0.0951057330825189,0.0350532838824544,
-0.36));
#39499=CARTESIAN_POINT('Ctrl Pts',(-0.0932543133983396,0.0383561915274667,
-0.36));
#39500=CARTESIAN_POINT('Ctrl Pts',(-0.0916992984606194,0.0411303171186509,
-0.36));
#39501=CARTESIAN_POINT('Ctrl Pts',(-0.0900144697478421,0.0438387400352794,
-0.36));
#39502=CARTESIAN_POINT('Ctrl Pts',(-0.0882142913185504,0.0464527333263584,
-0.36));
#39503=CARTESIAN_POINT('Ctrl Pts',(-0.0839781105678046,0.0526039836035903,
-0.36));
#39504=CARTESIAN_POINT('Ctrl Pts',(-0.0790927371523359,0.0582594033379722,
-0.36));
#39505=CARTESIAN_POINT('Ctrl Pts',(-0.0735935572855504,0.0632715851012407,
-0.36));
#39506=CARTESIAN_POINT('Ctrl Pts',(-0.0711679547302304,0.065482380381123,
-0.36));
#39507=CARTESIAN_POINT('Ctrl Pts',(-0.0686226008669145,0.0675674772847997,
-0.36));
#39508=CARTESIAN_POINT('Ctrl Pts',(-0.0659593141366111,0.0695111466142507,
-0.36));
#39509=CARTESIAN_POINT('Origin',(0.,0.,-0.36));
#39510=CARTESIAN_POINT('Origin',(0.,0.,-0.466687266823562));
#39511=CARTESIAN_POINT('Ctrl Pts',(-0.0659593141366105,0.0695111466142513,
-0.36));
#39512=CARTESIAN_POINT('Ctrl Pts',(-0.0847646433244671,0.0516667191265611,
-0.358062422274521));
#39513=CARTESIAN_POINT('Ctrl Pts',(-0.0956440567215446,0.0257261722731044,
-0.356124844549042));
#39514=CARTESIAN_POINT('Ctrl Pts',(-0.095872656538109,-8.6175248921171E-5,
-0.354187266823562));
#39515=CARTESIAN_POINT('Ctrl Pts',(-0.083632211506372,0.0881357089865025,
-0.374823468161444));
#39516=CARTESIAN_POINT('Ctrl Pts',(-0.112642290239959,0.0606079671851011,
-0.372466087858542));
#39517=CARTESIAN_POINT('Ctrl Pts',(-0.14091032653339,-0.0248385438731813,
-0.367751327252738));
#39518=CARTESIAN_POINT('Ctrl Pts',(-0.0567215063177935,-0.131497930301921,
-0.360679186344031));
#39519=CARTESIAN_POINT('Ctrl Pts',(0.0784298127526211,-0.119666359434824,
-0.353607045435325));
#39520=CARTESIAN_POINT('Ctrl Pts',(0.143117945131048,-0.000509442566161793,
-0.346534904526617));
#39521=CARTESIAN_POINT('Ctrl Pts',(0.0792351761535744,0.119198667837268,
-0.339462763617912));
#39522=CARTESIAN_POINT('Ctrl Pts',(-0.0558314673825238,0.131772923774124,
-0.332390622709204));
#39523=CARTESIAN_POINT('Ctrl Pts',(-0.140740043976632,0.025991892761529,
-0.325318481800499));
#39524=CARTESIAN_POINT('Ctrl Pts',(-0.0992120329567224,-0.103153117192596,
-0.318246340891791));
#39525=CARTESIAN_POINT('Ctrl Pts',(0.031445472711221,-0.139621098347674,
-0.311174199983086));
#39526=CARTESIAN_POINT('Ctrl Pts',(0.133853151494439,-0.05066114897936,
-0.304102059074379));
#39527=CARTESIAN_POINT('Ctrl Pts',(0.116010948020474,0.0838133411859342,
-0.297029918165673));
#39528=CARTESIAN_POINT('Ctrl Pts',(-0.00605227524711941,0.142991225558366,
-0.289957777256966));
#39529=CARTESIAN_POINT('Ctrl Pts',(-0.12267829001528,0.0737103367492016,
-0.282885636348259));
#39530=CARTESIAN_POINT('Ctrl Pts',(-0.129093564080224,-0.0617901475075677,
-0.275813495439553));
#39531=CARTESIAN_POINT('Ctrl Pts',(-0.0195347836114904,-0.14177993796111,
-0.268741354530847));
#39532=CARTESIAN_POINT('Ctrl Pts',(0.10757349863316,-0.0943986737283372,
-0.26166921362214));
#39533=CARTESIAN_POINT('Ctrl Pts',(0.138040756604721,0.0377877633064989,
-0.254597072713434));
#39534=CARTESIAN_POINT('Ctrl Pts',(0.0444960554859608,0.136026707539486,
-0.247524931804727));
#39535=CARTESIAN_POINT('Ctrl Pts',(-0.0890226582677377,0.112063070275597,
-0.240452790896021));
#39536=CARTESIAN_POINT('Ctrl Pts',(-0.142565903491056,-0.0125749041412679,
-0.233380649987314));
#39537=CARTESIAN_POINT('Ctrl Pts',(-0.0680319245716216,-0.125915932825319,
-0.226308509078608));
#39538=CARTESIAN_POINT('Ctrl Pts',(0.0676200343668064,-0.126137607550046,
-0.219236368169901));
#39539=CARTESIAN_POINT('Ctrl Pts',(0.142524043916613,-0.0130407793433053,
-0.212164227261195));
#39540=CARTESIAN_POINT('Ctrl Pts',(0.0893884348657091,0.111771520160272,
-0.205092086352488));
#39541=CARTESIAN_POINT('Ctrl Pts',(-0.0440512463399878,0.136171409372038,
-0.198019945443782));
#39542=CARTESIAN_POINT('Ctrl Pts',(-0.137916518725782,0.0382387092123,-0.190947804535075));
#39543=CARTESIAN_POINT('Ctrl Pts',(-0.107881444420903,-0.0940465787220441,
-0.183875663626369));
#39544=CARTESIAN_POINT('Ctrl Pts',(0.0190713051159471,-0.141843048316256,
-0.176803522717662));
#39545=CARTESIAN_POINT('Ctrl Pts',(0.128890926975957,-0.0622116866027405,
-0.169731381808955));
#39546=CARTESIAN_POINT('Ctrl Pts',(0.122918541674049,0.0733089157807597,
-0.162659240900249));
#39547=CARTESIAN_POINT('Ctrl Pts',(0.00651957295741905,0.142970837077603,
-0.155587099991542));
#39548=CARTESIAN_POINT('Ctrl Pts',(-0.115736397526259,0.0841917524929431,
-0.148514959082836));
#39549=CARTESIAN_POINT('Ctrl Pts',(-0.134018023195025,-0.050222848498276,
-0.14144281817413));
#39550=CARTESIAN_POINT('Ctrl Pts',(-0.0319016001457418,-0.139518648620136,
-0.134370677265423));
#39551=CARTESIAN_POINT('Ctrl Pts',(0.0988743262848422,-0.103474787844967,
-0.127298536356717));
#39552=CARTESIAN_POINT('Ctrl Pts',(0.140824326054265,0.0255279206178999,
-0.12022639544801));
#39553=CARTESIAN_POINT('Ctrl Pts',(0.0562616762174438,0.131597078231438,
-0.113154254539304));
#39554=CARTESIAN_POINT('Ctrl Pts',(-0.0788448723527147,0.119443060420805,
-0.106082113630597));
#39555=CARTESIAN_POINT('Ctrl Pts',(-0.143119427000951,-1.51941259976048E-5,
-0.0990099727218907));
#39556=CARTESIAN_POINT('Ctrl Pts',(-0.0788194185783735,-0.119459934035312,
-0.0919378318131843));
#39557=CARTESIAN_POINT('Ctrl Pts',(0.0562896220605368,-0.131584950015693,
-0.0848656909044778));
#39558=CARTESIAN_POINT('Ctrl Pts',(0.140829888105883,-0.0254982124362326,
-0.0777935499957713));
#39559=CARTESIAN_POINT('Ctrl Pts',(0.0988520446283971,0.103496335460187,
-0.0707214090870648));
#39560=CARTESIAN_POINT('Ctrl Pts',(-0.0319308144085461,0.139510902617143,
-0.0636492681783583));
#39561=CARTESIAN_POINT('Ctrl Pts',(-0.134029630703973,0.0501961269752127,
-0.0565771272696519));
#39562=CARTESIAN_POINT('Ctrl Pts',(-0.115716724825556,-0.0842198198972059,
-0.0495049863609454));
#39563=CARTESIAN_POINT('Ctrl Pts',(0.00654668273591539,-0.142962922239377,
-0.0424328454522389));
#39564=CARTESIAN_POINT('Ctrl Pts',(0.122940460166638,-0.0732951485999077,
-0.0353607045435324));
#39565=CARTESIAN_POINT('Ctrl Pts',(0.128865671478577,0.0622627052466987,
-0.028288563634826));
#39566=CARTESIAN_POINT('Ctrl Pts',(0.0190639912086942,0.141802106288977,
-0.0212164227261194));
#39567=CARTESIAN_POINT('Ctrl Pts',(-0.107945428332621,0.0941106766245759,
-0.014144281817413));
#39568=CARTESIAN_POINT('Ctrl Pts',(-0.137820628598294,-0.038446686700647,
-0.00707214090870644));
#39569=CARTESIAN_POINT('Ctrl Pts',(-0.0754254682766369,-0.103308324795554,
-0.00235738030290216));
#39570=CARTESIAN_POINT('Ctrl Pts',(-0.0373723213044952,-0.115609513450726,
0.));
#39571=CARTESIAN_POINT('Ctrl Pts',(-0.0777412457164515,0.0819275215290854,
-0.369882312107629));
#39572=CARTESIAN_POINT('Ctrl Pts',(-0.104707884747748,0.056338805161843,
-0.367524931804727));
#39573=CARTESIAN_POINT('Ctrl Pts',(-0.130984750034776,-0.0230889427375329,
-0.362810171198923));
#39574=CARTESIAN_POINT('Ctrl Pts',(-0.0527261025462999,-0.122235353181203,
-0.355738030290216));
#39575=CARTESIAN_POINT('Ctrl Pts',(0.0729052985072893,-0.111237185831287,
-0.34866588938151));
#39576=CARTESIAN_POINT('Ctrl Pts',(0.133036866279911,-0.000473557962907169,
-0.341593748472803));
#39577=CARTESIAN_POINT('Ctrl Pts',(0.0736539329498896,0.110802437942284,
-0.334521607564097));
#39578=CARTESIAN_POINT('Ctrl Pts',(-0.0518987570257442,0.122490976399911,
-0.32744946665539));
#39579=CARTESIAN_POINT('Ctrl Pts',(-0.130826462003793,0.0241610509325787,
-0.320377325746684));
#39580=CARTESIAN_POINT('Ctrl Pts',(-0.0922236407861768,-0.0958871191571506,
-0.313305184837977));
#39581=CARTESIAN_POINT('Ctrl Pts',(0.0292304863961032,-0.12978633373841,
-0.306233043929271));
#39582=CARTESIAN_POINT('Ctrl Pts',(0.124424675048295,-0.0470926304607176,
-0.299160903020564));
#39583=CARTESIAN_POINT('Ctrl Pts',(0.107839257786109,0.0779096168102174,
-0.292088762111858));
#39584=CARTESIAN_POINT('Ctrl Pts',(-0.00562595928835486,0.13291907270182,
-0.285016621203152));
#39585=CARTESIAN_POINT('Ctrl Pts',(-0.114036959161667,0.0685182574733831,
-0.277944480294445));
#39586=CARTESIAN_POINT('Ctrl Pts',(-0.120000348009553,-0.057437713934847,
-0.270872339385738));
#39587=CARTESIAN_POINT('Ctrl Pts',(-0.0181587738193776,-0.131793106940118,
-0.263800198477032));
#39588=CARTESIAN_POINT('Ctrl Pts',(0.0999961335373955,-0.0877493295637964,
-0.256728057568325));
#39589=CARTESIAN_POINT('Ctrl Pts',(0.128317309620287,0.0351260326538398,
-0.249655916659619));
#39590=CARTESIAN_POINT('Ctrl Pts',(0.0413617997257353,0.126445128071512,
-0.242583775750912));
#39591=CARTESIAN_POINT('Ctrl Pts',(-0.0827519950276166,0.104169464433825,
-0.235511634842206));
#39592=CARTESIAN_POINT('Ctrl Pts',(-0.132523709877523,-0.0116891410031967,
-0.228439493933499));
#39593=CARTESIAN_POINT('Ctrl Pts',(-0.0632398267297108,-0.117046545787487,
-0.221367353024793));
#39594=CARTESIAN_POINT('Ctrl Pts',(0.0628569496415179,-0.117252605975705,
-0.214295212116086));
#39595=CARTESIAN_POINT('Ctrl Pts',(0.132484798847864,-0.0121222004416881,
-0.20722307120738));
#39596=CARTESIAN_POINT('Ctrl Pts',(0.0830920067033574,0.103898450804675,
-0.200150930298674));
#39597=CARTESIAN_POINT('Ctrl Pts',(-0.0409483224722811,0.126579637257834,
-0.193078789389967));
#39598=CARTESIAN_POINT('Ctrl Pts',(-0.12820182292802,0.0355452144001576,
-0.186006648481261));
#39599=CARTESIAN_POINT('Ctrl Pts',(-0.100282387944889,-0.0874220357626795,
-0.178934507572554));
#39600=CARTESIAN_POINT('Ctrl Pts',(0.0177279422658734,-0.131851771867642,
-0.171862366663848));
#39601=CARTESIAN_POINT('Ctrl Pts',(0.119811984451657,-0.05782956025562,
-0.164790225755141));
#39602=CARTESIAN_POINT('Ctrl Pts',(0.11426028774406,0.0681451121794678,
-0.157718084846435));
#39603=CARTESIAN_POINT('Ctrl Pts',(0.0060603410351095,0.132900120364386,
-0.150645943937728));
#39604=CARTESIAN_POINT('Ctrl Pts',(-0.107584046342482,0.078261373219263,
-0.143573803029022));
#39605=CARTESIAN_POINT('Ctrl Pts',(-0.124577933358174,-0.046685203408583,
-0.136501662120315));
#39606=CARTESIAN_POINT('Ctrl Pts',(-0.0296544846896594,-0.129691100462874,
-0.129429521211609));
#39607=CARTESIAN_POINT('Ctrl Pts',(0.0919097218201968,-0.0961861316641179,
-0.122357380302902));
#39608=CARTESIAN_POINT('Ctrl Pts',(0.130904807339743,0.0237297605030454,
-0.115285239394196));
#39609=CARTESIAN_POINT('Ctrl Pts',(0.0522986623988346,0.122327517233929,
-0.108213098485489));
#39610=CARTESIAN_POINT('Ctrl Pts',(-0.0732911217418617,0.111029615767021,
-0.101140957576783));
#39611=CARTESIAN_POINT('Ctrl Pts',(-0.133038243768442,-1.41238676029155E-5,
-0.0940688166680761));
#39612=CARTESIAN_POINT('Ctrl Pts',(-0.0732674609048485,-0.111045300821714,
-0.0869966757593698));
#39613=CARTESIAN_POINT('Ctrl Pts',(0.0523246397658751,-0.122316243317057,
-0.0799245348506631));
#39614=CARTESIAN_POINT('Ctrl Pts',(0.130909977606244,-0.0237021449347227,
-0.0728523939419569));
#39615=CARTESIAN_POINT('Ctrl Pts',(0.0918890096604021,0.0962061614877861,
-0.0657802530332501));
#39616=CARTESIAN_POINT('Ctrl Pts',(-0.0296816411302489,0.129683900080257,
-0.058708112124544));
#39617=CARTESIAN_POINT('Ctrl Pts',(-0.124588723246293,0.0466603641217457,
-0.0516359712158372));
#39618=CARTESIAN_POINT('Ctrl Pts',(-0.107565759366307,-0.0782874635848309,
-0.0445638303071309));
#39619=CARTESIAN_POINT('Ctrl Pts',(0.0060855412290717,-0.132892763039114,
-0.0374916893984244));
#39620=CARTESIAN_POINT('Ctrl Pts',(0.114280662320881,-0.0681323147444817,
-0.0304195484897179));
#39621=CARTESIAN_POINT('Ctrl Pts',(0.119788507925182,0.0578769851994863,
-0.0233474075810114));
#39622=CARTESIAN_POINT('Ctrl Pts',(0.017721143542622,0.131813713754082,
-0.0162752666723049));
#39623=CARTESIAN_POINT('Ctrl Pts',(-0.100341864896571,0.0874816186757801,
-0.00920312576359841));
#39624=CARTESIAN_POINT('Ctrl Pts',(-0.128112687201144,-0.0357385421710475,
-0.0021309848548919));
#39625=CARTESIAN_POINT('Ctrl Pts',(-0.0701125769240916,-0.0960313940983636,
0.00258377575091239));
#39626=CARTESIAN_POINT('Ctrl Pts',(-0.0347398539533484,-0.10746609984895,
0.00494115605381455));
#39627=CARTESIAN_POINT('Ctrl Pts',(-0.071850279926531,0.0757193340716684,
-0.364941156053815));
#39628=CARTESIAN_POINT('Ctrl Pts',(-0.0967734792555375,0.0520696431385851,
-0.362583775750912));
#39629=CARTESIAN_POINT('Ctrl Pts',(-0.121059173536162,-0.0213393416018847,
-0.357869015145108));
#39630=CARTESIAN_POINT('Ctrl Pts',(-0.0487306987748063,-0.112972776060485,
-0.350796874236402));
#39631=CARTESIAN_POINT('Ctrl Pts',(0.0673807842619576,-0.10280801222775,
-0.343724733327695));
#39632=CARTESIAN_POINT('Ctrl Pts',(0.122955787428773,-0.00043767335965257,
-0.336652592418989));
#39633=CARTESIAN_POINT('Ctrl Pts',(0.0680726897462049,0.102406208047299,
-0.329580451510282));
#39634=CARTESIAN_POINT('Ctrl Pts',(-0.0479660466689646,0.113209029025698,
-0.322508310601576));
#39635=CARTESIAN_POINT('Ctrl Pts',(-0.120912880030953,0.0223302091036286,
-0.315436169692869));
#39636=CARTESIAN_POINT('Ctrl Pts',(-0.085235248615631,-0.0886211211217054,
-0.308364028784163));
#39637=CARTESIAN_POINT('Ctrl Pts',(0.0270155000809852,-0.119951569129147,
-0.301291887875456));
#39638=CARTESIAN_POINT('Ctrl Pts',(0.11499619860215,-0.0435241119420751,
-0.29421974696675));
#39639=CARTESIAN_POINT('Ctrl Pts',(0.0996675675517452,0.0720058924345007,
-0.287147606058044));
#39640=CARTESIAN_POINT('Ctrl Pts',(-0.00519964332959026,0.122846919845274,
-0.280075465149336));
#39641=CARTESIAN_POINT('Ctrl Pts',(-0.105395628308053,0.0633261781975646,
-0.273003324240631));
#39642=CARTESIAN_POINT('Ctrl Pts',(-0.110907131938881,-0.0530852803621263,
-0.265931183331924));
#39643=CARTESIAN_POINT('Ctrl Pts',(-0.0167827640272648,-0.121806275919127,
-0.258859042423217));
#39644=CARTESIAN_POINT('Ctrl Pts',(0.0924187684416306,-0.0810999853992555,
-0.251786901514511));
#39645=CARTESIAN_POINT('Ctrl Pts',(0.118593862635852,0.0324643020011807,
-0.244714760605804));
#39646=CARTESIAN_POINT('Ctrl Pts',(0.03822754396551,0.116863548603539,-0.237642619697098));
#39647=CARTESIAN_POINT('Ctrl Pts',(-0.0764813317874957,0.0962758585920524,
-0.230570478788392));
#39648=CARTESIAN_POINT('Ctrl Pts',(-0.122481516263989,-0.0108033778651255,
-0.223498337879685));
#39649=CARTESIAN_POINT('Ctrl Pts',(-0.0584477288878,-0.108177158749654,
-0.216426196970979));
#39650=CARTESIAN_POINT('Ctrl Pts',(0.0580938649162294,-0.108367604401363,
-0.209354056062272));
#39651=CARTESIAN_POINT('Ctrl Pts',(0.122445553779115,-0.0112036215400709,
-0.202281915153565));
#39652=CARTESIAN_POINT('Ctrl Pts',(0.0767955785410057,0.0960253814490789,
-0.195209774244859));
#39653=CARTESIAN_POINT('Ctrl Pts',(-0.0378453986045744,0.116987865143631,
-0.188137633336152));
#39654=CARTESIAN_POINT('Ctrl Pts',(-0.118487127130257,0.0328517195880153,
-0.181065492427446));
#39655=CARTESIAN_POINT('Ctrl Pts',(-0.0926833314688766,-0.080797492803315,
-0.173993351518739));
#39656=CARTESIAN_POINT('Ctrl Pts',(0.0163845794157999,-0.121860495419028,
-0.166921210610033));
#39657=CARTESIAN_POINT('Ctrl Pts',(0.110733041927356,-0.0534474339084993,
-0.159849069701326));
#39658=CARTESIAN_POINT('Ctrl Pts',(0.10560203381407,0.0629813085781758,
-0.15277692879262));
#39659=CARTESIAN_POINT('Ctrl Pts',(0.00560110911279988,0.12282940365117,
-0.145704787883913));
#39660=CARTESIAN_POINT('Ctrl Pts',(-0.0994316951587051,0.0723309939455828,
-0.138632646975207));
#39661=CARTESIAN_POINT('Ctrl Pts',(-0.115137843521322,-0.0431475583188898,
-0.1315605060665));
#39662=CARTESIAN_POINT('Ctrl Pts',(-0.027407369233577,-0.119863552305612,
-0.124488365157794));
#39663=CARTESIAN_POINT('Ctrl Pts',(0.0849451173555514,-0.0888974754832685,
-0.117416224249088));
#39664=CARTESIAN_POINT('Ctrl Pts',(0.120985288625221,0.021931600388191,
-0.110344083340381));
#39665=CARTESIAN_POINT('Ctrl Pts',(0.0483356485802257,0.113057956236419,
-0.103271942431675));
#39666=CARTESIAN_POINT('Ctrl Pts',(-0.0677373711310089,0.102616171113238,
-0.0961998015229683));
#39667=CARTESIAN_POINT('Ctrl Pts',(-0.122957060535933,-1.30536092081419E-5,
-0.0891276606142616));
#39668=CARTESIAN_POINT('Ctrl Pts',(-0.0677155032313236,-0.102630667608116,
-0.0820555197055553));
#39669=CARTESIAN_POINT('Ctrl Pts',(0.0483596574712134,-0.11304753661842,
-0.0749833787968486));
#39670=CARTESIAN_POINT('Ctrl Pts',(0.120990067106604,-0.0219060774332128,
-0.0679112378881423));
#39671=CARTESIAN_POINT('Ctrl Pts',(0.0849259746924071,0.088915987515385,
-0.0608390969794358));
#39672=CARTESIAN_POINT('Ctrl Pts',(-0.0274324678519518,0.11985689754337,
-0.0537669560707292));
#39673=CARTESIAN_POINT('Ctrl Pts',(-0.115147815788613,0.043124601268279,
-0.0466948151620228));
#39674=CARTESIAN_POINT('Ctrl Pts',(-0.0994147939070581,-0.0723551072724562,
-0.0396226742533162));
#39675=CARTESIAN_POINT('Ctrl Pts',(0.00562439972222807,-0.122822603838851,
-0.0325505333446099));
#39676=CARTESIAN_POINT('Ctrl Pts',(0.105620864475125,-0.0629694808890559,
-0.0254783924359033));
#39677=CARTESIAN_POINT('Ctrl Pts',(0.110711344371787,0.0534912651522741,
-0.0184062515271969));
#39678=CARTESIAN_POINT('Ctrl Pts',(0.0163782958765497,0.121825321219186,
-0.0113341106184903));
#39679=CARTESIAN_POINT('Ctrl Pts',(-0.092738301460522,0.0808525607269844,
-0.00426196970978388));
#39680=CARTESIAN_POINT('Ctrl Pts',(-0.118404745803993,-0.0330303976414481,
0.00281017119892266));
#39681=CARTESIAN_POINT('Ctrl Pts',(-0.0647996855715466,-0.0887544634011735,
0.00752493180472693));
#39682=CARTESIAN_POINT('Ctrl Pts',(-0.0321073866022016,-0.0993226862471739,
0.00988231210762909));
#39683=CARTESIAN_POINT('Ctrl Pts',(-0.0659593141366105,0.0695111466142513,
-0.36));
#39684=CARTESIAN_POINT('Ctrl Pts',(-0.0888390737633265,0.047800481115327,
-0.357642619697098));
#39685=CARTESIAN_POINT('Ctrl Pts',(-0.111133597037548,-0.0195897404662363,
-0.352927859091294));
#39686=CARTESIAN_POINT('Ctrl Pts',(-0.0447352950033125,-0.103710198939767,
-0.345855718182587));
#39687=CARTESIAN_POINT('Ctrl Pts',(0.0618562700166257,-0.0943788386242131,
-0.338783577273881));
#39688=CARTESIAN_POINT('Ctrl Pts',(0.112874708577635,-0.000401788756397879,
-0.331711436365174));
#39689=CARTESIAN_POINT('Ctrl Pts',(0.06249144654252,0.0940099781523149,
-0.324639295456468));
#39690=CARTESIAN_POINT('Ctrl Pts',(-0.0440333363121848,0.103927081651485,
-0.317567154547761));
#39691=CARTESIAN_POINT('Ctrl Pts',(-0.110999298058114,0.0204993672746782,
-0.310495013639055));
#39692=CARTESIAN_POINT('Ctrl Pts',(-0.0782468564450852,-0.0813551230862599,
-0.303422872730348));
#39693=CARTESIAN_POINT('Ctrl Pts',(0.0248005137658673,-0.110116804519884,
-0.296350731821642));
#39694=CARTESIAN_POINT('Ctrl Pts',(0.105567722156006,-0.0399555934234326,
-0.289278590912935));
#39695=CARTESIAN_POINT('Ctrl Pts',(0.0914958773173812,0.0661021680587838,
-0.282206450004229));
#39696=CARTESIAN_POINT('Ctrl Pts',(-0.00477332737082577,0.112774766988728,
-0.275134309095522));
#39697=CARTESIAN_POINT('Ctrl Pts',(-0.0967542974544388,0.058134098921746,
-0.268062168186816));
#39698=CARTESIAN_POINT('Ctrl Pts',(-0.101813915868209,-0.0487328467894054,
-0.260990027278109));
#39699=CARTESIAN_POINT('Ctrl Pts',(-0.0154067542351519,-0.111819444898135,
-0.253917886369403));
#39700=CARTESIAN_POINT('Ctrl Pts',(0.0848414033458655,-0.0744506412347145,
-0.246845745460696));
#39701=CARTESIAN_POINT('Ctrl Pts',(0.108870415651418,0.0298025713485215,
-0.23977360455199));
#39702=CARTESIAN_POINT('Ctrl Pts',(0.0350932882052845,0.107281969135566,
-0.232701463643283));
#39703=CARTESIAN_POINT('Ctrl Pts',(-0.0702106685473747,0.08838225275028,
-0.225629322734577));
#39704=CARTESIAN_POINT('Ctrl Pts',(-0.112439322650456,-0.0099176147270544,
-0.21855718182587));
#39705=CARTESIAN_POINT('Ctrl Pts',(-0.0536556310458891,-0.0993077717118213,
-0.211485040917164));
#39706=CARTESIAN_POINT('Ctrl Pts',(0.0533307801909408,-0.0994826028270216,
-0.204412900008458));
#39707=CARTESIAN_POINT('Ctrl Pts',(0.112406308710366,-0.0102850426384537,
-0.197340759099751));
#39708=CARTESIAN_POINT('Ctrl Pts',(0.0704991503786541,0.0881523120934825,
-0.190268618191045));
#39709=CARTESIAN_POINT('Ctrl Pts',(-0.0347424747368677,0.107396093029428,
-0.183196477282338));
#39710=CARTESIAN_POINT('Ctrl Pts',(-0.108772431332495,0.0301582247758729,
-0.176124336373632));
#39711=CARTESIAN_POINT('Ctrl Pts',(-0.0850842749928634,-0.0741729498439504,
-0.169052195464925));
#39712=CARTESIAN_POINT('Ctrl Pts',(0.0150412165657262,-0.111869218970413,
-0.161980054556218));
#39713=CARTESIAN_POINT('Ctrl Pts',(0.101654099403055,-0.0490653075613788,
-0.154907913647512));
#39714=CARTESIAN_POINT('Ctrl Pts',(0.09694377988408,0.0578175049768839,
-0.147835772738805));
#39715=CARTESIAN_POINT('Ctrl Pts',(0.00514187719049035,0.112758686937953,
-0.140763631830099));
#39716=CARTESIAN_POINT('Ctrl Pts',(-0.0912793439749284,0.0664006146719027,
-0.133691490921393));
#39717=CARTESIAN_POINT('Ctrl Pts',(-0.105697753684471,-0.0396099132291967,
-0.126619350012686));
#39718=CARTESIAN_POINT('Ctrl Pts',(-0.0251602537774947,-0.11003600414835,
-0.11954720910398));
#39719=CARTESIAN_POINT('Ctrl Pts',(0.0779805128909062,-0.081608819302419,
-0.112475068195273));
#39720=CARTESIAN_POINT('Ctrl Pts',(0.111065769910699,0.0201334402733364,
-0.105402927286567));
#39721=CARTESIAN_POINT('Ctrl Pts',(0.0443726347616168,0.10378839523891,
-0.0983307863778601));
#39722=CARTESIAN_POINT('Ctrl Pts',(-0.0621836205201562,0.0942027264594536,
-0.0912586454691536));
#39723=CARTESIAN_POINT('Ctrl Pts',(-0.112875877303425,-1.19833508133767E-5,
-0.0841865045604471));
#39724=CARTESIAN_POINT('Ctrl Pts',(-0.0621635455577987,-0.0942160343945172,
-0.0771143636517407));
#39725=CARTESIAN_POINT('Ctrl Pts',(0.0443946751765518,-0.103778829919784,
-0.0700422227430341));
#39726=CARTESIAN_POINT('Ctrl Pts',(0.111070156606965,-0.0201100099317029,
-0.0629700818343277));
#39727=CARTESIAN_POINT('Ctrl Pts',(0.077962939724412,0.0816258135429839,
-0.0558979409256211));
#39728=CARTESIAN_POINT('Ctrl Pts',(-0.0251832945736545,0.110029895006483,
-0.0488258000169148));
#39729=CARTESIAN_POINT('Ctrl Pts',(-0.105706908330933,0.0395888384148121,
-0.0417536591082082));
#39730=CARTESIAN_POINT('Ctrl Pts',(-0.0912638284478091,-0.0664227509600812,
-0.0346815181995017));
#39731=CARTESIAN_POINT('Ctrl Pts',(0.00516325821538433,-0.112752444638587,
-0.0276093772907953));
#39732=CARTESIAN_POINT('Ctrl Pts',(0.0969610666293677,-0.0578066470336301,
-0.0205372363820888));
#39733=CARTESIAN_POINT('Ctrl Pts',(0.101634180818392,0.0491055451050618,
-0.0134650954733823));
#39734=CARTESIAN_POINT('Ctrl Pts',(0.0150354482104775,0.11183692868429,
-0.00639295456467577));
#39735=CARTESIAN_POINT('Ctrl Pts',(-0.0851347380244728,0.0742235027781887,
0.000679186344030675));
#39736=CARTESIAN_POINT('Ctrl Pts',(-0.108696804406843,-0.0303222531118487,
0.0077513272527372));
#39737=CARTESIAN_POINT('Ctrl Pts',(-0.0594867942190013,-0.0814775327039834,
0.0124660878585415));
#39738=CARTESIAN_POINT('Ctrl Pts',(-0.0294749192510548,-0.0911792726453979,
0.0148234681614436));
#39739=CARTESIAN_POINT('',(-0.0373723213044952,-0.115609513450726,0.));
#39740=CARTESIAN_POINT('Ctrl Pts',(-0.0660853196898438,0.0695807828091147,
-3.64291929955129E-17));
#39741=CARTESIAN_POINT('Ctrl Pts',(-0.0685761827410638,0.0677880282189264,
-4.43191730826681E-17));
#39742=CARTESIAN_POINT('Ctrl Pts',(-0.0709697016741088,0.0658738526129303,
-1.8031305068503E-16));
#39743=CARTESIAN_POINT('Ctrl Pts',(-0.0732551202417263,0.0638423633381038,
-1.14491749414469E-16));
#39744=CARTESIAN_POINT('Ctrl Pts',(-0.0764302659566424,0.0610200031117285,
-2.31649688122036E-17));
#39745=CARTESIAN_POINT('Ctrl Pts',(-0.0793969518401287,0.0579714320251634,
1.14889233545085E-16));
#39746=CARTESIAN_POINT('Ctrl Pts',(-0.0821519934974501,0.0547273093807734,
6.59194920871187E-17));
#39747=CARTESIAN_POINT('Ctrl Pts',(-0.0844060535136914,0.0520731037279949,
2.58544949090369E-17));
#39748=CARTESIAN_POINT('Ctrl Pts',(-0.0865187418317461,0.0492864813759394,
-3.25476132089893E-17));
#39749=CARTESIAN_POINT('Ctrl Pts',(-0.0884776822274611,0.0463980921212896,
-4.33680868994202E-17));
#39750=CARTESIAN_POINT('Ctrl Pts',(-0.0909157026986048,0.0428033160133124,
-5.68348245410797E-17));
#39751=CARTESIAN_POINT('Ctrl Pts',(-0.093119879899582,0.0390465411034455,
1.20977856733227E-17));
#39752=CARTESIAN_POINT('Ctrl Pts',(-0.0950862089588394,0.0351579474418293,
-1.90819582357449E-17));
#39753=CARTESIAN_POINT('Ctrl Pts',(-0.0964142002011996,0.0325317245808024,
-4.01396884540584E-17));
#39754=CARTESIAN_POINT('Ctrl Pts',(-0.0976345593006655,0.0298429662492554,
1.52954116439559E-16));
#39755=CARTESIAN_POINT('Ctrl Pts',(-0.0987421319932224,0.0271076808973025,
1.43982048506075E-16));
#39756=CARTESIAN_POINT('Ctrl Pts',(-0.101792681749017,0.0195739775850942,
1.1927058728336E-16));
#39757=CARTESIAN_POINT('Ctrl Pts',(-0.103978837473498,0.0117228968643841,
-3.41615823321009E-18));
#39758=CARTESIAN_POINT('Ctrl Pts',(-0.105273847015717,0.00373491552187747,
3.12250225675825E-17));
#39759=CARTESIAN_POINT('Ctrl Pts',(-0.105891535872104,-7.51622415972098E-5,
4.77480447192829E-17));
#39760=CARTESIAN_POINT('Ctrl Pts',(-0.106305937424425,-0.00391695734714767,
-5.36856847393132E-17));
#39761=CARTESIAN_POINT('Ctrl Pts',(-0.106510652645819,-0.00777298745154552,
-7.11236625150491E-17));
#39762=CARTESIAN_POINT('Ctrl Pts',(-0.106667735066978,-0.010731802828013,
-8.45042003688641E-17));
#39763=CARTESIAN_POINT('Ctrl Pts',(-0.106700871473537,-0.0137001311918125,
-5.41871049115136E-17));
#39764=CARTESIAN_POINT('Ctrl Pts',(-0.106607850951963,-0.0166526766578767,
-3.46944695195361E-17));
#39765=CARTESIAN_POINT('Ctrl Pts',(-0.106474162175508,-0.0208960649351067,
-6.67972039362386E-18));
#39766=CARTESIAN_POINT('Ctrl Pts',(-0.106080766254757,-0.0251148848213788,
1.19106406122488E-16));
#39767=CARTESIAN_POINT('Ctrl Pts',(-0.105422546985642,-0.0292856618406229,
1.24032728532342E-16));
#39768=CARTESIAN_POINT('Ctrl Pts',(-0.104511890193629,-0.0350559979562071,
1.30930489878205E-16));
#39769=CARTESIAN_POINT('Ctrl Pts',(-0.103095019822919,-0.0407345534069762,
6.21935622857477E-17));
#39770=CARTESIAN_POINT('Ctrl Pts',(-0.101216464695186,-0.0462831105067708,
7.45931094670027E-17));
#39771=CARTESIAN_POINT('Ctrl Pts',(-0.0998882206379262,-0.0502062522263654,
8.33602862259234E-17));
#39772=CARTESIAN_POINT('Ctrl Pts',(-0.0983255778215935,-0.0540699920418813,
1.71835757213981E-16));
#39773=CARTESIAN_POINT('Ctrl Pts',(-0.0965569416166795,-0.057828974809559,
1.33573707650214E-16));
#39774=CARTESIAN_POINT('Ctrl Pts',(-0.0935701769319145,-0.0641769150755935,
6.89590977681626E-17));
#39775=CARTESIAN_POINT('Ctrl Pts',(-0.0899945245784868,-0.0702405695530934,
5.19776018937355E-17));
#39776=CARTESIAN_POINT('Ctrl Pts',(-0.085904169907901,-0.0759573404259926,
5.85469173142172E-17));
#39777=CARTESIAN_POINT('Ctrl Pts',(-0.0833364217251236,-0.0795460825284323,
6.2670850100373E-17));
#39778=CARTESIAN_POINT('Ctrl Pts',(-0.080565323852325,-0.08299812931733,
-1.25005049996683E-16));
#39779=CARTESIAN_POINT('Ctrl Pts',(-0.0776047828277375,-0.0862966723715114,
-1.50487261540988E-16));
#39780=CARTESIAN_POINT('Ctrl Pts',(-0.0755487774768718,-0.0885874098121124,
-1.68183879440172E-16));
#39781=CARTESIAN_POINT('Ctrl Pts',(-0.0733996466487082,-0.0908052846402178,
-4.16397669135319E-17));
#39782=CARTESIAN_POINT('Ctrl Pts',(-0.0711749316358312,-0.0929322610972621,
-3.16587034365767E-17));
#39783=CARTESIAN_POINT('Ctrl Pts',(-0.0646923432322698,-0.0991300495039903,
-2.57492147960364E-18));
#39784=CARTESIAN_POINT('Ctrl Pts',(-0.0575518306578732,-0.104581716780799,
1.24711580510287E-17));
#39785=CARTESIAN_POINT('Ctrl Pts',(-0.0498754978577729,-0.109157967797725,
1.78893358460108E-17));
#39786=CARTESIAN_POINT('Ctrl Pts',(-0.0458513303512718,-0.111556977992237,
2.07297097061342E-17));
#39787=CARTESIAN_POINT('Ctrl Pts',(-0.0416791333594398,-0.113715035869443,
-1.34694802438231E-17));
#39788=CARTESIAN_POINT('Ctrl Pts',(-0.0373723213044952,-0.115609513450726,
-8.67361737988404E-19));
#39789=CARTESIAN_POINT('Ctrl Pts',(-0.0373723213044952,-0.115609513450726,
-8.67361737988404E-19));
#39790=CARTESIAN_POINT('Ctrl Pts',(-0.0754254682766369,-0.103308324795554,
-0.00235738030290216));
#39791=CARTESIAN_POINT('Ctrl Pts',(-0.106623048437465,-0.0708775057481003,
-0.00471476060580431));
#39792=CARTESIAN_POINT('Ctrl Pts',(-0.117242638473601,-0.0325692023368365,
-0.00707214090870647));
#39793=CARTESIAN_POINT('Ctrl Pts',(-0.120153648675821,-0.0220682449853316,
-0.00771833893413964));
#39794=CARTESIAN_POINT('Ctrl Pts',(-0.121518425988536,-0.0111256526842618,
-0.0083645369595728));
#39795=CARTESIAN_POINT('Ctrl Pts',(-0.12142737051279,-0.000153818344799855,
-0.00901073498500596));
#39796=CARTESIAN_POINT('Origin',(0.,0.,-0.19));
#39797=CARTESIAN_POINT('Origin',(0.,0.,0.));
#39798=CARTESIAN_POINT('Origin',(0.,0.,0.360944059763209));
#39799=CARTESIAN_POINT('',(0.,0.,0.321888119526417));
#39800=CARTESIAN_POINT('',(-0.13,-1.59204083889156E-17,0.4));
#39801=CARTESIAN_POINT('',(-0.065,-7.9602041944578E-18,0.360944059763209));
#39802=CARTESIAN_POINT('Origin',(0.,0.,0.4));
#39803=CARTESIAN_POINT('Origin',(0.,0.,0.675));
#39804=CARTESIAN_POINT('',(-0.13,-1.59204083889156E-17,0.95));
#39805=CARTESIAN_POINT('',(-0.13,-1.59204083889156E-17,0.675));
#39806=CARTESIAN_POINT('Origin',(0.,0.,0.95));
#39807=CARTESIAN_POINT('Origin',(0.,0.,1.));
#39808=CARTESIAN_POINT('',(-0.18,2.20436423846524E-17,1.));
#39809=CARTESIAN_POINT('',(-0.18,-2.20436423846524E-17,1.));
#39810=CARTESIAN_POINT('Origin',(0.,0.,1.));
#39811=CARTESIAN_POINT('Origin',(0.,0.,0.0275));
#39812=CARTESIAN_POINT('',(0.144337567297406,0.25,0.0336751345948129));
#39813=CARTESIAN_POINT('',(0.0502493781056046,0.25,0.));
#39814=CARTESIAN_POINT('Ctrl Pts',(0.144337567297406,0.25,0.0336751345948129));
#39815=CARTESIAN_POINT('Ctrl Pts',(0.094379570415743,0.25,0.00869613615398113));
#39816=CARTESIAN_POINT('Ctrl Pts',(0.0502493781056046,0.25,-6.93889390390723E-18));
#39817=CARTESIAN_POINT('',(0.191381661893307,0.168517237963823,0.));
#39818=CARTESIAN_POINT('Ctrl Pts',(0.191381661893307,0.168517237963823,
1.73472347597681E-17));
#39819=CARTESIAN_POINT('Ctrl Pts',(0.169316565738238,0.206735105578296,
0.00869613615398118));
#39820=CARTESIAN_POINT('Ctrl Pts',(0.144337567297406,0.25,0.0336751345948129));
#39821=CARTESIAN_POINT('Origin',(0.,0.,0.));
#39822=CARTESIAN_POINT('Origin',(0.,0.,0.0275));
#39823=CARTESIAN_POINT('',(-0.144337567297406,0.25,0.0336751345948129));
#39824=CARTESIAN_POINT('',(-0.191381661893307,0.168517237963823,1.73472347597681E-17));
#39825=CARTESIAN_POINT('Ctrl Pts',(-0.144337567297406,0.25,0.0336751345948129));
#39826=CARTESIAN_POINT('Ctrl Pts',(-0.169316565738238,0.206735105578296,
0.00869613615398114));
#39827=CARTESIAN_POINT('Ctrl Pts',(-0.191381661893307,0.168517237963823,
1.73472347597681E-17));
#39828=CARTESIAN_POINT('',(-0.0502493781056045,0.25,1.04083408558608E-17));
#39829=CARTESIAN_POINT('Ctrl Pts',(-0.0502493781056045,0.25,3.46944695195361E-18));
#39830=CARTESIAN_POINT('Ctrl Pts',(-0.094379570415743,0.25,0.00869613615398118));
#39831=CARTESIAN_POINT('Ctrl Pts',(-0.144337567297406,0.25,0.0336751345948129));
#39832=CARTESIAN_POINT('Origin',(0.,0.,0.));
#39833=CARTESIAN_POINT('Origin',(0.,0.,0.0275));
#39834=CARTESIAN_POINT('',(-0.288675134594813,3.53525079574969E-17,0.0336751345948129));
#39835=CARTESIAN_POINT('',(-0.241631039998912,-0.081482762036177,-1.73472347597681E-17));
#39836=CARTESIAN_POINT('Ctrl Pts',(-0.288675134594813,3.53525079574969E-17,
0.0336751345948129));
#39837=CARTESIAN_POINT('Ctrl Pts',(-0.263696136153981,-0.0432648944217043,
0.00869613615398115));
#39838=CARTESIAN_POINT('Ctrl Pts',(-0.241631039998912,-0.081482762036177,
1.04083408558608E-17));
#39839=CARTESIAN_POINT('',(-0.241631039998912,0.081482762036177,1.73472347597681E-17));
#39840=CARTESIAN_POINT('Ctrl Pts',(-0.241631039998912,0.081482762036177,
1.73472347597681E-17));
#39841=CARTESIAN_POINT('Ctrl Pts',(-0.263696136153981,0.0432648944217042,
0.00869613615398121));
#39842=CARTESIAN_POINT('Ctrl Pts',(-0.288675134594813,3.53525079574969E-17,
0.0336751345948129));
#39843=CARTESIAN_POINT('Origin',(0.,0.,0.));
#39844=CARTESIAN_POINT('Origin',(0.,0.,0.0275));
#39845=CARTESIAN_POINT('',(-0.144337567297407,-0.25,0.0336751345948129));
#39846=CARTESIAN_POINT('',(-0.0502493781056046,-0.25,-2.42861286636753E-17));
#39847=CARTESIAN_POINT('Ctrl Pts',(-0.144337567297407,-0.25,0.0336751345948129));
#39848=CARTESIAN_POINT('Ctrl Pts',(-0.094379570415743,-0.25,0.00869613615398111));
#39849=CARTESIAN_POINT('Ctrl Pts',(-0.0502493781056048,-0.25,-1.73472347597681E-17));
#39850=CARTESIAN_POINT('',(-0.191381661893308,-0.168517237963823,3.46944695195361E-18));
#39851=CARTESIAN_POINT('Ctrl Pts',(-0.191381661893308,-0.168517237963823,
0.));
#39852=CARTESIAN_POINT('Ctrl Pts',(-0.169316565738238,-0.206735105578295,
0.00869613615398107));
#39853=CARTESIAN_POINT('Ctrl Pts',(-0.144337567297407,-0.25,0.0336751345948129));
#39854=CARTESIAN_POINT('Origin',(0.,0.,0.));
#39855=CARTESIAN_POINT('Origin',(0.,0.,0.0275));
#39856=CARTESIAN_POINT('',(0.144337567297406,-0.25,0.0336751345948129));
#39857=CARTESIAN_POINT('',(0.191381661893307,-0.168517237963823,3.46944695195361E-18));
#39858=CARTESIAN_POINT('Ctrl Pts',(0.144337567297406,-0.25,0.0336751345948129));
#39859=CARTESIAN_POINT('Ctrl Pts',(0.169316565738238,-0.206735105578296,
0.00869613615398108));
#39860=CARTESIAN_POINT('Ctrl Pts',(0.191381661893307,-0.168517237963823,
1.73472347597681E-17));
#39861=CARTESIAN_POINT('',(0.0502493781056045,-0.25,-1.73472347597681E-17));
#39862=CARTESIAN_POINT('Ctrl Pts',(0.0502493781056047,-0.25,-6.93889390390723E-18));
#39863=CARTESIAN_POINT('Ctrl Pts',(0.0943795704157429,-0.25,0.0086961361539811));
#39864=CARTESIAN_POINT('Ctrl Pts',(0.144337567297406,-0.25,0.0336751345948129));
#39865=CARTESIAN_POINT('Origin',(0.,0.,0.));
#39866=CARTESIAN_POINT('Origin',(0.,0.,0.0275));
#39867=CARTESIAN_POINT('',(0.241631039998912,-0.0814827620361769,1.04083408558608E-17));
#39868=CARTESIAN_POINT('',(0.288675134594813,0.,0.0336751345948129));
#39869=CARTESIAN_POINT('Ctrl Pts',(0.241631039998912,-0.0814827620361769,
2.08166817117217E-17));
#39870=CARTESIAN_POINT('Ctrl Pts',(0.263696136153981,-0.0432648944217041,
0.00869613615398126));
#39871=CARTESIAN_POINT('Ctrl Pts',(0.288675134594813,0.,0.0336751345948129));
#39872=CARTESIAN_POINT('',(0.241631039998912,0.0814827620361769,-6.93889390390723E-18));
#39873=CARTESIAN_POINT('Origin',(0.,0.,0.));
#39874=CARTESIAN_POINT('Ctrl Pts',(0.288675134594813,0.,0.0336751345948129));
#39875=CARTESIAN_POINT('Ctrl Pts',(0.263696136153981,0.0432648944217043,
0.0086961361539812));
#39876=CARTESIAN_POINT('Ctrl Pts',(0.241631039998912,0.0814827620361769,
3.12250225675825E-17));
#39877=CARTESIAN_POINT('Origin',(-0.144337567297407,-0.25,0.));
#39878=CARTESIAN_POINT('',(0.144337567297406,-0.25,0.966324865405187));
#39879=CARTESIAN_POINT('',(0.144337567297406,-0.25,0.));
#39880=CARTESIAN_POINT('',(0.0502493781056045,-0.25,1.));
#39881=CARTESIAN_POINT('Ctrl Pts',(0.144337567297406,-0.25,0.966324865405187));
#39882=CARTESIAN_POINT('Ctrl Pts',(0.0943795704157427,-0.25,0.991303863846019));
#39883=CARTESIAN_POINT('Ctrl Pts',(0.0502493781056045,-0.25,1.));
#39884=CARTESIAN_POINT('',(-0.0502493781056046,-0.25,1.));
#39885=CARTESIAN_POINT('',(-0.144337567297407,-0.25,1.));
#39886=CARTESIAN_POINT('',(-0.144337567297407,-0.25,0.966324865405187));
#39887=CARTESIAN_POINT('Ctrl Pts',(-0.0502493781056046,-0.25,1.));
#39888=CARTESIAN_POINT('Ctrl Pts',(-0.0943795704157429,-0.25,0.991303863846019));
#39889=CARTESIAN_POINT('Ctrl Pts',(-0.144337567297407,-0.25,0.966324865405187));
#39890=CARTESIAN_POINT('',(-0.144337567297407,-0.25,0.));
#39891=CARTESIAN_POINT('',(-0.144337567297407,-0.25,0.));
#39892=CARTESIAN_POINT('Origin',(-0.288675134594813,3.53525079574969E-17,
0.));
#39893=CARTESIAN_POINT('',(-0.191381661893308,-0.168517237963822,1.));
#39894=CARTESIAN_POINT('Ctrl Pts',(-0.144337567297407,-0.25,0.966324865405187));
#39895=CARTESIAN_POINT('Ctrl Pts',(-0.169316565738239,-0.206735105578295,
0.991303863846019));
#39896=CARTESIAN_POINT('Ctrl Pts',(-0.191381661893308,-0.168517237963823,
1.));
#39897=CARTESIAN_POINT('',(-0.241631039998912,-0.0814827620361775,1.));
#39898=CARTESIAN_POINT('',(-0.288675134594813,3.53525079574969E-17,1.));
#39899=CARTESIAN_POINT('',(-0.288675134594813,3.53525079574969E-17,0.966324865405187));
#39900=CARTESIAN_POINT('Ctrl Pts',(-0.241631039998912,-0.0814827620361772,
1.));
#39901=CARTESIAN_POINT('Ctrl Pts',(-0.263696136153981,-0.0432648944217047,
0.991303863846019));
#39902=CARTESIAN_POINT('Ctrl Pts',(-0.288675134594813,3.53525079574969E-17,
0.966324865405187));
#39903=CARTESIAN_POINT('',(-0.288675134594813,3.53525079574969E-17,0.));
#39904=CARTESIAN_POINT('',(-0.288675134594813,3.53525079574969E-17,0.));
#39905=CARTESIAN_POINT('Origin',(-0.144337567297406,0.25,0.));
#39906=CARTESIAN_POINT('',(-0.241631039998912,0.0814827620361772,1.));
#39907=CARTESIAN_POINT('Ctrl Pts',(-0.288675134594813,3.53525079574969E-17,
0.966324865405187));
#39908=CARTESIAN_POINT('Ctrl Pts',(-0.263696136153981,0.0432648944217045,
0.991303863846019));
#39909=CARTESIAN_POINT('Ctrl Pts',(-0.241631039998912,0.0814827620361772,
1.));
#39910=CARTESIAN_POINT('',(-0.191381661893307,0.168517237963823,1.));
#39911=CARTESIAN_POINT('',(-0.144337567297406,0.25,1.));
#39912=CARTESIAN_POINT('',(-0.144337567297406,0.25,0.966324865405187));
#39913=CARTESIAN_POINT('Ctrl Pts',(-0.191381661893307,0.168517237963823,
1.));
#39914=CARTESIAN_POINT('Ctrl Pts',(-0.169316565738238,0.206735105578295,
0.991303863846019));
#39915=CARTESIAN_POINT('Ctrl Pts',(-0.144337567297406,0.25,0.966324865405187));
#39916=CARTESIAN_POINT('',(-0.144337567297406,0.25,0.));
#39917=CARTESIAN_POINT('',(-0.144337567297406,0.25,0.));
#39918=CARTESIAN_POINT('Origin',(0.,0.,0.));
#39919=CARTESIAN_POINT('',(0.144337567297406,-0.25,0.));
#39920=CARTESIAN_POINT('',(0.144337567297406,0.25,0.));
#39921=CARTESIAN_POINT('',(0.288675134594813,0.,0.));
#39922=CARTESIAN_POINT('Origin',(0.144337567297406,0.25,0.));
#39923=CARTESIAN_POINT('',(-0.0502493781056043,0.25,1.));
#39924=CARTESIAN_POINT('Ctrl Pts',(-0.144337567297406,0.25,0.966324865405187));
#39925=CARTESIAN_POINT('Ctrl Pts',(-0.0943795704157428,0.25,0.991303863846019));
#39926=CARTESIAN_POINT('Ctrl Pts',(-0.0502493781056045,0.25,1.));
#39927=CARTESIAN_POINT('',(0.0502493781056044,0.25,1.));
#39928=CARTESIAN_POINT('',(0.144337567297406,0.25,1.));
#39929=CARTESIAN_POINT('',(0.144337567297406,0.25,0.966324865405187));
#39930=CARTESIAN_POINT('Ctrl Pts',(0.0502493781056046,0.25,1.));
#39931=CARTESIAN_POINT('Ctrl Pts',(0.0943795704157426,0.25,0.991303863846019));
#39932=CARTESIAN_POINT('Ctrl Pts',(0.144337567297406,0.25,0.966324865405187));
#39933=CARTESIAN_POINT('',(0.144337567297406,0.25,0.));
#39934=CARTESIAN_POINT('Origin',(0.,0.,0.9725));
#39935=CARTESIAN_POINT('',(0.241631039998912,0.0814827620361773,1.));
#39936=CARTESIAN_POINT('',(0.288675134594813,0.,0.966324865405187));
#39937=CARTESIAN_POINT('Ctrl Pts',(0.241631039998912,0.0814827620361773,
1.));
#39938=CARTESIAN_POINT('Ctrl Pts',(0.263696136153981,0.0432648944217048,
0.991303863846019));
#39939=CARTESIAN_POINT('Ctrl Pts',(0.288675134594813,0.,0.966324865405187));
#39940=CARTESIAN_POINT('',(0.241631039998912,-0.0814827620361771,1.));
#39941=CARTESIAN_POINT('Origin',(0.,0.,1.));
#39942=CARTESIAN_POINT('Ctrl Pts',(0.288675134594813,0.,0.966324865405187));
#39943=CARTESIAN_POINT('Ctrl Pts',(0.263696136153981,-0.0432648944217043,
0.991303863846019));
#39944=CARTESIAN_POINT('Ctrl Pts',(0.241631039998912,-0.0814827620361776,
1.));
#39945=CARTESIAN_POINT('Origin',(0.,0.,0.9725));
#39946=CARTESIAN_POINT('',(0.191381661893308,0.168517237963823,1.));
#39947=CARTESIAN_POINT('Origin',(0.,0.,1.));
#39948=CARTESIAN_POINT('Ctrl Pts',(0.144337567297406,0.25,0.966324865405187));
#39949=CARTESIAN_POINT('Ctrl Pts',(0.169316565738239,0.206735105578295,
0.991303863846019));
#39950=CARTESIAN_POINT('Ctrl Pts',(0.191381661893308,0.168517237963823,
1.));
#39951=CARTESIAN_POINT('Origin',(0.,0.,0.9725));
#39952=CARTESIAN_POINT('Origin',(0.,0.,1.));
#39953=CARTESIAN_POINT('Origin',(0.,0.,0.9725));
#39954=CARTESIAN_POINT('Origin',(0.,0.,1.));
#39955=CARTESIAN_POINT('Origin',(0.,0.,0.9725));
#39956=CARTESIAN_POINT('Origin',(0.,0.,1.));
#39957=CARTESIAN_POINT('Origin',(0.,0.,0.9725));
#39958=CARTESIAN_POINT('',(0.191381661893308,-0.168517237963823,1.));
#39959=CARTESIAN_POINT('Ctrl Pts',(0.191381661893308,-0.168517237963822,
1.));
#39960=CARTESIAN_POINT('Ctrl Pts',(0.169316565738238,-0.206735105578296,
0.991303863846019));
#39961=CARTESIAN_POINT('Ctrl Pts',(0.144337567297406,-0.25,0.966324865405187));
#39962=CARTESIAN_POINT('Origin',(0.,0.,1.));
#39963=CARTESIAN_POINT('Origin',(0.144337567297406,-0.25,0.));
#39964=CARTESIAN_POINT('',(0.288675134594813,0.,0.));
#39965=CARTESIAN_POINT('',(0.144337567297406,-0.25,1.));
#39966=CARTESIAN_POINT('Origin',(0.105,0.,-0.4));
#39967=CARTESIAN_POINT('',(-0.105,-1.28587913910472E-17,-0.4));
#39968=CARTESIAN_POINT('Origin',(0.,0.,-0.4));
#39969=CARTESIAN_POINT('Origin',(0.,0.,-0.39));
#39970=CARTESIAN_POINT('',(-0.115,-1.40834381901946E-17,-0.39));
#39971=CARTESIAN_POINT('Origin',(0.288675134594813,0.,0.));
#39972=CARTESIAN_POINT('',(0.288675134594813,0.,1.));
#39973=CARTESIAN_POINT('Origin',(0.,0.,1.));
#39974=CARTESIAN_POINT('',(0.,0.,0.));
#39975=CARTESIAN_POINT('Origin',(0.,0.,-0.593));
#39976=CARTESIAN_POINT('',(-0.0965944740297558,-7.73963603528036E-5,-1.12642640831103));
#39977=CARTESIAN_POINT('',(-0.096611016528836,-7.98840753066898E-5,-1.13222359168897));
#39978=CARTESIAN_POINT('',(-0.096675,-1.1839272930757E-17,-0.593));
#39979=CARTESIAN_POINT('',(0.0869541681035032,-0.0426122506771691,-1.149325));
#39980=CARTESIAN_POINT('Ctrl Pts',(-0.0965944740297558,-7.73963603528036E-5,
-1.12642640831103));
#39981=CARTESIAN_POINT('Ctrl Pts',(-0.0964320926110229,0.0217456623633545,
-1.12786083909321));
#39982=CARTESIAN_POINT('Ctrl Pts',(-0.0891113319759391,0.0436686423674009,
-1.12929526987539));
#39983=CARTESIAN_POINT('Ctrl Pts',(-0.0755433113465464,0.0605838294610271,
-1.13072970065757));
#39984=CARTESIAN_POINT('Ctrl Pts',(-0.0555256438879884,0.0855397607267844,
-1.13284599743912));
#39985=CARTESIAN_POINT('Ctrl Pts',(-0.0219097104812664,0.0995953453011509,
-1.13496229422066));
#39986=CARTESIAN_POINT('Ctrl Pts',(0.00990845972240706,0.0963245926632457,
-1.13707859100221));
#39987=CARTESIAN_POINT('Ctrl Pts',(0.0417266299260805,0.0930538400253404,
-1.13919488778376));
#39988=CARTESIAN_POINT('Ctrl Pts',(0.0717470369267054,0.0724567501751636,
-1.14131118456531));
#39989=CARTESIAN_POINT('Ctrl Pts',(0.0862756370450348,0.0439486032544623,
-1.14342748134686));
#39990=CARTESIAN_POINT('Ctrl Pts',(0.0997713324422876,0.0174672310611066,
-1.14539332089791));
#39991=CARTESIAN_POINT('Ctrl Pts',(0.0998996855624999,-0.0158403176033588,
-1.14735916044895));
#39992=CARTESIAN_POINT('Ctrl Pts',(0.0869546080653753,-0.0426125957048284,
-1.149325));
#39993=CARTESIAN_POINT('',(-0.096675,-1.1839272930757E-17,-1.149325));
#39994=CARTESIAN_POINT('Origin',(0.,0.,-1.149325));
#39995=CARTESIAN_POINT('',(-0.096675,-1.1839272930757E-17,-1.179325));
#39996=CARTESIAN_POINT('',(-0.096675,-1.1839272930757E-17,-0.593));
#39997=CARTESIAN_POINT('Origin',(0.,0.,-1.179325));
#39998=CARTESIAN_POINT('',(0.08682622236805,0.0425119128515047,-1.149325));
#39999=CARTESIAN_POINT('Origin',(0.,0.,-1.149325));
#40000=CARTESIAN_POINT('Ctrl Pts',(0.08682622236805,0.0425119128515047,
-1.149325));
#40001=CARTESIAN_POINT('Ctrl Pts',(0.0726941095669478,0.0713753039881243,
-1.14720870321845));
#40002=CARTESIAN_POINT('Ctrl Pts',(0.0431634374388978,0.0923900516972262,
-1.1450924064369));
#40003=CARTESIAN_POINT('Ctrl Pts',(0.0114476307410008,0.0961473177162503,
-1.14297610965536));
#40004=CARTESIAN_POINT('Ctrl Pts',(-0.0202681759568963,0.0999045837352744,
-1.14085981287381));
#40005=CARTESIAN_POINT('Ctrl Pts',(-0.0541691172246404,0.0864043680642206,
-1.13874351609226));
#40006=CARTESIAN_POINT('Ctrl Pts',(-0.0745947204902793,0.061772848111434,
-1.13662721931071));
#40007=CARTESIAN_POINT('Ctrl Pts',(-0.0887620388480758,0.0446882812436053,
-1.1351593434368));
#40008=CARTESIAN_POINT('Ctrl Pts',(-0.0964465189036506,0.0222485651587381,
-1.13369146756288));
#40009=CARTESIAN_POINT('Ctrl Pts',(-0.096611016528836,-7.98840753066898E-5,
-1.13222359168897));
#40010=CARTESIAN_POINT('Origin',(0.,0.,-0.593));
#40011=CARTESIAN_POINT('',(-0.0968310164775401,-1.30139444537575E-5,-1.08642640831103));
#40012=CARTESIAN_POINT('',(-0.0968328216949734,-3.70492603851143E-6,-1.09222359168897));
#40013=CARTESIAN_POINT('',(-0.096675,-1.1839272930757E-17,-0.593));
#40014=CARTESIAN_POINT('Ctrl Pts',(-0.0968310164775401,-1.30139444537575E-5,
-1.08642640831103));
#40015=CARTESIAN_POINT('Ctrl Pts',(-0.0967718957105941,0.0312797356956772,
-1.08849639173725));
#40016=CARTESIAN_POINT('Ctrl Pts',(-0.0802107361021334,0.062626267764312,
-1.09056637516347));
#40017=CARTESIAN_POINT('Ctrl Pts',(-0.0543031633502282,0.0801738568737231,
-1.0926363585897));
#40018=CARTESIAN_POINT('Ctrl Pts',(-0.0278159402458969,0.0981140518944984,
-1.09475265537124));
#40019=CARTESIAN_POINT('Ctrl Pts',(0.00844060388293086,0.101630927348887,
-1.09686895215279));
#40020=CARTESIAN_POINT('Ctrl Pts',(0.0378818670011569,0.0891158908792016,
-1.09898524893434));
#40021=CARTESIAN_POINT('Ctrl Pts',(0.0673231301193828,0.076600854409516,
-1.10110154571589));
#40022=CARTESIAN_POINT('Ctrl Pts',(0.0899491122270068,0.0480539060157556,
-1.10321784249744));
#40023=CARTESIAN_POINT('Ctrl Pts',(0.095411217499768,0.0165326330719422,
-1.10533413927899));
#40024=CARTESIAN_POINT('Ctrl Pts',(0.100873322772529,-0.0149886398718715,
-1.10745043606053));
#40025=CARTESIAN_POINT('Ctrl Pts',(0.0891715512104276,-0.0494842373657385,
-1.10956673284208));
#40026=CARTESIAN_POINT('Ctrl Pts',(0.0656569152152473,-0.0711752102609996,
-1.11168302962363));
#40027=CARTESIAN_POINT('Ctrl Pts',(0.0421422792200671,-0.0928661831562607,
-1.11379932640518));
#40028=CARTESIAN_POINT('Ctrl Pts',(0.00681477879180795,-0.101752531452916,
-1.11591562318673));
#40029=CARTESIAN_POINT('Ctrl Pts',(-0.0241634814538951,-0.0937700019294862,
-1.11803191996828));
#40030=CARTESIAN_POINT('Ctrl Pts',(-0.0551417416995981,-0.0857874724060563,
-1.12014821674983));
#40031=CARTESIAN_POINT('Ctrl Pts',(-0.0817707617627451,-0.0609360650625416,
-1.12226451353137));
#40032=CARTESIAN_POINT('Ctrl Pts',(-0.0918755710391218,-0.03058222241221,
-1.12438081031292));
#40033=CARTESIAN_POINT('Ctrl Pts',(-0.0951313175562236,-0.020802283495351,
-1.12506267631229));
#40034=CARTESIAN_POINT('Ctrl Pts',(-0.0966716630929989,-0.0104511292241676,
-1.12574454231166));
#40035=CARTESIAN_POINT('Ctrl Pts',(-0.0965944740297558,-7.73963603528036E-5,
-1.12642640831103));
#40036=CARTESIAN_POINT('Ctrl Pts',(-0.096611016528836,-7.98840753066898E-5,
-1.13222359168897));
#40037=CARTESIAN_POINT('Ctrl Pts',(-0.0966836818688159,-0.0099432748263196,
-1.13157517078133));
#40038=CARTESIAN_POINT('Ctrl Pts',(-0.0952889348227196,-0.0197849535113047,
-1.1309267498737));
#40039=CARTESIAN_POINT('Ctrl Pts',(-0.0923373744382648,-0.0291337196589252,
-1.13027832896607));
#40040=CARTESIAN_POINT('Ctrl Pts',(-0.0827041598570778,-0.0596459432419781,
-1.12816203218452));
#40041=CARTESIAN_POINT('Ctrl Pts',(-0.0564874654311699,-0.0849075661735644,
-1.12604573540297));
#40042=CARTESIAN_POINT('Ctrl Pts',(-0.0256429766363193,-0.0933758123919359,
-1.12392943862142));
#40043=CARTESIAN_POINT('Ctrl Pts',(0.00520151215853144,-0.101844058610307,
-1.12181314183987));
#40044=CARTESIAN_POINT('Ctrl Pts',(0.040673795322325,-0.0935189281154639,
-1.11969684505832));
#40045=CARTESIAN_POINT('Ctrl Pts',(0.0645295176708119,-0.0722020325036736,
-1.11758054827677));
#40046=CARTESIAN_POINT('Ctrl Pts',(0.0883852400192985,-0.0508851368918835,
-1.11546425149523));
#40047=CARTESIAN_POINT('Ctrl Pts',(0.100624401552479,-0.0165764761631469,
-1.11334795471368));
#40048=CARTESIAN_POINT('Ctrl Pts',(0.0956586130205045,0.0150273819453597,
-1.11123165793213));
#40049=CARTESIAN_POINT('Ctrl Pts',(0.0906928244885304,0.0466312400538666,
-1.10911536115058));
#40050=CARTESIAN_POINT('Ctrl Pts',(0.0685220858914019,0.0755302955421434,
-1.10699906436903));
#40051=CARTESIAN_POINT('Ctrl Pts',(0.0392823152972172,0.0885075508075104,
-1.10488276758748));
#40052=CARTESIAN_POINT('Ctrl Pts',(0.0100425447030326,0.101484806072877,
-1.10276647080593));
#40053=CARTESIAN_POINT('Ctrl Pts',(-0.0262662578882083,0.0985402611153346,
-1.10065017402439));
#40054=CARTESIAN_POINT('Ctrl Pts',(-0.0530332437966072,0.0810198486041363,
-1.09853387724284));
#40055=CARTESIAN_POINT('Ctrl Pts',(-0.0796374715166379,0.06360596996304,
-1.09643044872488));
#40056=CARTESIAN_POINT('Ctrl Pts',(-0.0968155688864563,0.0317929436444108,
-1.09432702020692));
#40057=CARTESIAN_POINT('Ctrl Pts',(-0.0968328216949734,-3.70492603851143E-6,
-1.09222359168897));
#40058=CARTESIAN_POINT('Origin',(0.,0.,-0.593));
#40059=CARTESIAN_POINT('',(-0.0966316008371174,8.59389927197543E-5,-1.04642640831103));
#40060=CARTESIAN_POINT('',(-0.0966173831184959,8.35728303465981E-5,-1.05222359168897));
#40061=CARTESIAN_POINT('',(-0.096675,-1.1839272930757E-17,-0.593));
#40062=CARTESIAN_POINT('Ctrl Pts',(-0.0966316008371174,8.59389927197543E-5,
-1.04642640831103));
#40063=CARTESIAN_POINT('Ctrl Pts',(-0.0967086374933281,0.00904146025168611,
-1.04701564759975));
#40064=CARTESIAN_POINT('Ctrl Pts',(-0.0955657530108521,0.0179776896157913,
-1.04760488688846));
#40065=CARTESIAN_POINT('Ctrl Pts',(-0.0931241231896304,0.0265437297547207,
-1.04819412617718));
#40066=CARTESIAN_POINT('Ctrl Pts',(-0.0843548278772829,0.057309300760937,
-1.05031042295873));
#40067=CARTESIAN_POINT('Ctrl Pts',(-0.0588324876973109,0.08329965024076,
-1.05242671974028));
#40068=CARTESIAN_POINT('Ctrl Pts',(-0.0282313235457831,0.0926264786465709,
-1.05454301652182));
#40069=CARTESIAN_POINT('Ctrl Pts',(0.00236984060574432,0.101953307052382,
-1.05665931330337));
#40070=CARTESIAN_POINT('Ctrl Pts',(0.0380498287288274,0.094616614384181,
-1.05877561008492));
#40071=CARTESIAN_POINT('Ctrl Pts',(0.0624881756074684,0.0739722936785937,
-1.06089190686647));
#40072=CARTESIAN_POINT('Ctrl Pts',(0.0869265224861093,0.0533279729730065,
-1.06300820364802));
#40073=CARTESIAN_POINT('Ctrl Pts',(0.100123228120308,0.0193760242300328,
-1.06512450042957));
#40074=CARTESIAN_POINT('Ctrl Pts',(0.0960419776750078,-0.0123535252285019,
-1.06724079721111));
#40075=CARTESIAN_POINT('Ctrl Pts',(0.0919607272297077,-0.0440830746870368,
-1.06935709399266));
#40076=CARTESIAN_POINT('Ctrl Pts',(0.0706015207049087,-0.0735902248611326,
-1.07147339077421));
#40077=CARTESIAN_POINT('Ctrl Pts',(0.0417342836900796,-0.0873780446853105,
-1.07358968755576));
#40078=CARTESIAN_POINT('Ctrl Pts',(0.0128670466752505,-0.101165864509488,
-1.07570598433731));
#40079=CARTESIAN_POINT('Ctrl Pts',(-0.0235082208296085,-0.0992343539837484,
-1.07782228111886));
#40080=CARTESIAN_POINT('Ctrl Pts',(-0.0507529716286648,-0.082467019364773,
-1.07993857790041));
#40081=CARTESIAN_POINT('Ctrl Pts',(-0.0779977224277213,-0.0656996847457975,
-1.08205487468195));
#40082=CARTESIAN_POINT('Ctrl Pts',(-0.0961119565209748,-0.0340965260335864,
-1.0841711714635));
#40083=CARTESIAN_POINT('Ctrl Pts',(-0.0968101225276843,-0.00211318938389995,
-1.08628746824505));
#40084=CARTESIAN_POINT('Ctrl Pts',(-0.0968254012970081,-0.0014132612605281,
-1.08633378160038));
#40085=CARTESIAN_POINT('Ctrl Pts',(-0.0968323392326173,-0.000713151063858057,
-1.08638009495571));
#40086=CARTESIAN_POINT('Ctrl Pts',(-0.0968310164775401,-1.30139444537575E-5,
-1.08642640831103));
#40087=CARTESIAN_POINT('Ctrl Pts',(-0.0968328216949734,-3.70492603851143E-6,
-1.09222359168897));
#40088=CARTESIAN_POINT('Ctrl Pts',(-0.096850285600455,-0.032189401806551,
-1.09009442664383));
#40089=CARTESIAN_POINT('Ctrl Pts',(-0.0791875082743585,-0.0643577242998591,
-1.08796526159869));
#40090=CARTESIAN_POINT('Ctrl Pts',(-0.0520464468139391,-0.0816568732620622,
-1.08583609655355));
#40091=CARTESIAN_POINT('Ctrl Pts',(-0.0250694207033475,-0.0988514694986514,
-1.083719799772));
#40092=CARTESIAN_POINT('Ctrl Pts',(0.0112710839020407,-0.101356085477478,
-1.08160350299045));
#40093=CARTESIAN_POINT('Ctrl Pts',(0.0403520772773434,-0.0880249422318465,
-1.0794872062089));
#40094=CARTESIAN_POINT('Ctrl Pts',(0.069433070652646,-0.074693798986215,
-1.07737090942735));
#40095=CARTESIAN_POINT('Ctrl Pts',(0.0912545527978629,-0.045526896516125,
-1.07525461264581));
#40096=CARTESIAN_POINT('Ctrl Pts',(0.0958353288144589,-0.013865599655261,
-1.07313831586426));
#40097=CARTESIAN_POINT('Ctrl Pts',(0.100416104831055,0.0177956972056032,
-1.07102201908271));
#40098=CARTESIAN_POINT('Ctrl Pts',(0.0877561747190295,0.0519513884572417,
-1.06890572230116));
#40099=CARTESIAN_POINT('Ctrl Pts',(0.0636462302200924,0.0729782879168203,
-1.06678942551961));
#40100=CARTESIAN_POINT('Ctrl Pts',(0.0395362857211552,0.0940051873763989,
-1.06467312873806));
#40101=CARTESIAN_POINT('Ctrl Pts',(0.00397632683530639,0.101903295043918,
-1.06255683195652));
#40102=CARTESIAN_POINT('Ctrl Pts',(-0.0267680336791695,0.0930599012284323,
-1.06044053517497));
#40103=CARTESIAN_POINT('Ctrl Pts',(-0.0575123941936451,0.084216507412947,
-1.05832423839342));
#40104=CARTESIAN_POINT('Ctrl Pts',(-0.0834411563367478,0.0586316121144577,
-1.05620794161187));
#40105=CARTESIAN_POINT('Ctrl Pts',(-0.0926942234682325,0.0280080651033813,
-1.05409164483032));
#40106=CARTESIAN_POINT('Ctrl Pts',(-0.0954167812986275,0.0189976065684176,
-1.05346896044987));
#40107=CARTESIAN_POINT('Ctrl Pts',(-0.0966956730758621,0.00955093650367408,
-1.05284627606942));
#40108=CARTESIAN_POINT('Ctrl Pts',(-0.0966173831184959,8.35728303465981E-5,
-1.05222359168897));
#40109=CARTESIAN_POINT('Origin',(0.,0.,-0.593));
#40110=CARTESIAN_POINT('',(-0.096532558168651,-4.01631997834981E-5,-1.00642640831103));
#40111=CARTESIAN_POINT('',(-0.096539508889345,-4.74460931573492E-5,-1.01222359168897));
#40112=CARTESIAN_POINT('',(-0.096675,-1.1839272930757E-17,-0.593));
#40113=CARTESIAN_POINT('Ctrl Pts',(-0.096532558168651,-4.01631997834981E-5,
-1.00642640831103));
#40114=CARTESIAN_POINT('Ctrl Pts',(-0.0964626778726808,0.0186229076283818,
-1.00765120024379));
#40115=CARTESIAN_POINT('Ctrl Pts',(-0.0912497818101863,0.0373220779001833,
-1.00887599217655));
#40116=CARTESIAN_POINT('Ctrl Pts',(-0.0811472458103819,0.0528374540286397,
-1.01010078410931));
#40117=CARTESIAN_POINT('Ctrl Pts',(-0.0636912487140321,0.0796462038962325,
-1.01221708089086));
#40118=CARTESIAN_POINT('Ctrl Pts',(-0.0316368472773319,0.0969494861144909,
-1.0143333776724));
#40119=CARTESIAN_POINT('Ctrl Pts',(0.000353889460091694,0.0968325710537681,
-1.01644967445395));
#40120=CARTESIAN_POINT('Ctrl Pts',(0.0323446261975153,0.0967156559930454,
-1.0185659712355));
#40121=CARTESIAN_POINT('Ctrl Pts',(0.0642716982356621,0.0791785436533415,
-1.02068226801705));
#40122=CARTESIAN_POINT('Ctrl Pts',(0.0815312782370999,0.0522429203921152,
-1.0227985647986));
#40123=CARTESIAN_POINT('Ctrl Pts',(0.0987908582385379,0.0253072971308888,
-1.02491486158015));
#40124=CARTESIAN_POINT('Ctrl Pts',(0.101382946203267,-0.0110268370518601,
-1.02703115836169));
#40125=CARTESIAN_POINT('Ctrl Pts',(0.0881218902579705,-0.0401398117892546,
-1.02914745514324));
#40126=CARTESIAN_POINT('Ctrl Pts',(0.0748608343126744,-0.0692527865266491,
-1.03126375192479));
#40127=CARTESIAN_POINT('Ctrl Pts',(0.0457466344573533,-0.0911446018186895,
-1.03338004870634));
#40128=CARTESIAN_POINT('Ctrl Pts',(0.0140964755307833,-0.0958016776657067,
-1.03549634548789));
#40129=CARTESIAN_POINT('Ctrl Pts',(-0.0175536833957866,-0.100458753512724,
-1.03761264226944));
#40130=CARTESIAN_POINT('Ctrl Pts',(-0.0517398013936054,-0.0878810899147185,
-1.03972893905098));
#40131=CARTESIAN_POINT('Ctrl Pts',(-0.0728247351701532,-0.0638218618494113,
-1.04184523583253));
#40132=CARTESIAN_POINT('Ctrl Pts',(-0.0880390030318676,-0.0464614307372775,
-1.04337229332537));
#40133=CARTESIAN_POINT('Ctrl Pts',(-0.0964319546062191,-0.0231229611988117,
-1.0448993508182));
#40134=CARTESIAN_POINT('Ctrl Pts',(-0.0966316008371174,8.59389927197543E-5,
-1.04642640831103));
#40135=CARTESIAN_POINT('Ctrl Pts',(-0.0966173831184959,8.35728303465981E-5,
-1.05222359168897));
#40136=CARTESIAN_POINT('Ctrl Pts',(-0.0964295915905974,-0.0226254788692061,
-1.05072997928787));
#40137=CARTESIAN_POINT('Ctrl Pts',(-0.0884331154221412,-0.0454535933732362,
-1.04923636688677));
#40138=CARTESIAN_POINT('Ctrl Pts',(-0.0738215226618864,-0.0626662176126394,
-1.04774275448568));
#40139=CARTESIAN_POINT('Ctrl Pts',(-0.0531183826041891,-0.0870547545939195,
-1.04562645770413));
#40140=CARTESIAN_POINT('Ctrl Pts',(-0.0191347303689279,-0.100169629832816,
-1.04351016092258));
#40141=CARTESIAN_POINT('Ctrl Pts',(0.0125848936453956,-0.0960119385413782,
-1.04139386414103));
#40142=CARTESIAN_POINT('Ctrl Pts',(0.0443045176597189,-0.0918542472499407,
-1.03927756735948));
#40143=CARTESIAN_POINT('Ctrl Pts',(0.0737601134531046,-0.0704239894281696,
-1.03716127057793));
#40144=CARTESIAN_POINT('Ctrl Pts',(0.0874783414676494,-0.0415236245754575,
-1.03504497379639));
#40145=CARTESIAN_POINT('Ctrl Pts',(0.101196569482194,-0.0126232597227454,
-1.03292867701484));
#40146=CARTESIAN_POINT('Ctrl Pts',(0.0991774297178981,0.0237472121609076,
-1.03081238023329));
#40147=CARTESIAN_POINT('Ctrl Pts',(0.0823444985901786,0.0509515001679581,
-1.02869608345174));
#40148=CARTESIAN_POINT('Ctrl Pts',(0.0655115674624591,0.0781557881750087,
-1.02657978667019));
#40149=CARTESIAN_POINT('Ctrl Pts',(0.0338648449713159,0.0961938923054568,
-1.02446348988864));
#40150=CARTESIAN_POINT('Ctrl Pts',(0.00187992427854601,0.09681496612358,
-1.02234719310709));
#40151=CARTESIAN_POINT('Ctrl Pts',(-0.0301049964142237,0.0974360399417031,
-1.02023089632555));
#40152=CARTESIAN_POINT('Ctrl Pts',(-0.0624281153086202,0.0806400834475018,
-1.018114599544));
#40153=CARTESIAN_POINT('Ctrl Pts',(-0.0803044493353819,0.0541097695880409,
-1.01599830276245));
#40154=CARTESIAN_POINT('Ctrl Pts',(-0.0909327626848177,0.0383362620816862,
-1.01474006573796));
#40155=CARTESIAN_POINT('Ctrl Pts',(-0.0964543450128613,0.0191217990142187,
-1.01348182871346));
#40156=CARTESIAN_POINT('Ctrl Pts',(-0.096539508889345,-4.74460931573492E-5,
-1.01222359168897));
#40157=CARTESIAN_POINT('Origin',(0.,0.,-0.593));
#40158=CARTESIAN_POINT('',(-0.0967783240400222,-6.36632972197126E-5,-0.966426408311032));
#40159=CARTESIAN_POINT('',(-0.0967903835966408,-5.70231646415709E-5,-0.972223591688967));
#40160=CARTESIAN_POINT('',(-0.096675,-1.1839272930757E-17,-0.593));
#40161=CARTESIAN_POINT('Ctrl Pts',(-0.0967783240400222,-6.36632972197126E-5,
-0.966426408311032));
#40162=CARTESIAN_POINT('Ctrl Pts',(-0.0965638778054847,0.0281004551149537,
-0.968286752887833));
#40163=CARTESIAN_POINT('Ctrl Pts',(-0.083560586212758,0.0564370375535735,
-0.970147097464634));
#40164=CARTESIAN_POINT('Ctrl Pts',(-0.0619458247367958,0.0744270572529086,
-0.972007442041436));
#40165=CARTESIAN_POINT('Ctrl Pts',(-0.0373572346895846,0.094892201863463,
-0.974123738822984));
#40166=CARTESIAN_POINT('Ctrl Pts',(-0.0016245794286527,0.10196790524414,
-0.976240035604533));
#40167=CARTESIAN_POINT('Ctrl Pts',(0.028907594321538,0.0924176554789381,
-0.978356332386081));
#40168=CARTESIAN_POINT('Ctrl Pts',(0.0594397680717282,0.0828674057137362,
-0.980472629167629));
#40169=CARTESIAN_POINT('Ctrl Pts',(0.0847714603111776,0.0566912028026555,
-0.982588925949178));
#40170=CARTESIAN_POINT('Ctrl Pts',(0.0933156500194906,0.025862357111442,
-0.984705222730726));
#40171=CARTESIAN_POINT('Ctrl Pts',(0.101859839727804,-0.00496648857977159,
-0.986821519512274));
#40172=CARTESIAN_POINT('Ctrl Pts',(0.0936165269049802,-0.0404479770511177,
-0.988937816293823));
#40173=CARTESIAN_POINT('Ctrl Pts',(0.0723563020911069,-0.0643524482907502,
-0.991054113075372));
#40174=CARTESIAN_POINT('Ctrl Pts',(0.0510960772772336,-0.0882569195303827,
-0.99317040985692));
#40175=CARTESIAN_POINT('Ctrl Pts',(0.0168189404723104,-0.100584373538301,
-0.995286706638468));
#40176=CARTESIAN_POINT('Ctrl Pts',(-0.0147963332778374,-0.0956960844300254,
-0.997403003420017));
#40177=CARTESIAN_POINT('Ctrl Pts',(-0.0464116070279851,-0.0908077953217495,
-0.999519300201565));
#40178=CARTESIAN_POINT('Ctrl Pts',(-0.0753650177233574,-0.0687037630972791,
-1.00163559698311));
#40179=CARTESIAN_POINT('Ctrl Pts',(-0.0884129266930442,-0.0394946382265804,
-1.00375189376466));
#40180=CARTESIAN_POINT('Ctrl Pts',(-0.0939094497773613,-0.0271900896971962,
-1.00464339861345));
#40181=CARTESIAN_POINT('Ctrl Pts',(-0.0965834228265787,-0.0136246894295979,
-1.00553490346224));
#40182=CARTESIAN_POINT('Ctrl Pts',(-0.096532558168651,-4.01631997834981E-5,
-1.00642640831103));
#40183=CARTESIAN_POINT('Ctrl Pts',(-0.096539508889345,-4.74460931573492E-5,
-1.01222359168897));
#40184=CARTESIAN_POINT('Ctrl Pts',(-0.0965975867345704,-0.0131199892464291,
-1.01136553193191));
#40185=CARTESIAN_POINT('Ctrl Pts',(-0.0941273970619773,-0.0261715032790142,
-1.01050747217486));
#40186=CARTESIAN_POINT('Ctrl Pts',(-0.0890243793814782,-0.0380963469727379,
-1.0096494124178));
#40187=CARTESIAN_POINT('Ctrl Pts',(-0.0764384262416856,-0.0675074784493349,
-1.00753311563626));
#40188=CARTESIAN_POINT('Ctrl Pts',(-0.0478369708029737,-0.0900650701778077,
-1.00541681885471));
#40189=CARTESIAN_POINT('Ctrl Pts',(-0.016302663323126,-0.0954510080514942,
-1.00330052207316));
#40190=CARTESIAN_POINT('Ctrl Pts',(0.0152316441567213,-0.100836945925181,
-1.00118422529161));
#40191=CARTESIAN_POINT('Ctrl Pts',(0.0496988036777041,-0.0890512299440807,
-0.999067928510063));
#40192=CARTESIAN_POINT('Ctrl Pts',(0.07133312159954,-0.0654847885278765,
-0.996951631728514));
#40193=CARTESIAN_POINT('Ctrl Pts',(0.0929674395213759,-0.0419183471116724,
-0.994835334946965));
#40194=CARTESIAN_POINT('Ctrl Pts',(0.101768915844065,-0.00657118026036393,
-0.992719038165417));
#40195=CARTESIAN_POINT('Ctrl Pts',(0.0937116492784364,0.0243884923567606,
-0.990602741383869));
#40196=CARTESIAN_POINT('Ctrl Pts',(0.0856543827128077,0.0553481649738856,
-0.98848644460232));
#40197=CARTESIAN_POINT('Ctrl Pts',(0.060738373258861,0.0819203433568267,
-0.986370147820772));
#40198=CARTESIAN_POINT('Ctrl Pts',(0.0303605036494764,0.0919505931829567,
-0.984253851039224));
#40199=CARTESIAN_POINT('Ctrl Pts',(-1.7365959907794E-5,0.101980843009087,
-0.982137554257675));
#40200=CARTESIAN_POINT('Ctrl Pts',(-0.0358570957247298,0.0954691642784059,
-0.980021257476126));
#40201=CARTESIAN_POINT('Ctrl Pts',(-0.0607651617655735,0.075394077245872,
-0.977904960694578));
#40202=CARTESIAN_POINT('Ctrl Pts',(-0.0830543976339355,0.0574296817278774,
-0.976011171026041));
#40203=CARTESIAN_POINT('Ctrl Pts',(-0.0965898337721487,0.0286040520070571,
-0.974117381357504));
#40204=CARTESIAN_POINT('Ctrl Pts',(-0.0967903835966408,-5.70231646415709E-5,
-0.972223591688967));
#40205=CARTESIAN_POINT('Origin',(0.,0.,-0.593));
#40206=CARTESIAN_POINT('',(-0.0967266999094946,8.16697450527169E-5,-0.926426408311032));
#40207=CARTESIAN_POINT('',(-0.09671155539721,8.46130275593083E-5,-0.932223591688967));
#40208=CARTESIAN_POINT('',(-0.096675,-1.1839272930757E-17,-0.593));
#40209=CARTESIAN_POINT('Ctrl Pts',(-0.0967266999094946,8.16697450527169E-5,
-0.926426408311032));
#40210=CARTESIAN_POINT('Ctrl Pts',(-0.0967785360195961,0.00583649577189784,
-0.926806008750327));
#40211=CARTESIAN_POINT('Ctrl Pts',(-0.0963090658617653,0.0115828782139499,
-0.927185609189623));
#40212=CARTESIAN_POINT('Ctrl Pts',(-0.0952880641309304,0.0172295353356017,
-0.927565209628919));
#40213=CARTESIAN_POINT('Ctrl Pts',(-0.089595914035079,0.048710010740837,
-0.929681506410467));
#40214=CARTESIAN_POINT('Ctrl Pts',(-0.0667614237514503,0.0770908895838589,
-0.931797803192016));
#40215=CARTESIAN_POINT('Ctrl Pts',(-0.0372293640561305,0.0893904161847099,
-0.933914099973564));
#40216=CARTESIAN_POINT('Ctrl Pts',(-0.00769730436081029,0.101689942785561,
-0.936030396755112));
#40217=CARTESIAN_POINT('Ctrl Pts',(0.0285323247462011,0.0979081171442405,
-0.93814669353666));
#40218=CARTESIAN_POINT('Ctrl Pts',(0.0548876547176703,0.0797747918411131,
-0.940262990318209));
#40219=CARTESIAN_POINT('Ctrl Pts',(0.0812429846891394,0.0616414665379859,
-0.942379287099758));
#40220=CARTESIAN_POINT('Ctrl Pts',(0.0977240155250663,0.0291566415730521,
-0.944495583881307));
#40221=CARTESIAN_POINT('Ctrl Pts',(0.0967921252944012,-0.00282073300728408,
-0.946611880662855));
#40222=CARTESIAN_POINT('Ctrl Pts',(0.0958602350637361,-0.0347981075876205,
-0.948728177444403));
#40223=CARTESIAN_POINT('Ctrl Pts',(0.0775154237664787,-0.0662680317833592,
-0.950844474225951));
#40224=CARTESIAN_POINT('Ctrl Pts',(0.0501488289561232,-0.0828357833790652,
-0.9529607710075));
#40225=CARTESIAN_POINT('Ctrl Pts',(0.0227822341457677,-0.0994035349747711,
-0.955077067789048));
#40226=CARTESIAN_POINT('Ctrl Pts',(-0.0136061441776863,-0.101069113970444,
-0.957193364570597));
#40227=CARTESIAN_POINT('Ctrl Pts',(-0.0423718236643878,-0.0870706644803458,
-0.959309661352146));
#40228=CARTESIAN_POINT('Ctrl Pts',(-0.071137503151089,-0.0730722149902475,
-0.961425958133694));
#40229=CARTESIAN_POINT('Ctrl Pts',(-0.0922804838010382,-0.0434097370143778,
-0.963542254915242));
#40230=CARTESIAN_POINT('Ctrl Pts',(-0.0961297117092678,-0.0116512051062275,
-0.96565855169679));
#40231=CARTESIAN_POINT('Ctrl Pts',(-0.0965952505591475,-0.00781021912907144,
-0.965914503901537));
#40232=CARTESIAN_POINT('Ctrl Pts',(-0.0968078282443584,-0.00393857351130197,
-0.966170456106285));
#40233=CARTESIAN_POINT('Ctrl Pts',(-0.0967783240400222,-6.36632972197126E-5,
-0.966426408311032));
#40234=CARTESIAN_POINT('Ctrl Pts',(-0.0967903835966408,-5.70231646415709E-5,
-0.972223591688967));
#40235=CARTESIAN_POINT('Ctrl Pts',(-0.096813946806011,-0.00342450013328669,
-0.972001084575956));
#40236=CARTESIAN_POINT('Ctrl Pts',(-0.0966534270383089,-0.00678970548966747,
-0.971778577462944));
#40237=CARTESIAN_POINT('Ctrl Pts',(-0.0963013940171612,-0.0101347559966597,
-0.971556070349933));
#40238=CARTESIAN_POINT('Ctrl Pts',(-0.09295315791104,-0.0419500068722704,
-0.969439773568385));
#40239=CARTESIAN_POINT('Ctrl Pts',(-0.0722802833819321,-0.0719420132891045,
-0.967323476786836));
#40240=CARTESIAN_POINT('Ctrl Pts',(-0.043738792138609,-0.0863920704160863,
-0.965207180005287));
#40241=CARTESIAN_POINT('Ctrl Pts',(-0.0151973008952858,-0.100842127543068,
-0.963090883223739));
#40242=CARTESIAN_POINT('Ctrl Pts',(0.0212128070622524,-0.0997502353801977,
-0.960974586442191));
#40243=CARTESIAN_POINT('Ctrl Pts',(0.0488371099897059,-0.0836158385495418,
-0.958858289660643));
#40244=CARTESIAN_POINT('Ctrl Pts',(0.0764614129171591,-0.0674814417188861,
-0.956741992879094));
#40245=CARTESIAN_POINT('Ctrl Pts',(0.0952999108145277,-0.036304540220445,
-0.954625696097545));
#40246=CARTESIAN_POINT('Ctrl Pts',(0.0967356479326414,-0.00434582415965373,
-0.952509399315997));
#40247=CARTESIAN_POINT('Ctrl Pts',(0.0981713850507552,0.0276128919011376,
-0.950393102534449));
#40248=CARTESIAN_POINT('Ctrl Pts',(0.0822043613896141,0.0603534225242792,
-0.9482768057529));
#40249=CARTESIAN_POINT('Ctrl Pts',(0.0561380858105309,0.0788998548164988,
-0.946160508971352));
#40250=CARTESIAN_POINT('Ctrl Pts',(0.0300718102314475,0.0974462871087184,
-0.944044212189803));
#40251=CARTESIAN_POINT('Ctrl Pts',(-0.00609371726557807,0.101798621070016,
-0.941927915408255));
#40252=CARTESIAN_POINT('Ctrl Pts',(-0.0358159489817476,0.0899660467458193,
-0.939811618626706));
#40253=CARTESIAN_POINT('Ctrl Pts',(-0.0655381806979173,0.0781334724216229,
-0.937695321845158));
#40254=CARTESIAN_POINT('Ctrl Pts',(-0.0888171166332309,0.0501159898119325,
-0.93557902506361));
#40255=CARTESIAN_POINT('Ctrl Pts',(-0.0950046912193912,0.0187291327843489,
-0.933462728282061));
#40256=CARTESIAN_POINT('Ctrl Pts',(-0.096212343214622,0.0126032429085056,
-0.93304968275103));
#40257=CARTESIAN_POINT('Ctrl Pts',(-0.0967689376763235,0.00634900418126095,
-0.932636637219998));
#40258=CARTESIAN_POINT('Ctrl Pts',(-0.09671155539721,8.46130275593083E-5,
-0.932223591688967));
#40259=CARTESIAN_POINT('Origin',(0.,0.,-0.593));
#40260=CARTESIAN_POINT('',(-0.0965175797178924,1.07195340507057E-5,-0.886426408311032));
#40261=CARTESIAN_POINT('',(-0.0965165233765785,2.38684902196363E-6,-0.892223591688966));
#40262=CARTESIAN_POINT('',(-0.096675,-1.1839272930757E-17,-0.593));
#40263=CARTESIAN_POINT('Ctrl Pts',(-0.0965175797178924,1.07195340507057E-5,
-0.886426408311032));
#40264=CARTESIAN_POINT('Ctrl Pts',(-0.0965329025079771,0.015485362273297,
-0.88744156139437));
#40265=CARTESIAN_POINT('Ctrl Pts',(-0.0930271006338032,0.0309534509611169,
-0.888456714477709));
#40266=CARTESIAN_POINT('Ctrl Pts',(-0.085962915872296,0.0445763294634369,
-0.889471867561047));
#40267=CARTESIAN_POINT('Ctrl Pts',(-0.0712361601539585,0.0729760402096004,
-0.891588164342595));
#40268=CARTESIAN_POINT('Ctrl Pts',(-0.0410446601273461,0.0933564611217898,
-0.893704461124144));
#40269=CARTESIAN_POINT('Ctrl Pts',(-0.00919837140112475,0.0963953423006903,
-0.895820757905692));
#40270=CARTESIAN_POINT('Ctrl Pts',(0.0226479173250966,0.0994342234795908,
-0.897937054687241));
#40271=CARTESIAN_POINT('Ctrl Pts',(0.0561489947509267,0.0851315649252025,
-0.900053351468789));
#40272=CARTESIAN_POINT('Ctrl Pts',(0.0759810647189922,0.0600295748599686,
-0.902169648250338));
#40273=CARTESIAN_POINT('Ctrl Pts',(0.0958131346870579,0.0349275847947343,
-0.904285945031886));
#40274=CARTESIAN_POINT('Ctrl Pts',(0.101976197197358,-0.000973736781346012,
-0.906402241813434));
#40275=CARTESIAN_POINT('Ctrl Pts',(0.091651193256279,-0.0312526931383618,
-0.908518538594983));
#40276=CARTESIAN_POINT('Ctrl Pts',(0.0813261893151997,-0.0615316494953771,
-0.910634835376531));
#40277=CARTESIAN_POINT('Ctrl Pts',(0.054513118922741,-0.086188240633328,
-0.912751132158081));
#40278=CARTESIAN_POINT('Ctrl Pts',(0.0234766032976432,-0.0939442449078458,
-0.914867428939629));
#40279=CARTESIAN_POINT('Ctrl Pts',(-0.00755991232745468,-0.101700249182364,
-0.916983725721177));
#40280=CARTESIAN_POINT('Ctrl Pts',(-0.0428198731851916,-0.0925556665934481,
-0.919100022502725));
#40281=CARTESIAN_POINT('Ctrl Pts',(-0.0661749486600234,-0.070693339315266,
-0.921216319284273));
#40282=CARTESIAN_POINT('Ctrl Pts',(-0.0853408210952234,-0.0527524606312398,
-0.922953015626526));
#40283=CARTESIAN_POINT('Ctrl Pts',(-0.0964895463830737,-0.0262470282134427,
-0.924689711968779));
#40284=CARTESIAN_POINT('Ctrl Pts',(-0.0967266999094946,8.16697450527169E-5,
-0.926426408311032));
#40285=CARTESIAN_POINT('Ctrl Pts',(-0.09671155539721,8.46130275593083E-5,
-0.932223591688967));
#40286=CARTESIAN_POINT('Ctrl Pts',(-0.0964749315111858,-0.0257474835929374,
-0.93052034043845));
#40287=CARTESIAN_POINT('Ctrl Pts',(-0.0857979951590669,-0.0517522162392853,
-0.928817089187933));
#40288=CARTESIAN_POINT('Ctrl Pts',(-0.0672808542741755,-0.0696416428344169,
-0.927113837937416));
#40289=CARTESIAN_POINT('Ctrl Pts',(-0.0442732295057914,-0.0918693299801235,
-0.924997541155867));
#40290=CARTESIAN_POINT('Ctrl Pts',(-0.00916176673201553,-0.10156847282606,
-0.92288124437432));
#40291=CARTESIAN_POINT('Ctrl Pts',(0.0219931282431221,-0.094302566659775,
-0.920764947592771));
#40292=CARTESIAN_POINT('Ctrl Pts',(0.0531480232182593,-0.0870366604934904,
-0.918648650811222));
#40293=CARTESIAN_POINT('Ctrl Pts',(0.0803463503947581,-0.0628057053149853,
-0.916532354029673));
#40294=CARTESIAN_POINT('Ctrl Pts',(0.0911472674624636,-0.0326932317562424,
-0.914416057248125));
#40295=CARTESIAN_POINT('Ctrl Pts',(0.101948184530169,-0.0025807581974989,
-0.912299760466577));
#40296=CARTESIAN_POINT('Ctrl Pts',(0.0963516914890807,0.0334132337414824,
-0.910183463685029));
#40297=CARTESIAN_POINT('Ctrl Pts',(0.0769176916362815,0.0588246587910732,
-0.90806716690348));
#40298=CARTESIAN_POINT('Ctrl Pts',(0.0574836917834826,0.0842360838406634,
-0.905950870121932));
#40299=CARTESIAN_POINT('Ctrl Pts',(0.0242121851189731,0.0990649420008637,
-0.903834573340383));
#40300=CARTESIAN_POINT('Ctrl Pts',(-0.00767804063006863,0.0965283350142507,
-0.901718276558835));
#40301=CARTESIAN_POINT('Ctrl Pts',(-0.0395682663791108,0.0939917280276376,
-0.899601979777287));
#40302=CARTESIAN_POINT('Ctrl Pts',(-0.0700772112126856,0.0740896558942112,
-0.897485682995738));
#40303=CARTESIAN_POINT('Ctrl Pts',(-0.0852497164454802,0.0459255660227048,
-0.89536938621419));
#40304=CARTESIAN_POINT('Ctrl Pts',(-0.0927675000744725,0.0319706172180849,
-0.894320788039116));
#40305=CARTESIAN_POINT('Ctrl Pts',(-0.0965200702590053,0.0159872797472848,
-0.893272189864041));
#40306=CARTESIAN_POINT('Ctrl Pts',(-0.0965165486863883,2.38646782571199E-6,
-0.892223591688966));
#40307=CARTESIAN_POINT('Origin',(0.,0.,-0.593));
#40308=CARTESIAN_POINT('',(-0.0966873976231268,-8.74994151896375E-5,-0.846426408311032));
#40309=CARTESIAN_POINT('',(-0.0967028036390754,-8.59090990596172E-5,-0.852223591688967));
#40310=CARTESIAN_POINT('',(-0.096675,-1.1839272930757E-17,-0.593));
#40311=CARTESIAN_POINT('Ctrl Pts',(-0.0966873976231268,-8.74994151896374E-5,
-0.846426408311032));
#40312=CARTESIAN_POINT('Ctrl Pts',(-0.0964563468117902,0.0249637526176381,
-0.848077114038413));
#40313=CARTESIAN_POINT('Ctrl Pts',(-0.0864956095149754,0.0501779485389757,
-0.849727819765794));
#40314=CARTESIAN_POINT('Ctrl Pts',(-0.0689844853064945,0.067954490953125,
-0.851378525493176));
#40315=CARTESIAN_POINT('Ctrl Pts',(-0.0465342476966098,0.0907450095017034,
-0.853494822274724));
#40316=CARTESIAN_POINT('Ctrl Pts',(-0.0116736885465889,0.101310502682944,
-0.855611119056273));
#40317=CARTESIAN_POINT('Ctrl Pts',(0.0196515526778018,0.094818186710419,
-0.857727415837821));
#40318=CARTESIAN_POINT('Ctrl Pts',(0.0509767939021918,0.0883258707378936,
-0.859843712619369));
#40319=CARTESIAN_POINT('Ctrl Pts',(0.0787667172009514,0.064775745611602,
-0.861960009400918));
#40320=CARTESIAN_POINT('Ctrl Pts',(0.0903098770749894,0.0349399221006658,
-0.864076306182466));
#40321=CARTESIAN_POINT('Ctrl Pts',(0.101853036949027,0.00510409858972969,
-0.866192602964014));
#40322=CARTESIAN_POINT('Ctrl Pts',(0.097149433398344,-0.0310174233058513,
-0.868308899745563));
#40323=CARTESIAN_POINT('Ctrl Pts',(0.0783505513169802,-0.0569022245788824,
-0.870425196527111));
#40324=CARTESIAN_POINT('Ctrl Pts',(0.0595516692356162,-0.0827870258519136,
-0.87254149330866));
#40325=CARTESIAN_POINT('Ctrl Pts',(0.0266575086235715,-0.098435106502395,
-0.874657790090208));
#40326=CARTESIAN_POINT('Ctrl Pts',(-0.00528574541949839,-0.0966888460426565,
-0.876774086871757));
#40327=CARTESIAN_POINT('Ctrl Pts',(-0.0372289994625683,-0.0949425855829181,
-0.878890383653305));
#40328=CARTESIAN_POINT('Ctrl Pts',(-0.068221346936663,-0.0758019840129603,
-0.881006680434853));
#40329=CARTESIAN_POINT('Ctrl Pts',(-0.0840865149686794,-0.0480221829379125,
-0.883122977216402));
#40330=CARTESIAN_POINT('Ctrl Pts',(-0.0923414204015161,-0.033567899796709,
-0.884224120914612));
#40331=CARTESIAN_POINT('Ctrl Pts',(-0.0965009589795843,-0.0167747344177196,
-0.885325264612822));
#40332=CARTESIAN_POINT('Ctrl Pts',(-0.0965175797178924,1.07195340507057E-5,
-0.886426408311032));
#40333=CARTESIAN_POINT('Ctrl Pts',(-0.0965165486863883,2.38646782571199E-6,
-0.892223591688966));
#40334=CARTESIAN_POINT('Ctrl Pts',(-0.0965129629676018,-0.0162736749299603,
-0.891155893082492));
#40335=CARTESIAN_POINT('Ctrl Pts',(-0.0926152032764517,-0.0325513493313622,
-0.890088194476018));
#40336=CARTESIAN_POINT('Ctrl Pts',(-0.0848328988951623,-0.0466910166261522,
-0.889020495869544));
#40337=CARTESIAN_POINT('Ctrl Pts',(-0.0694075104800352,-0.0747174017939175,
-0.886904199087995));
#40338=CARTESIAN_POINT('Ctrl Pts',(-0.0387206680177668,-0.0943440645198617,
-0.884787902306448));
#40339=CARTESIAN_POINT('Ctrl Pts',(-0.00680890271086272,-0.096593532974079,
-0.882671605524899));
#40340=CARTESIAN_POINT('Ctrl Pts',(0.0251028625960414,-0.0988430014282963,
-0.880555308743351));
#40341=CARTESIAN_POINT('Ctrl Pts',(0.0582395507475817,-0.0837152756107857,
-0.878439011961802));
#40342=CARTESIAN_POINT('Ctrl Pts',(0.0774440416275778,-0.0581299594437026,
-0.876322715180254));
#40343=CARTESIAN_POINT('Ctrl Pts',(0.096648532507574,-0.0325446432766194,
-0.874206418398705));
#40344=CARTESIAN_POINT('Ctrl Pts',(0.101920826116027,0.00349826324003634,
-0.872090121617157));
#40345=CARTESIAN_POINT('Ctrl Pts',(0.090849311879616,0.0335123007198961,
-0.869973824835609));
#40346=CARTESIAN_POINT('Ctrl Pts',(0.0797777976432054,0.0635263381997554,
-0.86785752805406));
#40347=CARTESIAN_POINT('Ctrl Pts',(0.0523624755619313,0.0875115066428186,
-0.865741231272511));
#40348=CARTESIAN_POINT('Ctrl Pts',(0.0211434440279221,0.0944967012290832,
-0.863624934490963));
#40349=CARTESIAN_POINT('Ctrl Pts',(-0.0100755875060871,0.101481895815348,
-0.861508637709414));
#40350=CARTESIAN_POINT('Ctrl Pts',(-0.0450983284928317,0.0914671165448139,
-0.859392340927867));
#40351=CARTESIAN_POINT('Ctrl Pts',(-0.0679049555418073,0.0690332440307253,
-0.857276044146318));
#40352=CARTESIAN_POINT('Ctrl Pts',(-0.0860544891803395,0.0511803487752086,
-0.855591893327202));
#40353=CARTESIAN_POINT('Ctrl Pts',(-0.096467569784056,0.0254624538886146,
-0.853907742508084));
#40354=CARTESIAN_POINT('Ctrl Pts',(-0.0967028036390754,-8.59090990596172E-5,
-0.852223591688967));
#40355=CARTESIAN_POINT('Origin',(0.,0.,-0.593));
#40356=CARTESIAN_POINT('',(-0.0968069805588836,4.52912843358962E-5,-0.806426408311032));
#40357=CARTESIAN_POINT('',(-0.0967967750279647,5.29324940476346E-5,-0.812223591688966));
#40358=CARTESIAN_POINT('',(-0.096675,-1.1839272930757E-17,-0.593));
#40359=CARTESIAN_POINT('Ctrl Pts',(-0.0968069805588836,4.52912843358962E-5,
-0.806426408311032));
#40360=CARTESIAN_POINT('Ctrl Pts',(-0.096821913186225,0.0026163686460789,
-0.806596369900907));
#40361=CARTESIAN_POINT('Ctrl Pts',(-0.0967283557208207,0.00518634230609915,
-0.806766331490783));
#40362=CARTESIAN_POINT('Ctrl Pts',(-0.096522800338362,0.00774732654152389,
-0.806936293080658));
#40363=CARTESIAN_POINT('Ctrl Pts',(-0.0939633032505456,0.0396357237905355,
-0.809052589862207));
#40364=CARTESIAN_POINT('Ctrl Pts',(-0.0740393367051216,0.0701303755759174,
-0.811168886643756));
#40365=CARTESIAN_POINT('Ctrl Pts',(-0.0458643628784741,0.0852826610246885,
-0.813285183425304));
#40366=CARTESIAN_POINT('Ctrl Pts',(-0.017689389051826,0.10043494647346,
-0.815401480206853));
#40367=CARTESIAN_POINT('Ctrl Pts',(0.0187365920560463,0.10024486558562,
-0.817517776988401));
#40368=CARTESIAN_POINT('Ctrl Pts',(0.0467518981286488,0.0847993636477818,
-0.819634073769949));
#40369=CARTESIAN_POINT('Ctrl Pts',(0.0747672042012515,0.0693538617099438,
-0.821750370551497));
#40370=CARTESIAN_POINT('Ctrl Pts',(0.0943718352385847,0.0386529387221085,
-0.823866667333046));
#40371=CARTESIAN_POINT('Ctrl Pts',(0.0965983969703672,0.00673956648870246,
-0.825982964114595));
#40372=CARTESIAN_POINT('Ctrl Pts',(0.0988249587021496,-0.0251738057447027,
-0.828099260896143));
#40373=CARTESIAN_POINT('Ctrl Pts',(0.0836734511283823,-0.0582996272236781,
-0.830215557677691));
#40374=CARTESIAN_POINT('Ctrl Pts',(0.0580743562328568,-0.0774857483789087,
-0.832331854459239));
#40375=CARTESIAN_POINT('Ctrl Pts',(0.0324752613373307,-0.0966718695341397,
-0.834448151240788));
#40376=CARTESIAN_POINT('Ctrl Pts',(-0.00357142087995465,-0.101918290365625,
-0.836564448022337));
#40377=CARTESIAN_POINT('Ctrl Pts',(-0.033577503981703,-0.0908252348197296,
-0.838680744803886));
#40378=CARTESIAN_POINT('Ctrl Pts',(-0.0635835870834512,-0.0797321792738341,
-0.840797041585434));
#40379=CARTESIAN_POINT('Ctrl Pts',(-0.0875490710696629,-0.0522996473505582,
-0.842913338366981));
#40380=CARTESIAN_POINT('Ctrl Pts',(-0.0945118550278948,-0.0210756094309628,
-0.84502963514853));
#40381=CARTESIAN_POINT('Ctrl Pts',(-0.0960436864568877,-0.0142062360722284,
-0.845495226202697));
#40382=CARTESIAN_POINT('Ctrl Pts',(-0.0967525668347142,-0.00715334928091926,
-0.845960817256864));
#40383=CARTESIAN_POINT('Ctrl Pts',(-0.0966873976231268,-8.74994151896374E-5,
-0.846426408311032));
#40384=CARTESIAN_POINT('Ctrl Pts',(-0.0967028036390754,-8.59090990596172E-5,
-0.852223591688967));
#40385=CARTESIAN_POINT('Ctrl Pts',(-0.0967631636493072,-0.00664151076283559,
-0.851791445726535));
#40386=CARTESIAN_POINT('Ctrl Pts',(-0.0961534001335114,-0.0131859502115887,
-0.851359299764104));
#40387=CARTESIAN_POINT('Ctrl Pts',(-0.094832266671799,-0.0195834870855345,
-0.850927153801673));
#40388=CARTESIAN_POINT('Ctrl Pts',(-0.0883624376416084,-0.0509133799300614,
-0.848810857020124));
#40389=CARTESIAN_POINT('Ctrl Pts',(-0.0648322664700212,-0.0787201998614719,
-0.846694560238576));
#40390=CARTESIAN_POINT('Ctrl Pts',(-0.0350047367470373,-0.0902847726574704,
-0.844578263457028));
#40391=CARTESIAN_POINT('Ctrl Pts',(-0.00517720702405281,-0.101849345453469,
-0.842461966675479));
#40392=CARTESIAN_POINT('Ctrl Pts',(0.0309476812503285,-0.0971716711140548,
-0.84034566989393));
#40393=CARTESIAN_POINT('Ctrl Pts',(0.0568459692467185,-0.0783913741998545,
-0.838229373112382));
#40394=CARTESIAN_POINT('Ctrl Pts',(0.082744257243108,-0.0596110772856547,
-0.836113076330834));
#40395=CARTESIAN_POINT('Ctrl Pts',(0.0984159449615066,-0.0267281577966689,
-0.833996779549286));
#40396=CARTESIAN_POINT('Ctrl Pts',(0.0966926137571569,0.00521634099247394,
-0.831880482767737));
#40397=CARTESIAN_POINT('Ctrl Pts',(0.0949692825528072,0.0371608397816173,
-0.829764185986189));
#40398=CARTESIAN_POINT('Ctrl Pts',(0.0758509324257091,0.0681669178709179,
-0.82764788920464));
#40399=CARTESIAN_POINT('Ctrl Pts',(0.0480825269031277,0.0840520218385643,
-0.825531592423091));
#40400=CARTESIAN_POINT('Ctrl Pts',(0.0203141213805463,0.0999371258062107,
-0.823415295641543));
#40401=CARTESIAN_POINT('Ctrl Pts',(-0.0161043395375181,0.100701255652203,
-0.821298998859995));
#40402=CARTESIAN_POINT('Ctrl Pts',(-0.0445146133599316,0.0859948891850922,
-0.819182702078447));
#40403=CARTESIAN_POINT('Ctrl Pts',(-0.0729248871823449,0.0712885227179818,
-0.817066405296898));
#40404=CARTESIAN_POINT('Ctrl Pts',(-0.0933269739091071,0.0411116599377694,
-0.814950108515349));
#40405=CARTESIAN_POINT('Ctrl Pts',(-0.096388713436468,0.00926756120038876,
-0.812833811733801));
#40406=CARTESIAN_POINT('Ctrl Pts',(-0.0966829908188508,0.00620688345917894,
-0.812630405052189));
#40407=CARTESIAN_POINT('Ctrl Pts',(-0.0968170783214265,0.00313080381600502,
-0.812426998370578));
#40408=CARTESIAN_POINT('Ctrl Pts',(-0.0967967750279647,5.29324940476346E-5,
-0.812223591688966));
#40409=CARTESIAN_POINT('Origin',(0.,0.,-0.593));
#40410=CARTESIAN_POINT('',(-0.0965527474869059,5.80210454589614E-5,-0.766426408311032));
#40411=CARTESIAN_POINT('',(-0.0965440014864236,5.14221950347461E-5,-0.772223591688967));
#40412=CARTESIAN_POINT('',(-0.096675,-1.1839272930757E-17,-0.593));
#40413=CARTESIAN_POINT('Ctrl Pts',(-0.0965527474869059,5.80210454589614E-5,
-0.766426408311032));
#40414=CARTESIAN_POINT('Ctrl Pts',(-0.0966199713755426,0.0123258193606181,
-0.76723192254495));
#40415=CARTESIAN_POINT('Ctrl Pts',(-0.0944522024343605,0.0245707460210818,
-0.768037436778869));
#40416=CARTESIAN_POINT('Ctrl Pts',(-0.0899403163476919,0.0358805176798972,
-0.768842951012787));
#40417=CARTESIAN_POINT('Ctrl Pts',(-0.0780864103558861,0.065594248801902,
-0.770959247794335));
#40418=CARTESIAN_POINT('Ctrl Pts',(-0.0500522249818788,0.0888530682223019,
-0.773075544575884));
#40419=CARTESIAN_POINT('Ctrl Pts',(-0.0186609341388208,0.0950181119090823,
-0.775191841357432));
#40420=CARTESIAN_POINT('Ctrl Pts',(0.0127303567042363,0.101183155595862,
-0.777308138138981));
#40421=CARTESIAN_POINT('Ctrl Pts',(0.0474787530163437,0.0902544235490242,
-0.779424434920529));
#40422=CARTESIAN_POINT('Ctrl Pts',(0.0696899199642036,0.0672308493854064,
-0.781540731702077));
#40423=CARTESIAN_POINT('Ctrl Pts',(0.0919010869120639,0.0442072752217881,
-0.783657028483626));
#40424=CARTESIAN_POINT('Ctrl Pts',(0.101575024495676,0.00908885894138933,
-0.785773325265174));
#40425=CARTESIAN_POINT('Ctrl Pts',(0.0942867571930242,-0.0220608130340657,
-0.787889622046723));
#40426=CARTESIAN_POINT('Ctrl Pts',(0.0869984898903725,-0.0532104850095206,
-0.790005918828271));
#40427=CARTESIAN_POINT('Ctrl Pts',(0.0627480177014573,-0.0803914126800321,
-0.792122215609819));
#40428=CARTESIAN_POINT('Ctrl Pts',(0.0326277985738104,-0.0911707124789926,
-0.794238512391368));
#40429=CARTESIAN_POINT('Ctrl Pts',(0.00250757944616346,-0.101950012277953,
-0.796354809172916));
#40430=CARTESIAN_POINT('Ctrl Pts',(-0.0334823866202151,-0.0963276842053627,
-0.798471105954465));
#40431=CARTESIAN_POINT('Ctrl Pts',(-0.0588798558383005,-0.0768754488127468,
-0.800587402736014));
#40432=CARTESIAN_POINT('Ctrl Pts',(-0.0822376327576704,-0.0589854389467146,
-0.802533737927686));
#40433=CARTESIAN_POINT('Ctrl Pts',(-0.0966359778157342,-0.0293977043556654,
-0.804480073119359));
#40434=CARTESIAN_POINT('Ctrl Pts',(-0.0968069805588836,4.52912843358962E-5,
-0.806426408311032));
#40435=CARTESIAN_POINT('Ctrl Pts',(-0.0967967750279647,5.29324940476346E-5,
-0.812223591688966));
#40436=CARTESIAN_POINT('Ctrl Pts',(-0.0966058374995047,-0.0288921814717637,
-0.810310701589029));
#40437=CARTESIAN_POINT('Ctrl Pts',(-0.0827605504412421,-0.0579957518286451,
-0.808397811489093));
#40438=CARTESIAN_POINT('Ctrl Pts',(-0.0600840974796387,-0.0759379549276761,
-0.806484921389156));
#40439=CARTESIAN_POINT('Ctrl Pts',(-0.0349963496674887,-0.0957880376238121,
-0.804368624607608));
#40440=CARTESIAN_POINT('Ctrl Pts',(0.000900538284770831,-0.101976868321535,
-0.802252327826059));
#40441=CARTESIAN_POINT('Ctrl Pts',(0.0311868976401448,-0.0916736013480633,
-0.800136031044511));
#40442=CARTESIAN_POINT('Ctrl Pts',(0.0614732569955178,-0.0813703343745921,
-0.798019734262962));
#40443=CARTESIAN_POINT('Ctrl Pts',(0.0861490877540057,-0.0545749697299277,
-0.795903437481414));
#40444=CARTESIAN_POINT('Ctrl Pts',(0.0939273678371664,-0.0235440298105936,
-0.793787140699865));
#40445=CARTESIAN_POINT('Ctrl Pts',(0.101705647920327,0.00748691010874134,
-0.791670843918317));
#40446=CARTESIAN_POINT('Ctrl Pts',(0.0925863773281602,0.0427534253027464,
-0.789554547136769));
#40447=CARTESIAN_POINT('Ctrl Pts',(0.0707408202227712,0.0661241871235485,
-0.78743825035522));
#40448=CARTESIAN_POINT('Ctrl Pts',(0.0488952631173822,0.0894949489443506,
-0.785321953573672));
#40449=CARTESIAN_POINT('Ctrl Pts',(0.0143234194987715,0.10096995739195,
-0.783205656792123));
#40450=CARTESIAN_POINT('Ctrl Pts',(-0.0171611331274083,0.0953004054467968,
-0.781089360010575));
#40451=CARTESIAN_POINT('Ctrl Pts',(-0.0486456857535873,0.0896308535016439,
-0.778973063229026));
#40452=CARTESIAN_POINT('Ctrl Pts',(-0.0770429473873355,0.0668167411637396,
-0.776856766447478));
#40453=CARTESIAN_POINT('Ctrl Pts',(-0.0893636686629692,0.0372935180914264,
-0.77474046966593));
#40454=CARTESIAN_POINT('Ctrl Pts',(-0.0942479477031789,0.0255896854646212,
-0.773901510340276));
#40455=CARTESIAN_POINT('Ctrl Pts',(-0.0966057153328721,0.0128314814091803,
-0.773062551014621));
#40456=CARTESIAN_POINT('Ctrl Pts',(-0.0965440014864236,5.14221950347461E-5,
-0.772223591688967));
#40457=CARTESIAN_POINT('Origin',(0.,0.,-0.593));
#40458=CARTESIAN_POINT('',(-0.0965963020766926,-7.83064175312459E-5,-0.726426408311032));
#40459=CARTESIAN_POINT('',(-0.0966095321632848,-8.1873982564944E-5,-0.732223591688966));
#40460=CARTESIAN_POINT('',(-0.096675,-1.1839272930757E-17,-0.593));
#40461=CARTESIAN_POINT('Ctrl Pts',(-0.0965963020766926,-7.83064175312459E-5,
-0.726426408311032));
#40462=CARTESIAN_POINT('Ctrl Pts',(-0.0964291685623488,0.0218439313421801,
-0.727867475188993));
#40463=CARTESIAN_POINT('Ctrl Pts',(-0.0890325024660615,0.0438682325777133,
-0.729308542066955));
#40464=CARTESIAN_POINT('Ctrl Pts',(-0.0753504419047513,0.0608192646984407,
-0.730749608944916));
#40465=CARTESIAN_POINT('Ctrl Pts',(-0.0552574807981732,0.0857129148611408,
-0.732865905726464));
#40466=CARTESIAN_POINT('Ctrl Pts',(-0.0216089613936002,0.0996651681664339,
-0.734982202508012));
#40467=CARTESIAN_POINT('Ctrl Pts',(0.0102038784153586,0.0962940959715852,
-0.737098499289561));
#40468=CARTESIAN_POINT('Ctrl Pts',(0.0420167182243175,0.0929230237767366,
-0.739214796071109));
#40469=CARTESIAN_POINT('Ctrl Pts',(0.0719938784376625,0.0722286260817463,
-0.741331092852657));
#40470=CARTESIAN_POINT('Ctrl Pts',(0.0864234450579025,0.0436767695465677,
-0.743447389634206));
#40471=CARTESIAN_POINT('Ctrl Pts',(0.100853011678142,0.0151249130113896,
-0.745563686415754));
#40472=CARTESIAN_POINT('Ctrl Pts',(0.0997349847052779,-0.0212844023639766,
-0.747679983197303));
#40473=CARTESIAN_POINT('Ctrl Pts',(0.0835807631374022,-0.0488971173697365,
-0.749796279978852));
#40474=CARTESIAN_POINT('Ctrl Pts',(0.0674265415695264,-0.0765098323754965,
-0.7519125767604));
#40475=CARTESIAN_POINT('Ctrl Pts',(0.03623612540664,-0.09532594701165,-0.754028873541948));
#40476=CARTESIAN_POINT('Ctrl Pts',(0.00427638652478659,-0.0967387439033137,
-0.756145170323496));
#40477=CARTESIAN_POINT('Ctrl Pts',(-0.0276833523570661,-0.0981515407949775,
-0.758261467105044));
#40478=CARTESIAN_POINT('Ctrl Pts',(-0.0604124139578854,-0.0821610199421518,
-0.760377763886594));
#40479=CARTESIAN_POINT('Ctrl Pts',(-0.0789401314534932,-0.0560814381039349,
-0.762494060668142));
#40480=CARTESIAN_POINT('Ctrl Pts',(-0.0904157472330977,-0.0399283819630976,
-0.763804843215772));
#40481=CARTESIAN_POINT('Ctrl Pts',(-0.0964433566204278,-0.0199048986054247,
-0.765115625763402));
#40482=CARTESIAN_POINT('Ctrl Pts',(-0.0965527474869059,5.80210454589614E-5,
-0.766426408311032));
#40483=CARTESIAN_POINT('Ctrl Pts',(-0.0965440014864236,5.14221950347461E-5,
-0.772223591688967));
#40484=CARTESIAN_POINT('Ctrl Pts',(-0.0964500405455227,-0.0194065513009297,
-0.770946254233073));
#40485=CARTESIAN_POINT('Ctrl Pts',(-0.0907475142576013,-0.0389151869271784,
-0.769668916777178));
#40486=CARTESIAN_POINT('Ctrl Pts',(-0.0798141682827737,-0.0548303776192502,
-0.768391579321284));
#40487=CARTESIAN_POINT('Ctrl Pts',(-0.0616997657094256,-0.0811987164508894,
-0.766275282539736));
#40488=CARTESIAN_POINT('Ctrl Pts',(-0.0292267796452108,-0.097703060307445,
-0.764158985758187));
#40489=CARTESIAN_POINT('Ctrl Pts',(0.00275125511920654,-0.0967941236016399,
-0.762042688976639));
#40490=CARTESIAN_POINT('Ctrl Pts',(0.0347292898836239,-0.0958851868958348,
-0.759926392195091));
#40491=CARTESIAN_POINT('Ctrl Pts',(0.0662123733482439,-0.0775629696276689,
-0.757810095413542));
#40492=CARTESIAN_POINT('Ctrl Pts',(0.082799764089584,-0.050208274569534,
-0.755693798631993));
#40493=CARTESIAN_POINT('Ctrl Pts',(0.0993871548309243,-0.0228535795113987,
-0.753577501850445));
#40494=CARTESIAN_POINT('Ctrl Pts',(0.101078852848984,0.0135335933367059,
-0.751461205068897));
#40495=CARTESIAN_POINT('Ctrl Pts',(0.0871010551027728,0.0423093130235439,
-0.749344908287348));
#40496=CARTESIAN_POINT('Ctrl Pts',(0.0731232573565615,0.0710850327103816,
-0.7472286115058));
#40497=CARTESIAN_POINT('Ctrl Pts',(0.0434759638460791,0.0922492992359529,
-0.745112314724252));
#40498=CARTESIAN_POINT('Ctrl Pts',(0.0117202035674321,0.0961213222801188,
-0.742996017942703));
#40499=CARTESIAN_POINT('Ctrl Pts',(-0.020035556711215,0.0999933453242847,
-0.740879721161155));
#40500=CARTESIAN_POINT('Ctrl Pts',(-0.0538997837580266,0.0865731248870451,
-0.738763424379606));
#40501=CARTESIAN_POINT('Ctrl Pts',(-0.07438257240678,0.0619992313717728,
-0.736647127598058));
#40502=CARTESIAN_POINT('Ctrl Pts',(-0.0886537829943919,0.0448775779031986,
-0.735172615628361));
#40503=CARTESIAN_POINT('Ctrl Pts',(-0.0964289899211591,0.0223413868496905,
-0.733698103658664));
#40504=CARTESIAN_POINT('Ctrl Pts',(-0.0966095321632848,-8.1873982564944E-5,
-0.732223591688966));
#40505=CARTESIAN_POINT('Origin',(0.,0.,-0.593));
#40506=CARTESIAN_POINT('',(-0.0968316171384256,-1.1157892015598E-5,-0.686426408311032));
#40507=CARTESIAN_POINT('',(-0.09683317566692,-1.75825702407311E-6,-0.692223591688967));
#40508=CARTESIAN_POINT('',(-0.096675,-1.1839272930757E-17,-0.593));
#40509=CARTESIAN_POINT('Ctrl Pts',(-0.0968316171384256,-1.1157892015598E-5,
-0.686426408311032));
#40510=CARTESIAN_POINT('Ctrl Pts',(-0.0967803231635655,0.0313814111628826,
-0.688503027833036));
#40511=CARTESIAN_POINT('Ctrl Pts',(-0.080097610772753,0.0628207796501225,
-0.69057964735504));
#40512=CARTESIAN_POINT('Ctrl Pts',(-0.0540521141943119,0.0803432698166147,
-0.692656266877044));
#40513=CARTESIAN_POINT('Ctrl Pts',(-0.027508975213516,0.0982005562145947,
-0.694772563658592));
#40514=CARTESIAN_POINT('Ctrl Pts',(0.00875814900968967,0.101604073658873,
-0.696888860440141));
#40515=CARTESIAN_POINT('Ctrl Pts',(0.038160239210447,0.08899701229312,-0.699005157221689));
#40516=CARTESIAN_POINT('Ctrl Pts',(0.0675623294112047,0.0763899509273669,
-0.701121454003237));
#40517=CARTESIAN_POINT('Ctrl Pts',(0.0900993855895135,0.0477723107515832,
-0.703237750784786));
#40518=CARTESIAN_POINT('Ctrl Pts',(0.0954626869101027,0.0162341449298691,
-0.705354047566334));
#40519=CARTESIAN_POINT('Ctrl Pts',(0.100825988230692,-0.0153040208918445,
-0.707470344347883));
#40520=CARTESIAN_POINT('Ctrl Pts',(0.0890155346935609,-0.0497627123594873,
-0.709586641129431));
#40521=CARTESIAN_POINT('Ctrl Pts',(0.0654335699408682,-0.0713801091235773,
-0.71170293791098));
#40522=CARTESIAN_POINT('Ctrl Pts',(0.0418516051881752,-0.0929975058876676,
-0.713819234692528));
#40523=CARTESIAN_POINT('Ctrl Pts',(0.00649812921991958,-0.101773607948205,
-0.715935531474077));
#40524=CARTESIAN_POINT('Ctrl Pts',(-0.0244557524109016,-0.0936941205610948,
-0.718051828255625));
#40525=CARTESIAN_POINT('Ctrl Pts',(-0.055409634041722,-0.0856146331739852,
-0.720168125037174));
#40526=CARTESIAN_POINT('Ctrl Pts',(-0.0819639213351086,-0.0606795563392294,
-0.722284421818721));
#40527=CARTESIAN_POINT('Ctrl Pts',(-0.0919723635775106,-0.0302944944117986,
-0.72440071860027));
#40528=CARTESIAN_POINT('Ctrl Pts',(-0.0951656772702392,-0.0205997754977805,
-0.725075948503857));
#40529=CARTESIAN_POINT('Ctrl Pts',(-0.0966746145745388,-0.0103502450175289,
-0.725751178407445));
#40530=CARTESIAN_POINT('Ctrl Pts',(-0.0965963020766926,-7.83064175312459E-5,
-0.726426408311032));
#40531=CARTESIAN_POINT('Ctrl Pts',(-0.0966095321632848,-8.1873982564944E-5,
-0.732223591688966));
#40532=CARTESIAN_POINT('Ctrl Pts',(-0.096688113599906,-0.00984165113600456,
-0.731581806877115));
#40533=CARTESIAN_POINT('Ctrl Pts',(-0.0953279267075589,-0.0195800342671315,
-0.730940022065264));
#40534=CARTESIAN_POINT('Ctrl Pts',(-0.0924383800560967,-0.0288412492993127,
-0.730298237253412));
#40535=CARTESIAN_POINT('Ctrl Pts',(-0.0829100488059648,-0.0593802698618187,
-0.728181940471864));
#40536=CARTESIAN_POINT('Ctrl Pts',(-0.0567520360550064,-0.0847307443935267,
-0.726065643690316));
#40537=CARTESIAN_POINT('Ctrl Pts',(-0.0259293317700408,-0.0932970606316171,
-0.723949346908767));
#40538=CARTESIAN_POINT('Ctrl Pts',(0.00489337251492607,-0.101863376869708,
-0.721833050127219));
#40539=CARTESIAN_POINT('Ctrl Pts',(0.0403807683338999,-0.0936455348141805,
-0.71971675334567));
#40540=CARTESIAN_POINT('Ctrl Pts',(0.0643004935818126,-0.072402474361556,
-0.717600456564122));
#40541=CARTESIAN_POINT('Ctrl Pts',(0.088220218829725,-0.0511594139089317,
-0.715484159782573));
#40542=CARTESIAN_POINT('Ctrl Pts',(0.100572273506576,-0.0168911350592103,
-0.713367863001025));
#40543=CARTESIAN_POINT('Ctrl Pts',(0.0957066790881852,0.0147276388620725,
-0.711251566219477));
#40544=CARTESIAN_POINT('Ctrl Pts',(0.0908410846697948,0.0463464127833544,
-0.709135269437928));
#40545=CARTESIAN_POINT('Ctrl Pts',(0.0687578411561641,0.0753156817761985,
-0.70701897265638));
#40546=CARTESIAN_POINT('Ctrl Pts',(0.0395580900059744,0.0883845534220754,
-0.704902675874831));
#40547=CARTESIAN_POINT('Ctrl Pts',(0.0103583388557835,0.101453425067953,
-0.702786379093283));
#40548=CARTESIAN_POINT('Ctrl Pts',(-0.0259579199309663,0.0986218993668624,
-0.700670082311735));
#40549=CARTESIAN_POINT('Ctrl Pts',(-0.0527791923484877,0.0811851502651922,
-0.698553785530186));
#40550=CARTESIAN_POINT('Ctrl Pts',(-0.0795214802530595,0.063799749701868,
-0.696443720916446));
#40551=CARTESIAN_POINT('Ctrl Pts',(-0.0968246219893057,0.0318950193429899,
-0.694333656302706));
#40552=CARTESIAN_POINT('Ctrl Pts',(-0.09683317566692,-1.75825702407311E-6,
-0.692223591688967));
#40553=CARTESIAN_POINT('Origin',(0.,0.,-0.593));
#40554=CARTESIAN_POINT('',(-0.0966287398315909,8.55332849566889E-5,-0.646426408311032));
#40555=CARTESIAN_POINT('',(-0.0966146360987624,8.30122117530267E-5,-0.652223591688966));
#40556=CARTESIAN_POINT('',(-0.096675,-1.1839272930757E-17,-0.593));
#40557=CARTESIAN_POINT('Ctrl Pts',(-0.0966287398315909,8.55332849566889E-5,
-0.646426408311032));
#40558=CARTESIAN_POINT('Ctrl Pts',(-0.0967060986674926,0.00914259352035314,
-0.64702228369553));
#40559=CARTESIAN_POINT('Ctrl Pts',(-0.0955368666845756,0.0181800678202769,
-0.647618159080028));
#40560=CARTESIAN_POINT('Ctrl Pts',(-0.0930406615301446,0.0268348161114135,
-0.648214034464527));
#40561=CARTESIAN_POINT('Ctrl Pts',(-0.0841751989320309,0.0575728134010026,
-0.650330331246075));
#40562=CARTESIAN_POINT('Ctrl Pts',(-0.0585717042856102,0.0834832223577448,
-0.652446628027624));
#40563=CARTESIAN_POINT('Ctrl Pts',(-0.0279415243004564,0.0927143099713701,
-0.654562924809172));
#40564=CARTESIAN_POINT('Ctrl Pts',(0.00268865568469739,0.101945397584995,
-0.656679221590721));
#40565=CARTESIAN_POINT('Ctrl Pts',(0.0383455210085838,0.0944971638555036,
-0.658795518372269));
#40566=CARTESIAN_POINT('Ctrl Pts',(0.062719192174226,0.0737765205652367,
-0.660911815153817));
#40567=CARTESIAN_POINT('Ctrl Pts',(0.0870928633398687,0.0530558772749696,
-0.663028111935366));
#40568=CARTESIAN_POINT('Ctrl Pts',(0.100183340347266,0.0190628244239271,
-0.665144408716914));
#40569=CARTESIAN_POINT('Ctrl Pts',(0.0960028814078669,-0.0126538063477889,
-0.667260705498463));
#40570=CARTESIAN_POINT('Ctrl Pts',(0.0918224224684676,-0.0443704371195039,
-0.669377002280011));
#40571=CARTESIAN_POINT('Ctrl Pts',(0.0703710275822714,-0.0738106458118936,
-0.671493299061559));
#40572=CARTESIAN_POINT('Ctrl Pts',(0.0414608230385063,-0.0875081265178838,
-0.673609595843108));
#40573=CARTESIAN_POINT('Ctrl Pts',(0.0125506184947407,-0.101205607223874,
-0.675725892624656));
#40574=CARTESIAN_POINT('Ctrl Pts',(-0.0238183957065942,-0.099160359943466,
-0.677842189406205));
#40575=CARTESIAN_POINT('Ctrl Pts',(-0.0510105945979204,-0.082307905406874,
-0.679958486187754));
#40576=CARTESIAN_POINT('Ctrl Pts',(-0.0782027934892469,-0.0654554508702817,
-0.682074782969302));
#40577=CARTESIAN_POINT('Ctrl Pts',(-0.096218177070564,-0.0337957890775055,
-0.68419107975085));
#40578=CARTESIAN_POINT('Ctrl Pts',(-0.0968162919920292,-0.00181043050527611,
-0.686307376532398));
#40579=CARTESIAN_POINT('Ctrl Pts',(-0.0968275057127055,-0.00121075498492486,
-0.686347053791943));
#40580=CARTESIAN_POINT('Ctrl Pts',(-0.0968325971948741,-0.000610964980873346,
-0.686386731051487));
#40581=CARTESIAN_POINT('Ctrl Pts',(-0.0968316171384256,-1.1157892015598E-5,
-0.686426408311032));
#40582=CARTESIAN_POINT('Ctrl Pts',(-0.09683317566692,-1.75825702407311E-6,
-0.692223591688967));
#40583=CARTESIAN_POINT('Ctrl Pts',(-0.0968417798718537,-0.0320869529029069,
-0.69010106273961));
#40584=CARTESIAN_POINT('Ctrl Pts',(-0.0793039408690168,-0.0641639627296817,
-0.687978533790253));
#40585=CARTESIAN_POINT('Ctrl Pts',(-0.052301429073298,-0.0814937561131604,
-0.685856004840896));
#40586=CARTESIAN_POINT('Ctrl Pts',(-0.0253782020311814,-0.0987726657711256,
-0.683739708059347));
#40587=CARTESIAN_POINT('Ctrl Pts',(0.0109540616794619,-0.101390833779945,
-0.681623411277799));
#40588=CARTESIAN_POINT('Ctrl Pts',(0.0400765472079607,-0.0881506785704375,
-0.67950711449625));
#40589=CARTESIAN_POINT('Ctrl Pts',(0.0691990327364591,-0.0749105233609298,
-0.677390817714702));
#40590=CARTESIAN_POINT('Ctrl Pts',(0.0911117400828133,-0.0458120449330938,
-0.675274520933153));
#40591=CARTESIAN_POINT('Ctrl Pts',(0.0957915330844569,-0.0141652376566684,
-0.673158224151605));
#40592=CARTESIAN_POINT('Ctrl Pts',(0.1004713260861,0.0174815696197567,-0.671041927370057));
#40593=CARTESIAN_POINT('Ctrl Pts',(0.0879182047430347,0.0516767057447719,
-0.668925630588508));
#40594=CARTESIAN_POINT('Ctrl Pts',(0.0638741178933472,0.07277890375574,
-0.66680933380696));
#40595=CARTESIAN_POINT('Ctrl Pts',(0.039830031043659,0.0938811017667088,
-0.664693037025411));
#40596=CARTESIAN_POINT('Ctrl Pts',(0.00429497868734867,0.101890361663629,
-0.662576740243863));
#40597=CARTESIAN_POINT('Ctrl Pts',(-0.026476878396567,0.0931431515405931,
-0.660460443462315));
#40598=CARTESIAN_POINT('Ctrl Pts',(-0.0572487354804823,0.084395941417557,
-0.658344146680766));
#40599=CARTESIAN_POINT('Ctrl Pts',(-0.0832573972920026,0.0588922612745646,
-0.656227849899217));
#40600=CARTESIAN_POINT('Ctrl Pts',(-0.0926061887821478,0.0282978014655855,
-0.654111553117669));
#40601=CARTESIAN_POINT('Ctrl Pts',(-0.0953862269904411,0.0191999659516889,
-0.653482232641435));
#40602=CARTESIAN_POINT('Ctrl Pts',(-0.0966930635408328,0.0096519621652146,
-0.6528529121652));
#40603=CARTESIAN_POINT('Ctrl Pts',(-0.0966146360987624,8.30122117530267E-5,
-0.652223591688966));
#40604=CARTESIAN_POINT('Origin',(0.,0.,-0.593));
#40605=CARTESIAN_POINT('',(-0.0965338432881175,-4.16383404607604E-5,-0.606426408311032));
#40606=CARTESIAN_POINT('',(-0.0965410275132817,-4.88435499436115E-5,-0.612223591688966));
#40607=CARTESIAN_POINT('',(-0.096675,-1.1839272930757E-17,-0.593));
#40608=CARTESIAN_POINT('Ctrl Pts',(-0.0965338432881175,-4.16383404607604E-5,
-0.606426408311032));
#40609=CARTESIAN_POINT('Ctrl Pts',(-0.0964609475612972,0.0187219270939628,
-0.607657836339573));
#40610=CARTESIAN_POINT('Ctrl Pts',(-0.0911876223337323,0.0375233571128565,
-0.608889264368114));
#40611=CARTESIAN_POINT('Ctrl Pts',(-0.0809816167434835,0.0530909578300473,
-0.610120692396655));
#40612=CARTESIAN_POINT('Ctrl Pts',(-0.0634418691638409,0.0798449885412464,
-0.612236989178203));
#40613=CARTESIAN_POINT('Ctrl Pts',(-0.0313335139014484,0.0970479462159885,
-0.614353285959752));
#40614=CARTESIAN_POINT('Ctrl Pts',(0.000656700771827244,0.0968309908954595,
-0.616469582741301));
#40615=CARTESIAN_POINT('Ctrl Pts',(0.0326469154451024,0.0966140355749306,
-0.618585879522849));
#40616=CARTESIAN_POINT('Ctrl Pts',(0.0645189895292607,0.0789771672591311,
-0.620702176304397));
#40617=CARTESIAN_POINT('Ctrl Pts',(0.0816942526081138,0.051987701858247,
-0.622818473085946));
#40618=CARTESIAN_POINT('Ctrl Pts',(0.0988695156869669,0.0249982364573629,
-0.624934769867494));
#40619=CARTESIAN_POINT('Ctrl Pts',(0.101347967760515,-0.0113438260286058,
-0.627051066649043));
#40620=CARTESIAN_POINT('Ctrl Pts',(0.0879959350105063,-0.0404151886711796,
-0.629167363430591));
#40621=CARTESIAN_POINT('Ctrl Pts',(0.0746439022604976,-0.0694865513137538,
-0.631283660212139));
#40622=CARTESIAN_POINT('Ctrl Pts',(0.0454613846869319,-0.0912872141129328,
-0.633399956993688));
#40623=CARTESIAN_POINT('Ctrl Pts',(0.0137968171766093,-0.0958452914310114,
-0.635516253775236));
#40624=CARTESIAN_POINT('Ctrl Pts',(-0.0178677503337125,-0.10040336874909,
-0.637632550556785));
#40625=CARTESIAN_POINT('Ctrl Pts',(-0.0520143677807911,-0.0877188605860689,
-0.639748847338333));
#40626=CARTESIAN_POINT('Ctrl Pts',(-0.0730239612294275,-0.063593813693341,
-0.641865144119882));
#40627=CARTESIAN_POINT('Ctrl Pts',(-0.0881179857070617,-0.0462615388345649,
-0.643385565516932));
#40628=CARTESIAN_POINT('Ctrl Pts',(-0.0964313528738214,-0.0230242452602008,
-0.644905986913982));
#40629=CARTESIAN_POINT('Ctrl Pts',(-0.0966287398315909,8.55332849566889E-5,
-0.646426408311032));
#40630=CARTESIAN_POINT('Ctrl Pts',(-0.0966146360987624,8.30122117530267E-5,
-0.652223591688966));
#40631=CARTESIAN_POINT('Ctrl Pts',(-0.0964293255098825,-0.0225267746692927,
-0.650736615383652));
#40632=CARTESIAN_POINT('Ctrl Pts',(-0.0885101440476594,-0.0452535031236791,
-0.649249639078338));
#40633=CARTESIAN_POINT('Ctrl Pts',(-0.0740171277690317,-0.0624350587840144,
-0.647762662773024));
#40634=CARTESIAN_POINT('Ctrl Pts',(-0.0533903540970001,-0.0868882197496698,
-0.645646365991476));
#40635=CARTESIAN_POINT('Ctrl Pts',(-0.0194478855841665,-0.100109302206014,
-0.643530069209927));
#40636=CARTESIAN_POINT('Ctrl Pts',(0.0122845840146836,-0.0960508238596976,
-0.641413772428379));
#40637=CARTESIAN_POINT('Ctrl Pts',(0.0440170536135328,-0.091992345513381,
-0.63929747564683));
#40638=CARTESIAN_POINT('Ctrl Pts',(0.0735395242983992,-0.070654306364404,
-0.637181178865282));
#40639=CARTESIAN_POINT('Ctrl Pts',(0.0873480625364419,-0.0417969824230209,
-0.635064882083734));
#40640=CARTESIAN_POINT('Ctrl Pts',(0.101156600774485,-0.0129396584816366,
-0.632948585302185));
#40641=CARTESIAN_POINT('Ctrl Pts',(0.0992512065657041,0.0234369502521536,
-0.630832288520637));
#40642=CARTESIAN_POINT('Ctrl Pts',(0.0825034301615626,0.0506937449801911,
-0.628715991739088));
#40643=CARTESIAN_POINT('Ctrl Pts',(0.0657556537574214,0.0779505397082283,
-0.62659969495754));
#40644=CARTESIAN_POINT('Ctrl Pts',(0.0341654951579198,0.0960875204305122,
-0.624483398175992));
#40645=CARTESIAN_POINT('Ctrl Pts',(0.00218267324238817,0.0968086138009291,
-0.622367101394443));
#40646=CARTESIAN_POINT('Ctrl Pts',(-0.0298001486731421,0.0975297071713459,
-0.620250804612895));
#40647=CARTESIAN_POINT('Ctrl Pts',(-0.0621756339047028,0.0808349131898973,
-0.618134507831346));
#40648=CARTESIAN_POINT('Ctrl Pts',(-0.0801348457163669,0.0543606316239479,
-0.616018211049797));
#40649=CARTESIAN_POINT('Ctrl Pts',(-0.0908687486736435,0.0385374222218539,
-0.61475333792952));
#40650=CARTESIAN_POINT('Ctrl Pts',(-0.0964528109375644,0.0192207439005784,
-0.613488464809243));
#40651=CARTESIAN_POINT('Ctrl Pts',(-0.0965410275132817,-4.88435499436115E-5,
-0.612223591688966));
#40652=CARTESIAN_POINT('Origin',(0.,0.,-0.593));
#40653=CARTESIAN_POINT('',(-0.0967807988947103,-6.24008650121077E-5,-0.566426408311032));
#40654=CARTESIAN_POINT('',(-0.0967926476771765,-5.56256174443557E-5,-0.572223591688966));
#40655=CARTESIAN_POINT('',(-0.096675,-1.1839272930757E-17,-0.593));
#40656=CARTESIAN_POINT('Ctrl Pts',(-0.0967807988947103,-6.24008650121077E-5,
-0.566426408311032));
#40657=CARTESIAN_POINT('Ctrl Pts',(-0.0965688219293542,0.0282002888768916,
-0.568293388983616));
#40658=CARTESIAN_POINT('Ctrl Pts',(-0.0834609918028184,0.0566341393471626,
-0.5701603696562));
#40659=CARTESIAN_POINT('Ctrl Pts',(-0.0617127749374913,0.0746204091600604,
-0.572027350328784));
#40660=CARTESIAN_POINT('Ctrl Pts',(-0.0370603069005264,0.0950085607226655,
-0.574143647110332));
#40661=CARTESIAN_POINT('Ctrl Pts',(-0.00130569935051607,0.101972487011741,
-0.576259943891881));
#40662=CARTESIAN_POINT('Ctrl Pts',(0.0291964597445464,0.0923268042991058,
-0.578376240673429));
#40663=CARTESIAN_POINT('Ctrl Pts',(0.0596986188396094,0.0826811215864704,
-0.580492537454977));
#40664=CARTESIAN_POINT('Ctrl Pts',(0.0849483294797243,0.0564258298721237,
-0.582608834236526));
#40665=CARTESIAN_POINT('Ctrl Pts',(0.0933960700192532,0.0255704156919484,
-0.584725131018074));
#40666=CARTESIAN_POINT('Ctrl Pts',(0.101843810558782,-0.00528499848822653,
-0.586841427799623));
#40667=CARTESIAN_POINT('Ctrl Pts',(0.0934895809977251,-0.0407405351342299,
-0.588957724581171));
#40668=CARTESIAN_POINT('Ctrl Pts',(0.0721547065196973,-0.0645784049102844,
-0.59107402136272));
#40669=CARTESIAN_POINT('Ctrl Pts',(0.0508198320416695,-0.0884162746863389,
-0.593190318144268));
#40670=CARTESIAN_POINT('Ctrl Pts',(0.0165043126466707,-0.100636477592444,
-0.595306614925816));
#40671=CARTESIAN_POINT('Ctrl Pts',(-0.0150955199455927,-0.095649345691816,
-0.597422911707365));
#40672=CARTESIAN_POINT('Ctrl Pts',(-0.046695352537856,-0.0906622137911875,
-0.599539208488913));
#40673=CARTESIAN_POINT('Ctrl Pts',(-0.0755794983273839,-0.0684677470838248,
-0.601655505270462));
#40674=CARTESIAN_POINT('Ctrl Pts',(-0.0885360012737014,-0.0392179618563158,
-0.60377180205201));
#40675=CARTESIAN_POINT('Ctrl Pts',(-0.0939533910771552,-0.0269880037494673,
-0.604656670805017));
#40676=CARTESIAN_POINT('Ctrl Pts',(-0.0965862240601935,-0.0135245966320609,
-0.605541539558025));
#40677=CARTESIAN_POINT('Ctrl Pts',(-0.0965338432881175,-4.16383404607604E-5,
-0.606426408311032));
#40678=CARTESIAN_POINT('Ctrl Pts',(-0.0965410275132817,-4.88435499436115E-5,
-0.612223591688966));
#40679=CARTESIAN_POINT('Ctrl Pts',(-0.0966004087102398,-0.0130197751282173,
-0.611372168027695));
#40680=CARTESIAN_POINT('Ctrl Pts',(-0.0941696024950817,-0.0259693696638901,
-0.610520744366424));
#40681=CARTESIAN_POINT('Ctrl Pts',(-0.0891430782153712,-0.0378177653336196,
-0.609669320705153));
#40682=CARTESIAN_POINT('Ctrl Pts',(-0.0766491605109436,-0.0672681115747841,
-0.607553023923604));
#40683=CARTESIAN_POINT('Ctrl Pts',(-0.0481183867103214,-0.0899150349066602,
-0.605436727142056));
#40684=CARTESIAN_POINT('Ctrl Pts',(-0.016601076251763,-0.0953995599351676,
-0.603320430360507));
#40685=CARTESIAN_POINT('Ctrl Pts',(0.014916234206795,-0.100884084963675,
-0.601204133578959));
#40686=CARTESIAN_POINT('Ctrl Pts',(0.0494200813232888,-0.0892062116888138,
-0.59908783679741));
#40687=CARTESIAN_POINT('Ctrl Pts',(0.071127990010792,-0.065707539944554,
-0.596971540015862));
#40688=CARTESIAN_POINT('Ctrl Pts',(0.0928358986982952,-0.0422088682002942,
-0.594855243234314));
#40689=CARTESIAN_POINT('Ctrl Pts',(0.101747868956808,-0.00688939798663464,
-0.592738946452765));
#40690=CARTESIAN_POINT('Ctrl Pts',(0.0937874582926693,0.024095319784998,
-0.590622649671217));
#40691=CARTESIAN_POINT('Ctrl Pts',(0.0858270476285311,0.0550800375566302,
-0.588506352889668));
#40692=CARTESIAN_POINT('Ctrl Pts',(0.0609942560417432,0.0817300028862363,
-0.586390056108119));
#40693=CARTESIAN_POINT('Ctrl Pts',(0.0306479013833725,0.0918552007745646,
-0.584273759326571));
#40694=CARTESIAN_POINT('Ctrl Pts',(0.000301546725000868,0.101980398662893,
-0.582157462545023));
#40695=CARTESIAN_POINT('Ctrl Pts',(-0.0355583710049534,0.0955808291099426,
-0.580041165763475));
#40696=CARTESIAN_POINT('Ctrl Pts',(-0.0605290936942883,0.075583732278107,
-0.577924868981926));
#40697=CARTESIAN_POINT('Ctrl Pts',(-0.0829526994788125,0.05762642196031,
-0.576024443217606));
#40698=CARTESIAN_POINT('Ctrl Pts',(-0.0965952956441005,0.0287041121739278,
-0.574124017453286));
#40699=CARTESIAN_POINT('Ctrl Pts',(-0.0967926476771765,-5.56256174443557E-5,
-0.572223591688966));
#40700=CARTESIAN_POINT('Origin',(0.,0.,-0.593));
#40701=CARTESIAN_POINT('',(-0.0967237190630299,8.23214974291983E-5,-0.526426408311032));
#40702=CARTESIAN_POINT('',(-0.0967085211101146,8.50951967561498E-5,-0.532223591688966));
#40703=CARTESIAN_POINT('',(-0.096675,-1.1839272930757E-17,-0.593));
#40704=CARTESIAN_POINT('Ctrl Pts',(-0.0967237190630299,8.23214974291983E-5,
-0.526426408311032));
#40705=CARTESIAN_POINT('Ctrl Pts',(-0.0967766851406952,0.00593821845587171,
-0.52681264484611));
#40706=CARTESIAN_POINT('Ctrl Pts',(-0.0962905307316554,0.0117853401103693,
-0.527198881381188));
#40707=CARTESIAN_POINT('Ctrl Pts',(-0.09523371832439,0.0175274341479589,
-0.527585117916267));
#40708=CARTESIAN_POINT('Ctrl Pts',(-0.0894431509050166,0.0489899552391718,
-0.529701414697815));
#40709=CARTESIAN_POINT('Ctrl Pts',(-0.0665200201184249,0.0772992877172744,
-0.531817711479364));
#40710=CARTESIAN_POINT('Ctrl Pts',(-0.0369496419739366,0.089506402071015,
-0.533934008260912));
#40711=CARTESIAN_POINT('Ctrl Pts',(-0.0073792638294475,0.101713516424756,
-0.536050305042461));
#40712=CARTESIAN_POINT('Ctrl Pts',(0.0288383616729391,0.097818412654134,
-0.538166601824009));
#40713=CARTESIAN_POINT('Ctrl Pts',(0.0551368565792162,0.0796027581196986,
-0.540282898605557));
#40714=CARTESIAN_POINT('Ctrl Pts',(0.0814353514854927,0.0613871035852636,
-0.542399195387106));
#40715=CARTESIAN_POINT('Ctrl Pts',(0.0978147157956604,0.0288508982870171,
-0.544515492168655));
#40716=CARTESIAN_POINT('Ctrl Pts',(0.0967828310716766,-0.00312340574559222,
-0.546631788950203));
#40717=CARTESIAN_POINT('Ctrl Pts',(0.0957509463476929,-0.0350977097782011,
-0.548748085731751));
#40718=CARTESIAN_POINT('Ctrl Pts',(0.0773078125895573,-0.0665101125451723,
-0.550864382513299));
#40719=CARTESIAN_POINT('Ctrl Pts',(0.0498895412279715,-0.0829922028251017,
-0.552980679294848));
#40720=CARTESIAN_POINT('Ctrl Pts',(0.0224712698663842,-0.0994742931050322,
-0.555096976076396));
#40721=CARTESIAN_POINT('Ctrl Pts',(-0.0139221390986548,-0.101026070897919,
-0.557213272857945));
#40722=CARTESIAN_POINT('Ctrl Pts',(-0.0426439022409416,-0.0869377343583631,
-0.559329569639493));
#40723=CARTESIAN_POINT('Ctrl Pts',(-0.0713656653832267,-0.0728493978188077,
-0.561445866421042));
#40724=CARTESIAN_POINT('Ctrl Pts',(-0.0924157827027609,-0.0431209469468107,
-0.56356216320259));
#40725=CARTESIAN_POINT('Ctrl Pts',(-0.0961656771005684,-0.0113505330927453,
-0.565678459984138));
#40726=CARTESIAN_POINT('Ctrl Pts',(-0.0966074436280423,-0.00760773291871241,
-0.565927776093103));
#40727=CARTESIAN_POINT('Ctrl Pts',(-0.0968091062430234,-0.0038365930346435,
-0.566177092202067));
#40728=CARTESIAN_POINT('Ctrl Pts',(-0.0967807988947103,-6.24008650121077E-5,
-0.566426408311032));
#40729=CARTESIAN_POINT('Ctrl Pts',(-0.0967926476771765,-5.56256174443557E-5,
-0.572223591688966));
#40730=CARTESIAN_POINT('Ctrl Pts',(-0.0968150650664437,-0.00332246927364548,
-0.572007720671738));
#40731=CARTESIAN_POINT('Ctrl Pts',(-0.0966640000047558,-0.00658721528194418,
-0.571791849654509));
#40732=CARTESIAN_POINT('Ctrl Pts',(-0.0963326163565946,-0.00983355451673743,
-0.57157597863728));
#40733=CARTESIAN_POINT('Ctrl Pts',(-0.0930838886808508,-0.0416591203690247,
-0.569459681855732));
#40734=CARTESIAN_POINT('Ctrl Pts',(-0.0725049056806487,-0.0717156279628795,
-0.567343385074184));
#40735=CARTESIAN_POINT('Ctrl Pts',(-0.0440087419449873,-0.0862548688536479,
-0.565227088292636));
#40736=CARTESIAN_POINT('Ctrl Pts',(-0.015512578209325,-0.100794109744417,
-0.563110791511087));
#40737=CARTESIAN_POINT('Ctrl Pts',(0.020900766261797,-0.0998160839320984,
-0.560994494729539));
#40738=CARTESIAN_POINT('Ctrl Pts',(0.0485753893016762,-0.0837681521983809,
-0.55887819794799));
#40739=CARTESIAN_POINT('Ctrl Pts',(0.0762500123415555,-0.0677202204646633,
-0.556761901166442));
#40740=CARTESIAN_POINT('Ctrl Pts',(0.095185913950192,-0.0366023828095467,
-0.554645604384894));
#40741=CARTESIAN_POINT('Ctrl Pts',(0.0967215847492896,-0.00464831282579854,
-0.552529307603345));
#40742=CARTESIAN_POINT('Ctrl Pts',(0.0982572555483871,0.0273057571579487,
-0.550413010821796));
#40743=CARTESIAN_POINT('Ctrl Pts',(0.0823926955379466,0.0600960594703274,
-0.548296714040247));
#40744=CARTESIAN_POINT('Ctrl Pts',(0.0563845454712289,0.0787239150483727,
-0.546180417258699));
#40745=CARTESIAN_POINT('Ctrl Pts',(0.0303763954045105,0.0973517706264184,
-0.544064120477151));
#40746=CARTESIAN_POINT('Ctrl Pts',(-0.00577534471848571,0.10181717947013,
-0.541947823695603));
#40747=CARTESIAN_POINT('Ctrl Pts',(-0.0355344337095269,0.0900776098122266,
-0.539831526914055));
#40748=CARTESIAN_POINT('Ctrl Pts',(-0.0652935227005681,0.0783380401543233,
-0.537715230132506));
#40749=CARTESIAN_POINT('Ctrl Pts',(-0.0886599605596542,0.0503934919948053,
-0.535598933350957));
#40750=CARTESIAN_POINT('Ctrl Pts',(-0.0949456572852223,0.0190261381057114,
-0.533482636569409));
#40751=CARTESIAN_POINT('Ctrl Pts',(-0.096192170274538,0.0128056957633096,
-0.533062954942594));
#40752=CARTESIAN_POINT('Ctrl Pts',(-0.096766955217955,0.00645064599455275,
-0.53264327331578));
#40753=CARTESIAN_POINT('Ctrl Pts',(-0.0967085211101146,8.50951967561498E-5,
-0.532223591688966));
#40754=CARTESIAN_POINT('Origin',(0.,0.,-0.593));
#40755=CARTESIAN_POINT('',(-0.0965172713955322,9.07121298592689E-6,-0.486426408311032));
#40756=CARTESIAN_POINT('',(-0.0965164910401789,7.28318461152001E-7,-0.492223591688966));
#40757=CARTESIAN_POINT('',(-0.096675,-1.1839272930757E-17,-0.593));
#40758=CARTESIAN_POINT('Ctrl Pts',(-0.0965172713955322,9.07121298592689E-6,
-0.486426408311032));
#40759=CARTESIAN_POINT('Ctrl Pts',(-0.0965303204669342,0.0155849964339054,
-0.487448197490153));
#40760=CARTESIAN_POINT('Ctrl Pts',(-0.0929763058240226,0.0311553037760087,
-0.488469986669274));
#40761=CARTESIAN_POINT('Ctrl Pts',(-0.0858230972773667,0.0448449331298415,
-0.489491775848395));
#40762=CARTESIAN_POINT('Ctrl Pts',(-0.0710076025213427,0.0731984517754618,
-0.491608072629944));
#40763=CARTESIAN_POINT('Ctrl Pts',(-0.0407525168478783,0.0934843587383312,
-0.493724369411492));
#40764=CARTESIAN_POINT('Ctrl Pts',(-0.00889688070606006,0.0964236359374735,
-0.495840666193041));
#40765=CARTESIAN_POINT('Ctrl Pts',(0.0229587554357591,0.0993629131366158,
-0.497956962974589));
#40766=CARTESIAN_POINT('Ctrl Pts',(0.0564149420459315,0.08495556057203,
-0.500073259756137));
#40767=CARTESIAN_POINT('Ctrl Pts',(0.0761684165666363,0.0597916747669077,
-0.502189556537686));
#40768=CARTESIAN_POINT('Ctrl Pts',(0.0959218910873405,0.034627788961786,
-0.504305853319234));
#40769=CARTESIAN_POINT('Ctrl Pts',(0.101972653518578,-0.00129263008387249,
-0.506422150100783));
#40770=CARTESIAN_POINT('Ctrl Pts',(0.091553012274957,-0.0315391502276436,
-0.508538446882331));
#40771=CARTESIAN_POINT('Ctrl Pts',(0.081133371031336,-0.0617856703714156,
-0.510654743663879));
#40772=CARTESIAN_POINT('Ctrl Pts',(0.0542433261128582,-0.0863582916133,
-0.512771040445428));
#40773=CARTESIAN_POINT('Ctrl Pts',(0.0231827078132096,-0.094017201150362,
-0.514887337226976));
#40774=CARTESIAN_POINT('Ctrl Pts',(-0.00787791048643809,-0.101676110687424,
-0.517003634008525));
#40775=CARTESIAN_POINT('Ctrl Pts',(-0.0431091021672566,-0.0924213085196625,
-0.519119930790073));
#40776=CARTESIAN_POINT('Ctrl Pts',(-0.0663956959815876,-0.0704860525836203,
-0.521236227571622));
#40777=CARTESIAN_POINT('Ctrl Pts',(-0.0854323502850516,-0.0525541090953691,
-0.522966287818092));
#40778=CARTESIAN_POINT('Ctrl Pts',(-0.0964864693544764,-0.026147860308577,
-0.524696348064562));
#40779=CARTESIAN_POINT('Ctrl Pts',(-0.0967237190630299,8.23214974291983E-5,
-0.526426408311032));
#40780=CARTESIAN_POINT('Ctrl Pts',(-0.0967085211101146,8.50951967561498E-5,
-0.532223591688966));
#40781=CARTESIAN_POINT('Ctrl Pts',(-0.0964722939641516,-0.0256484353219682,
-0.530526976534232));
#40782=CARTESIAN_POINT('Ctrl Pts',(-0.0858874872503391,-0.0515535821784303,
-0.528830361379498));
#40783=CARTESIAN_POINT('Ctrl Pts',(-0.0674983073426272,-0.0694309028777585,
-0.527133746224764));
#40784=CARTESIAN_POINT('Ctrl Pts',(-0.0445603050824128,-0.091730430353467,
-0.525017449443216));
#40785=CARTESIAN_POINT('Ctrl Pts',(-0.00947934496993338,-0.101539325686214,
-0.522901152661667));
#40786=CARTESIAN_POINT('Ctrl Pts',(0.0216981194752549,-0.0943708820546786,
-0.520784855880119));
#40787=CARTESIAN_POINT('Ctrl Pts',(0.0528755839204423,-0.0872024384231437,
-0.51866855909857));
#40788=CARTESIAN_POINT('Ctrl Pts',(0.0801495526983388,-0.0630566558273281,
-0.516552262317022));
#40789=CARTESIAN_POINT('Ctrl Pts',(0.0910445841196321,-0.0329781059344485,
-0.514435965535473));
#40790=CARTESIAN_POINT('Ctrl Pts',(0.101939615540926,-0.0028995560415681,
-0.512319668753925));
#40791=CARTESIAN_POINT('Ctrl Pts',(0.0964557096056154,0.0331117611483767,
-0.510203371972377));
#40792=CARTESIAN_POINT('Ctrl Pts',(0.0771012709130743,0.0585838355873803,
-0.508087075190828));
#40793=CARTESIAN_POINT('Ctrl Pts',(0.0577468322205332,0.0840559100263839,
-0.50597077840928));
#40794=CARTESIAN_POINT('Ctrl Pts',(0.0245218607707614,0.0989887417144463,
-0.503854481627731));
#40795=CARTESIAN_POINT('Ctrl Pts',(-0.00737614147654734,0.0965518736506882,
-0.501738184846183));
#40796=CARTESIAN_POINT('Ctrl Pts',(-0.0392741437238552,0.0941150055869301,
-0.499621888064634));
#40797=CARTESIAN_POINT('Ctrl Pts',(-0.0698451767686999,0.0743084377713525,
-0.497505591283086));
#40798=CARTESIAN_POINT('Ctrl Pts',(-0.0851056820304146,0.0461919327878629,
-0.495389294501538));
#40799=CARTESIAN_POINT('Ctrl Pts',(-0.0927149210951618,0.0321723964477871,
-0.494334060230681));
#40800=CARTESIAN_POINT('Ctrl Pts',(-0.0965175816304359,0.0160868027612428,
-0.493278825959824));
#40801=CARTESIAN_POINT('Ctrl Pts',(-0.0965165001841129,7.28276446517835E-7,
-0.492223591688966));
#40802=CARTESIAN_POINT('Origin',(0.,0.,-0.593));
#40803=CARTESIAN_POINT('',(-0.096690457956298,-8.72527295337211E-5,-0.446426408311032));
#40804=CARTESIAN_POINT('',(-0.0967058503150131,-8.54906923442515E-5,-0.452223591688966));
#40805=CARTESIAN_POINT('',(-0.096675,-1.1839272930757E-17,-0.593));
#40806=CARTESIAN_POINT('Ctrl Pts',(-0.096690457956298,-8.72527295337211E-5,
-0.446426408311032));
#40807=CARTESIAN_POINT('Ctrl Pts',(-0.0964584083749974,0.0250626678574959,
-0.448083750134195));
#40808=CARTESIAN_POINT('Ctrl Pts',(-0.0864088916390611,0.0503769466530735,
-0.449741091957359));
#40809=CARTESIAN_POINT('Ctrl Pts',(-0.0687716419790343,0.0681698856769454,
-0.451398433780523));
#40810=CARTESIAN_POINT('Ctrl Pts',(-0.0462502440578617,0.0908900868232714,
-0.453514730562072));
#40811=CARTESIAN_POINT('Ctrl Pts',(-0.0113568151501427,0.101346513051999,
-0.455631027343621));
#40812=CARTESIAN_POINT('Ctrl Pts',(0.0199479702554438,0.0947562691139126,
-0.457747324125169));
#40813=CARTESIAN_POINT('Ctrl Pts',(0.0512527556610312,0.0881660251758255,
-0.459863620906718));
#40814=CARTESIAN_POINT('Ctrl Pts',(0.0789688975644853,0.0645291110709228,
-0.461979917688266));
#40815=CARTESIAN_POINT('Ctrl Pts',(0.0904186989652336,0.0346573358920554,
-0.464096214469814));
#40816=CARTESIAN_POINT('Ctrl Pts',(0.101868500365982,0.00478556071318895,
-0.466212511251362));
#40817=CARTESIAN_POINT('Ctrl Pts',(0.097051961264024,-0.0313210755396426,
-0.468328808032911));
#40818=CARTESIAN_POINT('Ctrl Pts',(0.0781722246342648,-0.0571469627314554,
-0.47044510481446));
#40819=CARTESIAN_POINT('Ctrl Pts',(0.0592924880045052,-0.0829728499232685,
-0.472561401596008));
#40820=CARTESIAN_POINT('Ctrl Pts',(0.026349553846944,-0.0985179880540636,
-0.474677698377556));
#40821=CARTESIAN_POINT('Ctrl Pts',(-0.00558808313182638,-0.0966718437840723,
-0.476793995159105));
#40822=CARTESIAN_POINT('Ctrl Pts',(-0.0375257201105967,-0.094825699514081,
-0.478910291940653));
#40823=CARTESIAN_POINT('Ctrl Pts',(-0.0684580599105757,-0.0755882728433033,
-0.481026588722201));
#40824=CARTESIAN_POINT('Ctrl Pts',(-0.0842362778912744,-0.0477589943437285,
-0.48314288550375));
#40825=CARTESIAN_POINT('Ctrl Pts',(-0.0923964658588589,-0.033366231876092,
-0.484237393106177));
#40826=CARTESIAN_POINT('Ctrl Pts',(-0.0965032936512519,-0.0166753573535768,
-0.485331900708604));
#40827=CARTESIAN_POINT('Ctrl Pts',(-0.0965172713955322,9.07121298592689E-6,
-0.486426408311032));
#40828=CARTESIAN_POINT('Ctrl Pts',(-0.0965165001841129,7.28276446517835E-7,
-0.492223591688966));
#40829=CARTESIAN_POINT('Ctrl Pts',(-0.0965154127647765,-0.0161741923562409,
-0.491162529178275));
#40830=CARTESIAN_POINT('Ctrl Pts',(-0.0926684498905901,-0.0323495991129097,
-0.490101466667584));
#40831=CARTESIAN_POINT('Ctrl Pts',(-0.084978495369719,-0.0464255004629906,
-0.489040404156892));
#40832=CARTESIAN_POINT('Ctrl Pts',(-0.0696408259687238,-0.0744999865789511,
-0.486924107375344));
#40833=CARTESIAN_POINT('Ctrl Pts',(-0.0390155096881494,-0.0942225166594689,
-0.484807810593795));
#40834=CARTESIAN_POINT('Ctrl Pts',(-0.0071109349142395,-0.0965717679924415,
-0.482691513812247));
#40835=CARTESIAN_POINT('Ctrl Pts',(0.0247936398596695,-0.098921019325414,
-0.480575217030698));
#40836=CARTESIAN_POINT('Ctrl Pts',(0.0579774731269135,-0.0838969919108423,
-0.47845892024915));
#40837=CARTESIAN_POINT('Ctrl Pts',(0.0772618800277791,-0.0583718567728794,
-0.476342623467602));
#40838=CARTESIAN_POINT('Ctrl Pts',(0.0965462869286451,-0.0328467216349161,
-0.474226326686053));
#40839=CARTESIAN_POINT('Ctrl Pts',(0.101931267463132,0.00317952122643966,
-0.472110029904505));
#40840=CARTESIAN_POINT('Ctrl Pts',(0.0909536667012348,0.033228034581377,
-0.469993733122956));
#40841=CARTESIAN_POINT('Ctrl Pts',(0.0799760659393374,0.0632765479363147,
-0.467877436341408));
#40842=CARTESIAN_POINT('Ctrl Pts',(0.052635883881056,0.0873473317848345,
-0.465761139559859));
#40843=CARTESIAN_POINT('Ctrl Pts',(0.0214388489673388,0.0944301197896949,
-0.463644842778311));
#40844=CARTESIAN_POINT('Ctrl Pts',(-0.00975818594637752,0.101512907794555,
-0.461528545996763));
#40845=CARTESIAN_POINT('Ctrl Pts',(-0.0448120737155289,0.0916076999557566,
-0.459412249215214));
#40846=CARTESIAN_POINT('Ctrl Pts',(-0.0676887440363411,0.0692452575944605,
-0.457295952433666));
#40847=CARTESIAN_POINT('Ctrl Pts',(-0.0859657528056922,0.0513790843529079,
-0.455605165518766));
#40848=CARTESIAN_POINT('Ctrl Pts',(-0.0964700478136312,0.025561462546613,
-0.453914378603866));
#40849=CARTESIAN_POINT('Ctrl Pts',(-0.0967058503150131,-8.54906923442515E-5,
-0.452223591688966));
#40850=CARTESIAN_POINT('Origin',(0.,0.,-0.593));
#40851=CARTESIAN_POINT('',(-0.0968050622971842,4.68532484065691E-5,-0.406426408311032));
#40852=CARTESIAN_POINT('',(-0.0967945983128168,5.43772629733152E-5,-0.412223591688966));
#40853=CARTESIAN_POINT('',(-0.096675,-1.1839272930757E-17,-0.593));
#40854=CARTESIAN_POINT('Ctrl Pts',(-0.0968050622971842,4.68532484065691E-5,
-0.406426408311032));
#40855=CARTESIAN_POINT('Ctrl Pts',(-0.0968210205998854,0.00271845753054062,
-0.40660300599669));
#40856=CARTESIAN_POINT('Ctrl Pts',(-0.0967200026210178,0.00538883683724322,
-0.406779603682348));
#40857=CARTESIAN_POINT('Ctrl Pts',(-0.0964981010810641,0.00804913296256427,
-0.406956201368007));
#40858=CARTESIAN_POINT('Ctrl Pts',(-0.0938388957065765,0.0399293702770765,
-0.409072498149555));
#40859=CARTESIAN_POINT('Ctrl Pts',(-0.0738196642753906,0.0703615670975442,
-0.411188794931103));
#40860=CARTESIAN_POINT('Ctrl Pts',(-0.0455974442696008,0.0854256702038734,
-0.413305091712652));
#40861=CARTESIAN_POINT('Ctrl Pts',(-0.0173752242638107,0.100489773310203,
-0.4154213884942));
#40862=CARTESIAN_POINT('Ctrl Pts',(0.0190499843165828,0.100185782702395,
-0.417537685275749));
#40863=CARTESIAN_POINT('Ctrl Pts',(0.0470168525184595,0.0846527473444171,
-0.419653982057297));
#40864=CARTESIAN_POINT('Ctrl Pts',(0.0749837207203371,0.0691197119864384,
-0.421770278838846));
#40865=CARTESIAN_POINT('Ctrl Pts',(0.0944922485436957,0.0383576318782866,
-0.423886575620394));
#40866=CARTESIAN_POINT('Ctrl Pts',(0.0966190004853783,0.00643745282753642,
-0.426002872401943));
#40867=CARTESIAN_POINT('Ctrl Pts',(0.0987457524270609,-0.0254827262232124,
-0.428119169183491));
#40868=CARTESIAN_POINT('Ctrl Pts',(0.0834907284870702,-0.0585610042165598,
-0.43023546596504));
#40869=CARTESIAN_POINT('Ctrl Pts',(0.0578317602814135,-0.0776669785459265,
-0.432351762746588));
#40870=CARTESIAN_POINT('Ctrl Pts',(0.0321727920757572,-0.096772952875293,
-0.434468059528136));
#40871=CARTESIAN_POINT('Ctrl Pts',(-0.00389012039556526,-0.101906623540679,
-0.436584356309685));
#40872=CARTESIAN_POINT('Ctrl Pts',(-0.0338613667816545,-0.0907197877718999,
-0.438700653091233));
#40873=CARTESIAN_POINT('Ctrl Pts',(-0.063832613167745,-0.0795329520031206,
-0.440816949872781));
#40874=CARTESIAN_POINT('Ctrl Pts',(-0.0877121934686019,-0.0520256098001765,
-0.44293324665433));
#40875=CARTESIAN_POINT('Ctrl Pts',(-0.0945773001517176,-0.0207799506667414,
-0.445049543435878));
#40876=CARTESIAN_POINT('Ctrl Pts',(-0.0960661153214635,-0.0140037979492643,
-0.445508498394263));
#40877=CARTESIAN_POINT('Ctrl Pts',(-0.0967547176669023,-0.00705182732426255,
-0.445967453352647));
#40878=CARTESIAN_POINT('Ctrl Pts',(-0.096690457956298,-8.72527295337211E-5,
-0.446426408311032));
#40879=CARTESIAN_POINT('Ctrl Pts',(-0.0967058503150131,-8.54906923442515E-5,
-0.452223591688966));
#40880=CARTESIAN_POINT('Ctrl Pts',(-0.0967651932694884,-0.00653990050382228,
-0.451798081822318));
#40881=CARTESIAN_POINT('Ctrl Pts',(-0.0961741846374927,-0.0129835010778726,
-0.451372571955669));
#40882=CARTESIAN_POINT('Ctrl Pts',(-0.0948930440917267,-0.019286833631939,
-0.450947062089021));
#40883=CARTESIAN_POINT('Ctrl Pts',(-0.0885212209538268,-0.0506368056132461,
-0.448830765307472));
#40884=CARTESIAN_POINT('Ctrl Pts',(-0.0650781218055549,-0.0785170726920666,
-0.446714468525924));
#40885=CARTESIAN_POINT('Ctrl Pts',(-0.0352869024451259,-0.090174865036598,
-0.444598171744375));
#40886=CARTESIAN_POINT('Ctrl Pts',(-0.00549568308469609,-0.10183265738113,
-0.442481874962827));
#40887=CARTESIAN_POINT('Ctrl Pts',(0.0306436564878915,-0.0972679749913715,
-0.440365578181279));
#40888=CARTESIAN_POINT('Ctrl Pts',(0.0566005472454594,-0.0785687585497888,
-0.43824928139973));
#40889=CARTESIAN_POINT('Ctrl Pts',(0.0825574380030276,-0.0598695421082059,
-0.436132984618182));
#40890=CARTESIAN_POINT('Ctrl Pts',(0.0983318799455758,-0.0270357916147993,
-0.434016687836633));
#40891=CARTESIAN_POINT('Ctrl Pts',(0.0967084534090917,0.00491394014636167,
-0.431900391055085));
#40892=CARTESIAN_POINT('Ctrl Pts',(0.0950850268726077,0.0368636719075213,
-0.429784094273536));
#40893=CARTESIAN_POINT('Ctrl Pts',(0.0760637318570921,0.0679293849364347,
-0.427667797491988));
#40894=CARTESIAN_POINT('Ctrl Pts',(0.048345137713258,0.0839012480719245,
-0.42555150071044));
#40895=CARTESIAN_POINT('Ctrl Pts',(0.0206265435694232,0.0998731112074149,
-0.423435203928891));
#40896=CARTESIAN_POINT('Ctrl Pts',(-0.015789349702731,0.100751124449481,
-0.421318907147343));
#40897=CARTESIAN_POINT('Ctrl Pts',(-0.0442454740842226,0.0861336739701893,
-0.419202610365794));
#40898=CARTESIAN_POINT('Ctrl Pts',(-0.0727015984657142,0.0715162234908976,
-0.417086313584246));
#40899=CARTESIAN_POINT('Ctrl Pts',(-0.0931979539565437,0.0414033092902477,
-0.414970016802697));
#40900=CARTESIAN_POINT('Ctrl Pts',(-0.0963592607853087,0.00956894087396099,
-0.412853720021149));
#40901=CARTESIAN_POINT('Ctrl Pts',(-0.0966730209688041,0.00640937496758658,
-0.412643677243755));
#40902=CARTESIAN_POINT('Ctrl Pts',(-0.0968160206487383,0.00323285171690641,
-0.41243363446636));
#40903=CARTESIAN_POINT('Ctrl Pts',(-0.0967945983128168,5.43772629733152E-5,
-0.412223591688966));
#40904=CARTESIAN_POINT('Origin',(0.,0.,-0.593));
#40905=CARTESIAN_POINT('',(-0.0965509256710446,5.67507499378977E-5,-0.366426408311032));
#40906=CARTESIAN_POINT('',(-0.0965423984694297,5.0056945484775E-5,-0.372223591688966));
#40907=CARTESIAN_POINT('',(-0.096675,-1.1839272930757E-17,-0.593));
#40908=CARTESIAN_POINT('Ctrl Pts',(-0.0965509256710446,5.67507499378977E-5,
-0.366426408311032));
#40909=CARTESIAN_POINT('Ctrl Pts',(-0.0966171433328029,0.0124262003756307,
-0.367238558640733));
#40910=CARTESIAN_POINT('Ctrl Pts',(-0.0944123650341302,0.0247729380575116,
-0.368050708970434));
#40911=CARTESIAN_POINT('Ctrl Pts',(-0.0898276716852722,0.036161601918378,
-0.368862859300135));
#40912=CARTESIAN_POINT('Ctrl Pts',(-0.0778809034285336,0.0658381184368829,
-0.370979156081684));
#40913=CARTESIAN_POINT('Ctrl Pts',(-0.0497741205849931,0.0890091561478041,
-0.373095452863232));
#40914=CARTESIAN_POINT('Ctrl Pts',(-0.0183637040244166,0.0950760034299082,
-0.37521174964478));
#40915=CARTESIAN_POINT('Ctrl Pts',(0.0130467125361599,0.101142850712012,
-0.377328046426329));
#40916=CARTESIAN_POINT('Ctrl Pts',(0.0477607628137719,0.0901055075652994,
-0.379444343207877));
#40917=CARTESIAN_POINT('Ctrl Pts',(0.0698998222648158,0.0670125876313357,
-0.381560639989425));
#40918=CARTESIAN_POINT('Ctrl Pts',(0.0920388817158606,0.043919667697371,
-0.383676936770974));
#40919=CARTESIAN_POINT('Ctrl Pts',(0.101602950340336,0.00877117097615361,
-0.385793233552523));
#40920=CARTESIAN_POINT('Ctrl Pts',(0.0942173080009238,-0.0223555569548012,
-0.387909530334071));
#40921=CARTESIAN_POINT('Ctrl Pts',(0.086831665661512,-0.0534822848857547,
-0.39002582711562));
#40922=CARTESIAN_POINT('Ctrl Pts',(0.0624963123582147,-0.0805872440264466,
-0.392142123897168));
#40923=CARTESIAN_POINT('Ctrl Pts',(0.0323425316822245,-0.0912722997304472,
-0.394258420678716));
#40924=CARTESIAN_POINT('Ctrl Pts',(0.00218875100623434,-0.101957355434448,
-0.396374717460265));
#40925=CARTESIAN_POINT('Ctrl Pts',(-0.0337834570424483,-0.0962225077017568,
-0.398491014241813));
#40926=CARTESIAN_POINT('Ctrl Pts',(-0.0591199714078947,-0.0766909449311324,
-0.400607311023361));
#40927=CARTESIAN_POINT('Ctrl Pts',(-0.0823422408155461,-0.0587892238786714,
-0.402547010119251));
#40928=CARTESIAN_POINT('Ctrl Pts',(-0.0966297808080416,-0.029297293541015,
-0.404486709215142));
#40929=CARTESIAN_POINT('Ctrl Pts',(-0.0968050622971842,4.68532484065691E-5,
-0.406426408311032));
#40930=CARTESIAN_POINT('Ctrl Pts',(-0.0967945983128168,5.43772629733152E-5,
-0.412223591688966));
#40931=CARTESIAN_POINT('Ctrl Pts',(-0.0966001788039178,-0.0287920307405604,
-0.410317337684812));
#40932=CARTESIAN_POINT('Ctrl Pts',(-0.0828630361045588,-0.057799150832469,
-0.408411083680658));
#40933=CARTESIAN_POINT('Ctrl Pts',(-0.0603212754475115,-0.0757496897480507,
-0.406504829676504));
#40934=CARTESIAN_POINT('Ctrl Pts',(-0.0352957251142473,-0.0956781293218542,
-0.404388532894955));
#40935=CARTESIAN_POINT('Ctrl Pts',(0.000581633718982209,-0.101979185837537,
-0.402272236113407));
#40936=CARTESIAN_POINT('Ctrl Pts',(0.0309000651693513,-0.0917706801820185,
-0.400155939331858));
#40937=CARTESIAN_POINT('Ctrl Pts',(0.0612184966197203,-0.0815621745265001,
-0.39803964255031));
#40938=CARTESIAN_POINT('Ctrl Pts',(0.0859780006872285,-0.0548441066997805,
-0.395923345768761));
#40939=CARTESIAN_POINT('Ctrl Pts',(0.0938532821144865,-0.0238376426032253,
-0.393807048987213));
#40940=CARTESIAN_POINT('Ctrl Pts',(0.101728563541744,0.00716882149332862,
-0.391690752205665));
#40941=CARTESIAN_POINT('Ctrl Pts',(0.0927196223287525,0.0424636818597185,
-0.389574455424117));
#40942=CARTESIAN_POINT('Ctrl Pts',(0.0709472566512509,0.0659026444249548,
-0.387458158642568));
#40943=CARTESIAN_POINT('Ctrl Pts',(0.0491748909737483,0.089341606990192,
-0.38534186186102));
#40944=CARTESIAN_POINT('Ctrl Pts',(0.0146391008317351,0.100924671754276,
-0.383225565079471));
#40945=CARTESIAN_POINT('Ctrl Pts',(-0.0168630275634053,0.0953536054375309,
-0.381109268297923));
#40946=CARTESIAN_POINT('Ctrl Pts',(-0.0483651559585449,0.0897825391207864,
-0.378992971516374));
#40947=CARTESIAN_POINT('Ctrl Pts',(-0.0768336226068113,0.0670573417232148,
-0.376876674734826));
#40948=CARTESIAN_POINT('Ctrl Pts',(-0.0892466081115938,0.0375727921389412,
-0.374760377953277));
#40949=CARTESIAN_POINT('Ctrl Pts',(-0.0942063868159446,0.0257918357300971,
-0.37391478253184));
#40950=CARTESIAN_POINT('Ctrl Pts',(-0.0966028891884939,0.0129317408436426,
-0.373069187110403));
#40951=CARTESIAN_POINT('Ctrl Pts',(-0.0965423984694297,5.0056945484775E-5,
-0.372223591688966));
#40952=CARTESIAN_POINT('Origin',(0.,0.,-0.593));
#40953=CARTESIAN_POINT('',(-0.0965988706096985,-7.90725476241677E-5,-0.326426408311032));
#40954=CARTESIAN_POINT('',(-0.0966122385588212,-8.24931776182297E-5,-0.332223591688966));
#40955=CARTESIAN_POINT('',(-0.096675,-1.1839272930757E-17,-0.593));
#40956=CARTESIAN_POINT('Ctrl Pts',(-0.0965988706096985,-7.90725476241677E-5,
-0.326426408311032));
#40957=CARTESIAN_POINT('Ctrl Pts',(-0.0964290112854852,0.0219426387689453,
-0.327874111284776));
#40958=CARTESIAN_POINT('Ctrl Pts',(-0.0889581327325248,0.0440685769717619,
-0.329321814258519));
#40959=CARTESIAN_POINT('Ctrl Pts',(-0.0751598805966252,0.0610546018118317,
-0.330769517232263));
#40960=CARTESIAN_POINT('Ctrl Pts',(-0.054989170778521,0.0858852959198736,
-0.332885814013812));
#40961=CARTESIAN_POINT('Ctrl Pts',(-0.0212971846766535,0.0997322559807113,
-0.33500211079536));
#40962=CARTESIAN_POINT('Ctrl Pts',(0.0105049576247015,0.0962617157493233,
-0.337118407576909));
#40963=CARTESIAN_POINT('Ctrl Pts',(0.0423070999260574,0.0927911755179352,
-0.339234704358457));
#40964=CARTESIAN_POINT('Ctrl Pts',(0.0722193984269001,0.0720031349943205,
-0.341351001140006));
#40965=CARTESIAN_POINT('Ctrl Pts',(0.0865596076579527,0.0434062941956763,
-0.343467297921554));
#40966=CARTESIAN_POINT('Ctrl Pts',(0.100899816889005,0.0148094533970324,
-0.345583594703102));
#40967=CARTESIAN_POINT('Ctrl Pts',(0.0996679368502675,-0.0215961876766415,
-0.347699891484651));
#40968=CARTESIAN_POINT('Ctrl Pts',(0.0834274443029201,-0.049158250485381,
-0.349816188266199));
#40969=CARTESIAN_POINT('Ctrl Pts',(0.0671869517555729,-0.07672031329412,
-0.351932485047748));
#40970=CARTESIAN_POINT('Ctrl Pts',(0.0359378466996168,-0.0954387978379257,
-0.354048781829296));
#40971=CARTESIAN_POINT('Ctrl Pts',(0.0039738460173819,-0.0967516439215915,
-0.356165078610845));
#40972=CARTESIAN_POINT('Ctrl Pts',(-0.027990154664854,-0.0980644900052573,
-0.358281375392393));
#40973=CARTESIAN_POINT('Ctrl Pts',(-0.0606690509733682,-0.0819716976287823,
-0.360397672173941));
#40974=CARTESIAN_POINT('Ctrl Pts',(-0.0791151222926576,-0.0558343037774998,
-0.36251396895549));
#40975=CARTESIAN_POINT('Ctrl Pts',(-0.0904823268696878,-0.0397273996093885,
-0.363818115407337));
#40976=CARTESIAN_POINT('Ctrl Pts',(-0.0964445937205749,-0.0198060421970087,
-0.365122261859184));
#40977=CARTESIAN_POINT('Ctrl Pts',(-0.0965509256710446,5.67507499378977E-5,
-0.366426408311032));
#40978=CARTESIAN_POINT('Ctrl Pts',(-0.0965423984694297,5.0056945484775E-5,
-0.372223591688966));
#40979=CARTESIAN_POINT('Ctrl Pts',(-0.0964514972688789,-0.0193076321277276,
-0.370952890328855));
#40980=CARTESIAN_POINT('Ctrl Pts',(-0.090812222688808,-0.0387140734331841,
-0.369682188968743));
#40981=CARTESIAN_POINT('Ctrl Pts',(-0.079985242555171,-0.0545805161383707,
-0.368411487608632));
#40982=CARTESIAN_POINT('Ctrl Pts',(-0.0619533871326681,-0.0810053730604315,
-0.366295190827084));
#40983=CARTESIAN_POINT('Ctrl Pts',(-0.0295321719263656,-0.0976111851335773,
-0.364178894045535));
#40984=CARTESIAN_POINT('Ctrl Pts',(0.00244854888678868,-0.096802253986617,
-0.362062597263987));
#40985=CARTESIAN_POINT('Ctrl Pts',(0.0344292696999425,-0.0959933228396567,
-0.359946300482439));
#40986=CARTESIAN_POINT('Ctrl Pts',(0.0659694961199474,-0.0777696484725894,
-0.35783000370089));
#40987=CARTESIAN_POINT('Ctrl Pts',(0.082642348847544,-0.0504669589484183,
-0.355713706919342));
#40988=CARTESIAN_POINT('Ctrl Pts',(0.0993152015751415,-0.0231642694242456,
-0.353597410137793));
#40989=CARTESIAN_POINT('Ctrl Pts',(0.101120680610329,0.0132174352570328,
-0.351481113356245));
#40990=CARTESIAN_POINT('Ctrl Pts',(0.0872329381049923,0.042036725349521,
-0.349364816574696));
#40991=CARTESIAN_POINT('Ctrl Pts',(0.0733451955996561,0.0708560154420084,
-0.347248519793148));
#40992=CARTESIAN_POINT('Ctrl Pts',(0.0437642315537964,0.0921128909457067,
-0.345132223011599));
#40993=CARTESIAN_POINT('Ctrl Pts',(0.0120207350678154,0.0960842010788969,
-0.343015926230051));
#40994=CARTESIAN_POINT('Ctrl Pts',(-0.0197227614181652,0.100055511212087,
-0.340899629448502));
#40995=CARTESIAN_POINT('Ctrl Pts',(-0.0536287903442663,0.0867412559747704,
-0.338783332666954));
#40996=CARTESIAN_POINT('Ctrl Pts',(-0.0741883258613981,0.0622315360120855,
-0.336667035885406));
#40997=CARTESIAN_POINT('Ctrl Pts',(-0.0885774779519113,0.0450777395196946,
-0.335185887819926));
#40998=CARTESIAN_POINT('Ctrl Pts',(-0.0964291408375652,0.0224400883890291,
-0.333704739754446));
#40999=CARTESIAN_POINT('Ctrl Pts',(-0.0966122385588212,-8.24931776182297E-5,
-0.332223591688966));
#41000=CARTESIAN_POINT('Origin',(0.,0.,-0.593));
#41001=CARTESIAN_POINT('',(-0.0968321016897829,-9.30107239267841E-6,-0.286426408311032));
#41002=CARTESIAN_POINT('',(-0.096833216074716,1.13968060647145E-7,-0.292223591688966));
#41003=CARTESIAN_POINT('',(-0.096675,-1.1839272930757E-17,-0.593));
#41004=CARTESIAN_POINT('Ctrl Pts',(-0.0968321016897829,-9.30107239267841E-6,
-0.286426408311032));
#41005=CARTESIAN_POINT('Ctrl Pts',(-0.0967888706163907,0.0314831625185701,
-0.288509663928818));
#41006=CARTESIAN_POINT('Ctrl Pts',(-0.0799841734743482,0.0630152174938467,
-0.290592919546605));
#41007=CARTESIAN_POINT('Ctrl Pts',(-0.0538006019224041,0.0805119077310139,
-0.292676175164392));
#41008=CARTESIAN_POINT('Ctrl Pts',(-0.0272017497548095,0.0982861016035854,
-0.29479247194594));
#41009=CARTESIAN_POINT('Ctrl Pts',(0.00907584055141718,0.101576188530772,
-0.296908768727489));
#41010=CARTESIAN_POINT('Ctrl Pts',(0.0384383624190365,0.0888772431404299,
-0.299025065509037));
#41011=CARTESIAN_POINT('Ctrl Pts',(0.0678008842866576,0.0761782977500875,
-0.301141362290586));
#41012=CARTESIAN_POINT('Ctrl Pts',(0.0902483377156704,0.0474903200422152,
-0.303257659072134));
#41013=CARTESIAN_POINT('Ctrl Pts',(0.0955129872471203,0.0159355364149357,
-0.305373955853682));
#41014=CARTESIAN_POINT('Ctrl Pts',(0.10077763677857,-0.015619247212342,
-0.307490252635231));
#41015=CARTESIAN_POINT('Ctrl Pts',(0.0888594824124587,-0.0500408367590265,
-0.30960654941678));
#41016=CARTESIAN_POINT('Ctrl Pts',(0.0652100314468056,-0.0715843827409785,
-0.311722846198328));
#41017=CARTESIAN_POINT('Ctrl Pts',(0.0415605804811526,-0.0931279287229305,
-0.313839142979876));
#41018=CARTESIAN_POINT('Ctrl Pts',(0.00617983291595768,-0.10179343114015,
-0.315955439761424));
#41019=CARTESIAN_POINT('Ctrl Pts',(-0.0247486313390017,-0.0936171848569828,
-0.318071736542973));
#41020=CARTESIAN_POINT('Ctrl Pts',(-0.055677095593962,-0.0854409385738153,
-0.320188033324521));
#41021=CARTESIAN_POINT('Ctrl Pts',(-0.0821532765386865,-0.0604229435902602,
-0.32230433010607));
#41022=CARTESIAN_POINT('Ctrl Pts',(-0.0920666502438785,-0.0300067320208591,
-0.324420626887618));
#41023=CARTESIAN_POINT('Ctrl Pts',(-0.0951985456999085,-0.0203974508985341,
-0.325089220695423));
#41024=CARTESIAN_POINT('Ctrl Pts',(-0.0966773168755601,-0.0102493768783783,
-0.325757814503227));
#41025=CARTESIAN_POINT('Ctrl Pts',(-0.0965988706096985,-7.90725476241677E-5,
-0.326426408311032));
#41026=CARTESIAN_POINT('Ctrl Pts',(-0.0966122385588212,-8.24931776182297E-5,
-0.332223591688966));
#41027=CARTESIAN_POINT('Ctrl Pts',(-0.0966907548701079,-0.00974066922227465,
-0.331588442972898));
#41028=CARTESIAN_POINT('Ctrl Pts',(-0.0953591124199333,-0.0193776853301763,
-0.330953294256829));
#41029=CARTESIAN_POINT('Ctrl Pts',(-0.0925281198827719,-0.028552036696178,
-0.33031814554076));
#41030=CARTESIAN_POINT('Ctrl Pts',(-0.0830953362788522,-0.0591207047537023,
-0.328201848759212));
#41031=CARTESIAN_POINT('Ctrl Pts',(-0.0570167269628521,-0.0845528561806965,
-0.326085551977664));
#41032=CARTESIAN_POINT('Ctrl Pts',(-0.0262209618144473,-0.0932155187190727,
-0.323969255196115));
#41033=CARTESIAN_POINT('Ctrl Pts',(0.00457480333395574,-0.101878181257448,
-0.321852958414567));
#41034=CARTESIAN_POINT('Ctrl Pts',(0.0400877243147619,-0.0937713549072077,
-0.319736661633018));
#41035=CARTESIAN_POINT('Ctrl Pts',(0.0640737635065671,-0.0726031996446781,
-0.31762036485147));
#41036=CARTESIAN_POINT('Ctrl Pts',(0.0880598026983737,-0.0514350443821474,
-0.315504068069922));
#41037=CARTESIAN_POINT('Ctrl Pts',(0.100518960101178,-0.017205560207324,
-0.313387771288373));
#41038=CARTESIAN_POINT('Ctrl Pts',(0.0957522671144628,0.0144282747056279,
-0.311271474506825));
#41039=CARTESIAN_POINT('Ctrl Pts',(0.0909855741277478,0.0460621096185807,
-0.309155177725276));
#41040=CARTESIAN_POINT('Ctrl Pts',(0.0689930307515148,0.0751002952696631,
-0.307038880943728));
#41041=CARTESIAN_POINT('Ctrl Pts',(0.0398342911095972,0.0882604159311316,
-0.304922584162179));
#41042=CARTESIAN_POINT('Ctrl Pts',(0.0106755514676821,0.101420536592599,
-0.302806287380631));
#41043=CARTESIAN_POINT('Ctrl Pts',(-0.0256493844399152,0.0987025922644553,
-0.300689990599082));
#41044=CARTESIAN_POINT('Ctrl Pts',(-0.0525250535878632,0.0813498034056174,
-0.298573693817534));
#41045=CARTESIAN_POINT('Ctrl Pts',(-0.0794058523729649,0.0639937024986232,
-0.296456993108011));
#41046=CARTESIAN_POINT('Ctrl Pts',(-0.0968337763961882,0.0319971699547993,
-0.294340292398489));
#41047=CARTESIAN_POINT('Ctrl Pts',(-0.096833216074716,1.13968060647145E-7,
-0.292223591688966));
#41048=CARTESIAN_POINT('Origin',(0.,0.,-0.593));
#41049=CARTESIAN_POINT('',(-0.0966258978973466,8.50958607245579E-5,-0.246426408311032));
#41050=CARTESIAN_POINT('',(-0.0966119077409059,8.24194000266483E-5,-0.252223591688966));
#41051=CARTESIAN_POINT('',(-0.096675,-1.1839272930757E-17,-0.593));
#41052=CARTESIAN_POINT('Ctrl Pts',(-0.0966258978973466,8.50958607245579E-5,
-0.246426408311032));
#41053=CARTESIAN_POINT('Ctrl Pts',(-0.0967035430033851,0.0092437051732415,
-0.247028919791313));
#41054=CARTESIAN_POINT('Ctrl Pts',(-0.0955076479844384,0.0183824419548729,
-0.247631431271594));
#41055=CARTESIAN_POINT('Ctrl Pts',(-0.0929562892575429,0.0271256399218355,
-0.248233942751875));
#41056=CARTESIAN_POINT('Ctrl Pts',(-0.0839947467160028,0.0578357630041277,
-0.250350239533423));
#41057=CARTESIAN_POINT('Ctrl Pts',(-0.0583103507134378,0.0836659784968148,
-0.252466536314972));
#41058=CARTESIAN_POINT('Ctrl Pts',(-0.0276514532137634,0.0928012348455942,
-0.25458283309652));
#41059=CARTESIAN_POINT('Ctrl Pts',(0.00300744428591197,0.101936491194374,
-0.256699129878069));
#41060=CARTESIAN_POINT('Ctrl Pts',(0.0386408432826971,0.0943767883992445,
-0.258815426659617));
#41061=CARTESIAN_POINT('Ctrl Pts',(0.0629495980601638,0.0735800255352227,
-0.260931723441166));
#41062=CARTESIAN_POINT('Ctrl Pts',(0.0872583528376278,0.0527832626712033,
-0.263048020222714));
#41063=CARTESIAN_POINT('Ctrl Pts',(0.100242463395776,0.0187494397382947,
-0.265164317004262));
#41064=CARTESIAN_POINT('Ctrl Pts',(0.0959628412405606,-0.0129539628970974,
-0.267280613785811));
#41065=CARTESIAN_POINT('Ctrl Pts',(0.0916832190853444,-0.044657365532493,
-0.269396910567359));
#41066=CARTESIAN_POINT('Ctrl Pts',(0.0701398642167597,-0.0740303478703715,
-0.271513207348908));
#41067=CARTESIAN_POINT('Ctrl Pts',(0.0411869665271511,-0.0876373541475984,
-0.273629504130456));
#41068=CARTESIAN_POINT('Ctrl Pts',(0.0122340688375434,-0.101244360424825,
-0.275745800912005));
#41069=CARTESIAN_POINT('Ctrl Pts',(-0.0241283716730878,-0.0990853906414008,
-0.277862097693553));
#41070=CARTESIAN_POINT('Ctrl Pts',(-0.0512677369224376,-0.0821479835696045,
-0.279978394475101));
#41071=CARTESIAN_POINT('Ctrl Pts',(-0.0784071021717868,-0.0652105764978087,
-0.28209469125665));
#41072=CARTESIAN_POINT('Ctrl Pts',(-0.0963233921598552,-0.0334947321376415,
-0.284210988038198));
#41073=CARTESIAN_POINT('Ctrl Pts',(-0.0968214801394086,-0.00150765954857932,
-0.286327284819747));
#41074=CARTESIAN_POINT('Ctrl Pts',(-0.0968292566510225,-0.00100825411882745,
-0.286360325983508));
#41075=CARTESIAN_POINT('Ctrl Pts',(-0.0968327873497487,-0.000508782575230481,
-0.28639336714727));
#41076=CARTESIAN_POINT('Ctrl Pts',(-0.0968321016897829,-9.30107239267841E-6,
-0.286426408311032));
#41077=CARTESIAN_POINT('Ctrl Pts',(-0.096833216074716,1.13968060647145E-7,
-0.292223591688966));
#41078=CARTESIAN_POINT('Ctrl Pts',(-0.096832655967095,-0.0319847300834253,
-0.290107698835392));
#41079=CARTESIAN_POINT('Ctrl Pts',(-0.0794199518304906,-0.0639700965998081,
-0.287991805981818));
#41080=CARTESIAN_POINT('Ctrl Pts',(-0.0525560190935891,-0.0813298015832744,
-0.285875913128243));
#41081=CARTESIAN_POINT('Ctrl Pts',(-0.0256869579807819,-0.0986928205674731,
-0.283759616346695));
#41082=CARTESIAN_POINT('Ctrl Pts',(0.0106369405918268,-0.10142459335248,
-0.281643319565147));
#41083=CARTESIAN_POINT('Ctrl Pts',(0.0398006880884165,-0.088275574176717,
-0.279527022783598));
#41084=CARTESIAN_POINT('Ctrl Pts',(0.0689644355850071,-0.0751265550009541,
-0.27741072600205));
#41085=CARTESIAN_POINT('Ctrl Pts',(0.0909680320055784,-0.0460967438644211,
-0.275294429220502));
#41086=CARTESIAN_POINT('Ctrl Pts',(0.0957467674307411,-0.0144647258910801,
-0.273178132438953));
#41087=CARTESIAN_POINT('Ctrl Pts',(0.100525502855904,0.0171672920822619,
-0.271061835657405));
#41088=CARTESIAN_POINT('Ctrl Pts',(0.0880793772856569,0.0514015168924121,
-0.268945538875856));
#41089=CARTESIAN_POINT('Ctrl Pts',(0.0641013984034045,0.0725788019415346,
-0.266829242094308));
#41090=CARTESIAN_POINT('Ctrl Pts',(0.0401234195211542,0.0937560869906552,
-0.264712945312759));
#41091=CARTESIAN_POINT('Ctrl Pts',(0.00461358732690071,0.101876432278751,
-0.262596648531211));
#41092=CARTESIAN_POINT('Ctrl Pts',(-0.0261854734061089,0.093225494104555,
-0.260480351749662));
#41093=CARTESIAN_POINT('Ctrl Pts',(-0.0569845341391203,0.0845745559303588,
-0.258364054968114));
#41094=CARTESIAN_POINT('Ctrl Pts',(-0.0830728234108873,0.0591523342938697,
-0.256247758186566));
#41095=CARTESIAN_POINT('Ctrl Pts',(-0.0925172436134204,0.0285872594474463,
-0.254131461405017));
#41096=CARTESIAN_POINT('Ctrl Pts',(-0.0953553337853935,0.0194023188510939,
-0.253495504833));
#41097=CARTESIAN_POINT('Ctrl Pts',(-0.096690434039967,0.00975296361118441,
-0.252859548260983));
#41098=CARTESIAN_POINT('Ctrl Pts',(-0.0966119077409059,8.24194000266483E-5,
-0.252223591688966));
#41099=CARTESIAN_POINT('Origin',(0.,0.,-0.593));
#41100=CARTESIAN_POINT('',(-0.0965351754675536,-4.30991072692052E-5,-0.206426408311032));
#41101=CARTESIAN_POINT('',(-0.0965425912303032,-5.0224085100017E-5,-0.212223591688966));
#41102=CARTESIAN_POINT('',(-0.096675,-1.1839272930757E-17,-0.593));
#41103=CARTESIAN_POINT('Ctrl Pts',(-0.0965351754675536,-4.30991072692052E-5,
-0.206426408311032));
#41104=CARTESIAN_POINT('Ctrl Pts',(-0.0964592547998338,0.018820931113738,
-0.207664472435356));
#41105=CARTESIAN_POINT('Ctrl Pts',(-0.0911250957801962,0.0377246133573255,
-0.20890253655968));
#41106=CARTESIAN_POINT('Ctrl Pts',(-0.0808151957183313,0.0533439424371889,
-0.210140600684003));
#41107=CARTESIAN_POINT('Ctrl Pts',(-0.0631918691956234,0.0800429923589462,
-0.212256897465552));
#41108=CARTESIAN_POINT('Ctrl Pts',(-0.03102987416261,0.0971454572669495,
-0.2143731942471));
#41109=CARTESIAN_POINT('Ctrl Pts',(0.000959505631360331,0.0968284638039782,
-0.216489491028648));
#41110=CARTESIAN_POINT('Ctrl Pts',(0.0329488854253307,0.0965114703410068,
-0.218605787810197));
#41111=CARTESIAN_POINT('Ctrl Pts',(0.0647656499802579,0.078775018507061,
-0.220722084591745));
#41112=CARTESIAN_POINT('Ctrl Pts',(0.0818564281248476,0.0517319749123845,
-0.222838381373294));
#41113=CARTESIAN_POINT('Ctrl Pts',(0.0989472062694382,0.0246889313177066,
-0.224954678154842));
#41114=CARTESIAN_POINT('Ctrl Pts',(0.101311998003689,-0.0116607040377033,
-0.227070974936391));
#41115=CARTESIAN_POINT('Ctrl Pts',(0.0878691191168146,-0.0406901703036554,
-0.229187271717939));
#41116=CARTESIAN_POINT('Ctrl Pts',(0.0744262402299409,-0.0697196365696058,
-0.231303568499488));
#41117=CARTESIAN_POINT('Ctrl Pts',(0.0451756907219436,-0.0914289337460994,
-0.233419865281036));
#41118=CARTESIAN_POINT('Ctrl Pts',(0.0134970241056018,-0.0958879679312891,
-0.235536162062584));
#41119=CARTESIAN_POINT('Ctrl Pts',(-0.0181816425107408,-0.100347002116479,
-0.237652458844133));
#41120=CARTESIAN_POINT('Ctrl Pts',(-0.0522884262354281,-0.0875557733103637,
-0.239768755625681));
#41121=CARTESIAN_POINT('Ctrl Pts',(-0.0732224735575136,-0.0633651435713575,
-0.24188505240723));
#41122=CARTESIAN_POINT('Ctrl Pts',(-0.0881965799345135,-0.0460616065407357,
-0.243398837708497));
#41123=CARTESIAN_POINT('Ctrl Pts',(-0.0964308177634683,-0.0229255331664144,
-0.244912623009765));
#41124=CARTESIAN_POINT('Ctrl Pts',(-0.0966258978973466,8.50958607245579E-5,
-0.246426408311032));
#41125=CARTESIAN_POINT('Ctrl Pts',(-0.0966119077409059,8.24194000266483E-5,
-0.252223591688966));
#41126=CARTESIAN_POINT('Ctrl Pts',(-0.0964291190991639,-0.0224280727840927,
-0.250743251479435));
#41127=CARTESIAN_POINT('Ctrl Pts',(-0.0885867876710175,-0.0450533745206066,
-0.249262911269903));
#41128=CARTESIAN_POINT('Ctrl Pts',(-0.0742120116041304,-0.0622032885160329,
-0.247782571060372));
#41129=CARTESIAN_POINT('Ctrl Pts',(-0.0536618082590074,-0.0867208335767331,
-0.245666274278824));
#41130=CARTESIAN_POINT('Ctrl Pts',(-0.019760850435462,-0.100047995641777,
-0.243549977497275));
#41131=CARTESIAN_POINT('Ctrl Pts',(0.011984155600785,-0.0960887703276321,
-0.241433680715727));
#41132=CARTESIAN_POINT('Ctrl Pts',(0.043729161637033,-0.0921295450134873,
-0.239317383934178));
#41133=CARTESIAN_POINT('Ctrl Pts',(0.0733182158859835,-0.0708839323201507,
-0.23720108715263));
#41134=CARTESIAN_POINT('Ctrl Pts',(0.0872169286909223,-0.0420699312842774,
-0.235084790371081));
#41135=CARTESIAN_POINT('Ctrl Pts',(0.101115641495861,-0.0132559302484049,
-0.232968493589533));
#41136=CARTESIAN_POINT('Ctrl Pts',(0.0993240128567908,0.0231264591300049,
-0.230852196807985));
#41137=CARTESIAN_POINT('Ctrl Pts',(0.0826615552839103,0.050435493916336,
-0.228735900026436));
#41138=CARTESIAN_POINT('Ctrl Pts',(0.0659990977110294,0.0777445287026677,
-0.226619603244888));
#41139=CARTESIAN_POINT('Ctrl Pts',(0.0344658112043376,0.0959802088969194,
-0.224503306463339));
#41140=CARTESIAN_POINT('Ctrl Pts',(0.00248540066314722,0.0968013148262096,
-0.222387009681791));
#41141=CARTESIAN_POINT('Ctrl Pts',(-0.0294950098780432,0.0976224207554999,
-0.220270712900242));
#41142=CARTESIAN_POINT('Ctrl Pts',(-0.0619225444537312,0.0810289524198287,
-0.218154416118694));
#41143=CARTESIAN_POINT('Ctrl Pts',(-0.079964458331246,0.0546109620162111,
-0.216038119337145));
#41144=CARTESIAN_POINT('Ctrl Pts',(-0.0908043650828087,0.0387385576536239,
-0.214766610121085));
#41145=CARTESIAN_POINT('Ctrl Pts',(-0.096451317698328,0.0193196749306095,
-0.213495100905026));
#41146=CARTESIAN_POINT('Ctrl Pts',(-0.0965425912303032,-5.0224085100017E-5,
-0.212223591688966));
#41147=CARTESIAN_POINT('Origin',(0.,0.,-0.593));
#41148=CARTESIAN_POINT('',(-0.0967832346277187,-6.11107174333103E-5,-0.166426408311032));
#41149=CARTESIAN_POINT('',(-0.0967948658423725,-5.42027044862851E-5,-0.172223591688967));
#41150=CARTESIAN_POINT('',(-0.096675,-1.1839272930757E-17,-0.593));
#41151=CARTESIAN_POINT('Ctrl Pts',(-0.0967832346277187,-6.11107174333103E-5,
-0.166426408311032));
#41152=CARTESIAN_POINT('Ctrl Pts',(-0.0965738675467705,0.0283001656582659,
-0.168300025079399));
#41153=CARTESIAN_POINT('Ctrl Pts',(-0.0833609810550404,0.0568311707808718,
-0.170173641847765));
#41154=CARTESIAN_POINT('Ctrl Pts',(-0.0614791216390247,0.0748130313352698,
-0.172047258616132));
#41155=CARTESIAN_POINT('Ctrl Pts',(-0.0367630167032322,0.0951239904705796,
-0.17416355539768));
#41156=CARTESIAN_POINT('Ctrl Pts',(-0.000986806504219694,0.101976071561127,
-0.176279852179229));
#41157=CARTESIAN_POINT('Ctrl Pts',(0.0294850396506297,0.09223505022771,
-0.178396148960777));
#41158=CARTESIAN_POINT('Ctrl Pts',(0.0599568858054783,0.0824940288942931,
-0.180512445742326));
#41159=CARTESIAN_POINT('Ctrl Pts',(0.085124367916164,0.0561599051369124,
-0.182628742523874));
#41160=CARTESIAN_POINT('Ctrl Pts',(0.0934755766709938,0.0252782242125185,
-0.184745039305422));
#41161=CARTESIAN_POINT('Ctrl Pts',(0.101826785425824,-0.00560345671187625,
-0.186861336086971));
#41162=CARTESIAN_POINT('Ctrl Pts',(0.0933617208247971,-0.0410326948032845,
-0.188977632868519));
#41163=CARTESIAN_POINT('Ctrl Pts',(0.0719524053255447,-0.0648037299990389,
-0.191093929650068));
#41164=CARTESIAN_POINT('Ctrl Pts',(0.0505430898262929,-0.0885747651947925,
-0.193210226431616));
#41165=CARTESIAN_POINT('Ctrl Pts',(0.0161895234288162,-0.100687597494893,
-0.195326523213164));
#41166=CARTESIAN_POINT('Ctrl Pts',(-0.015394558986119,-0.0956016715717106,
-0.197442819994713));
#41167=CARTESIAN_POINT('Ctrl Pts',(-0.0469786414010552,-0.0905157456485279,
-0.199559116776261));
#41168=CARTESIAN_POINT('Ctrl Pts',(-0.0757932398334497,-0.0682310615020615,
-0.20167541355781));
#41169=CARTESIAN_POINT('Ctrl Pts',(-0.0886582100434459,-0.0389409019610718,
-0.203791710339358));
#41170=CARTESIAN_POINT('Ctrl Pts',(-0.0939969872277939,-0.026785907978898,
-0.204669942996583));
#41171=CARTESIAN_POINT('Ctrl Pts',(-0.0965890305211326,-0.0134244798140298,
-0.205548175653807));
#41172=CARTESIAN_POINT('Ctrl Pts',(-0.0965351754675536,-4.30991072692052E-5,
-0.206426408311032));
#41173=CARTESIAN_POINT('Ctrl Pts',(-0.0965425912303032,-5.0224085100017E-5,
-0.212223591688966));
#41174=CARTESIAN_POINT('Ctrl Pts',(-0.0966032331382791,-0.0129195368879978,
-0.211378804123477));
#41175=CARTESIAN_POINT('Ctrl Pts',(-0.0942114646287571,-0.0257672271039402,
-0.210534016557989));
#41176=CARTESIAN_POINT('Ctrl Pts',(-0.0892609053485345,-0.0375388138450597,
-0.2096892289925));
#41177=CARTESIAN_POINT('Ctrl Pts',(-0.0768591453089668,-0.0670280868311531,
-0.207572932210952));
#41178=CARTESIAN_POINT('Ctrl Pts',(-0.0483993320504909,-0.0897641203317749,
-0.205456635429404));
#41179=CARTESIAN_POINT('Ctrl Pts',(-0.0168993268047482,-0.0953471788889501,
-0.203340338647855));
#41180=CARTESIAN_POINT('Ctrl Pts',(0.0146006784409936,-0.100930237446125,
-0.201224041866307));
#41181=CARTESIAN_POINT('Ctrl Pts',(0.049140875674001,-0.0893603210598525,
-0.199107745084758));
#41182=CARTESIAN_POINT('Ctrl Pts',(0.0709221628258518,-0.0659296487832139,
-0.19699144830321));
#41183=CARTESIAN_POINT('Ctrl Pts',(0.0927034499777021,-0.0424989765065759,
-0.194875151521661));
#41184=CARTESIAN_POINT('Ctrl Pts',(0.101725827048397,-0.00720754833957142,
-0.192758854740113));
#41185=CARTESIAN_POINT('Ctrl Pts',(0.093862350140176,0.0238019115755997,
-0.190642557958565));
#41186=CARTESIAN_POINT('Ctrl Pts',(0.0859988732319544,0.0548113714907725,
-0.188526261177016));
#41187=CARTESIAN_POINT('Ctrl Pts',(0.0612495423448144,0.0815388631541128,
-0.186409964395468));
#41188=CARTESIAN_POINT('Ctrl Pts',(0.0309349993989626,0.0917589100889316,
-0.184293667613919));
#41189=CARTESIAN_POINT('Ctrl Pts',(0.000620456453112605,0.10197895702375,
-0.182177370832371));
#41190=CARTESIAN_POINT('Ctrl Pts',(-0.0352592985514467,0.0956915592300501,
-0.180061074050823));
#41191=CARTESIAN_POINT('Ctrl Pts',(-0.0602924336904824,0.075772648155117,
-0.177944777269274));
#41192=CARTESIAN_POINT('Ctrl Pts',(-0.0828505822822485,0.0578230883689023,
-0.176037715409172));
#41193=CARTESIAN_POINT('Ctrl Pts',(-0.0966008620437373,0.0288042201319593,
-0.174130653549069));
#41194=CARTESIAN_POINT('Ctrl Pts',(-0.0967948658423725,-5.42027044862851E-5,
-0.172223591688967));
#41195=CARTESIAN_POINT('Origin',(0.,0.,-0.593));
#41196=CARTESIAN_POINT('',(-0.0967207250391251,8.29397659327311E-5,-0.126426408311032));
#41197=CARTESIAN_POINT('',(-0.0967054797063448,8.55434351395205E-5,-0.132223591688966));
#41198=CARTESIAN_POINT('',(-0.096675,-1.1839272930757E-17,-0.593));
#41199=CARTESIAN_POINT('Ctrl Pts',(-0.0967207250391251,8.29397659327311E-5,
-0.126426408311032));
#41200=CARTESIAN_POINT('Ctrl Pts',(-0.0967748071718798,0.0060399254137226,
-0.126819280941893));
#41201=CARTESIAN_POINT('Ctrl Pts',(-0.0962716703858991,0.0119878001314283,
-0.127212153572754));
#41202=CARTESIAN_POINT('Ctrl Pts',(-0.0951784404822581,0.0178251613315098,
-0.127605026203615));
#41203=CARTESIAN_POINT('Ctrl Pts',(-0.0892895117434499,0.0492694202339371,
-0.129721322985163));
#41204=CARTESIAN_POINT('Ctrl Pts',(-0.0662779660166628,0.0775069299341794,
-0.131837619766712));
#41205=CARTESIAN_POINT('Ctrl Pts',(-0.0366695589289991,0.0896215127660818,
-0.13395391654826));
#41206=CARTESIAN_POINT('Ctrl Pts',(-0.00706115184133365,0.101736095597985,
-0.136070213329808));
#41207=CARTESIAN_POINT('Ctrl Pts',(0.0291441166072093,0.0977277515615458,
-0.138186510111357));
#41208=CARTESIAN_POINT('Ctrl Pts',(0.055385519441118,0.0794299458780596,
-0.140302806892906));
#41209=CARTESIAN_POINT('Ctrl Pts',(0.0816269222750259,0.0611321401945739,
-0.142419103674454));
#41210=CARTESIAN_POINT('Ctrl Pts',(0.0979044594943001,0.028544872864042,
-0.144535400456002));
#41211=CARTESIAN_POINT('Ctrl Pts',(0.0967725902766724,-0.00342604790653714,
-0.146651697237551));
#41212=CARTESIAN_POINT('Ctrl Pts',(0.0956407210590447,-0.0353969686771154,
-0.148767994019099));
#41213=CARTESIAN_POINT('Ctrl Pts',(0.0770994454045165,-0.0667515428877409,
-0.150884290800648));
#41214=CARTESIAN_POINT('Ctrl Pts',(0.0496297656710845,-0.0831478106837788,
-0.153000587582196));
#41215=CARTESIAN_POINT('Ctrl Pts',(0.0221600859376509,-0.0995440784798177,
-0.155116884363744));
#41216=CARTESIAN_POINT('Ctrl Pts',(-0.0142379978746874,-0.100982039861267,
-0.157233181145293));
#41217=CARTESIAN_POINT('Ctrl Pts',(-0.0429155638196797,-0.0868039540382351,
-0.159349477926842));
#41218=CARTESIAN_POINT('Ctrl Pts',(-0.0715931297646696,-0.0726258682152039,
-0.16146577470839));
#41219=CARTESIAN_POINT('Ctrl Pts',(-0.0925501778423148,-0.0428317351876939,
-0.163582071489938));
#41220=CARTESIAN_POINT('Ctrl Pts',(-0.0962007020448521,-0.0110497500839039,
-0.165698368271487));
#41221=CARTESIAN_POINT('Ctrl Pts',(-0.0966193150056223,-0.00740524585785208,
-0.165941048284668));
#41222=CARTESIAN_POINT('Ctrl Pts',(-0.0968103528766703,-0.00373460203161953,
-0.16618372829785));
#41223=CARTESIAN_POINT('Ctrl Pts',(-0.0967832346277187,-6.11107174333103E-5,
-0.166426408311032));
#41224=CARTESIAN_POINT('Ctrl Pts',(-0.0967948658423725,-5.42027044862851E-5,
-0.172223591688967));
#41225=CARTESIAN_POINT('Ctrl Pts',(-0.0968161511349039,-0.00322042922370149,
-0.172014356767521));
#41226=CARTESIAN_POINT('Ctrl Pts',(-0.096674251824014,-0.00638472437038313,
-0.171805121846075));
#41227=CARTESIAN_POINT('Ctrl Pts',(-0.0963628966307718,-0.00953225687232562,
-0.171595886924629));
#41228=CARTESIAN_POINT('Ctrl Pts',(-0.093213709158514,-0.0413678264686656,
-0.16947959014308));
#41229=CARTESIAN_POINT('Ctrl Pts',(-0.0727288189404871,-0.0714885413051794,
-0.167363293361532));
#41230=CARTESIAN_POINT('Ctrl Pts',(-0.0442782613806259,-0.0861168237782632,
-0.165246996579984));
#41231=CARTESIAN_POINT('Ctrl Pts',(-0.0158277038207638,-0.100745106251347,
-0.163130699798435));
#41232=CARTESIAN_POINT('Ctrl Pts',(0.0205885210809334,-0.099880956361003,
-0.161014403016887));
#41233=CARTESIAN_POINT('Ctrl Pts',(0.0483131935882508,-0.0839196466581255,
-0.158898106235338));
#41234=CARTESIAN_POINT('Ctrl Pts',(0.0760378660955673,-0.0679583369552484,
-0.15678180945379));
#41235=CARTESIAN_POINT('Ctrl Pts',(0.0950709862085039,-0.0368998674398402,
-0.154665512672241));
#41236=CARTESIAN_POINT('Ctrl Pts',(0.0967065756835142,-0.00495075602753841,
-0.152549215890693));
#41237=CARTESIAN_POINT('Ctrl Pts',(0.0983421651585245,0.0269983553847643,
-0.150432919109144));
#41238=CARTESIAN_POINT('Ctrl Pts',(0.0825802239956075,0.0598381086939593,
-0.148316622327596));
#41239=CARTESIAN_POINT('Ctrl Pts',(0.0566304537585547,0.078547205402699,
-0.146200325546048));
#41240=CARTESIAN_POINT('Ctrl Pts',(0.0306806835215034,0.0972563021114377,
-0.144084028764499));
#41241=CARTESIAN_POINT('Ctrl Pts',(-0.00545691578968455,0.101834742219722,
-0.141967731982951));
#41242=CARTESIAN_POINT('Ctrl Pts',(-0.0352525709877608,0.0901882920099803,
-0.139851435201403));
#41243=CARTESIAN_POINT('Ctrl Pts',(-0.0650482261858388,0.0785418418002379,
-0.137735138419854));
#41244=CARTESIAN_POINT('Ctrl Pts',(-0.0885019372708057,0.0506705012724692,
-0.135618841638306));
#41245=CARTESIAN_POINT('Ctrl Pts',(-0.0948856947517297,0.0193229573153638,
-0.133502544856757));
#41246=CARTESIAN_POINT('Ctrl Pts',(-0.0961716717350178,0.0130081466208925,
-0.13307622713416));
#41247=CARTESIAN_POINT('Ctrl Pts',(-0.0967649474668955,0.00655227107519142,
-0.132649909411563));
#41248=CARTESIAN_POINT('Ctrl Pts',(-0.0967054797063448,8.55434351395205E-5,
-0.132223591688966));
#41249=CARTESIAN_POINT('Origin',(0.,0.,-0.593));
#41250=CARTESIAN_POINT('',(-0.0965170586776495,7.4335118630045E-6,-0.0864264083110323));
#41251=CARTESIAN_POINT('',(-0.096516496468341,-9.27006410983469E-7,-0.0922235916889666));
#41252=CARTESIAN_POINT('',(-0.096675,-1.1839272930757E-17,-0.593));
#41253=CARTESIAN_POINT('Ctrl Pts',(-0.0965170586776495,7.4335118630045E-6,
-0.0864264083110323));
#41254=CARTESIAN_POINT('Ctrl Pts',(-0.0965277726618348,0.0156846135208846,
-0.087454833585936));
#41255=CARTESIAN_POINT('Ctrl Pts',(-0.0929251385372256,0.0313571364771244,
-0.0884832588608397));
#41256=CARTESIAN_POINT('Ctrl Pts',(-0.0856824059907095,0.0451130878663906,
-0.0895116841357433));
#41257=CARTESIAN_POINT('Ctrl Pts',(-0.0707782880622152,0.0734201281177776,
-0.0916279809172917));
#41258=CARTESIAN_POINT('Ctrl Pts',(-0.0404599773489722,0.093611342862549,
-0.0937442776988399));
#41259=CARTESIAN_POINT('Ctrl Pts',(-0.00859532061802182,0.0964509920919599,
-0.0958605744803884));
#41260=CARTESIAN_POINT('Ctrl Pts',(0.0232693361129286,0.0992906413213708,
-0.0979768712619368));
#41261=CARTESIAN_POINT('Ctrl Pts',(0.056680338861587,0.0847787250354175,
-0.100093168043486));
#41262=CARTESIAN_POINT('Ctrl Pts',(0.0763550328277099,0.0595531870686323,
-0.102209464825034));
#41263=CARTESIAN_POINT('Ctrl Pts',(0.0960297267938328,0.034327649101847,
-0.104325761606582));
#41264=CARTESIAN_POINT('Ctrl Pts',(0.101968111977424,-0.00161151054576864,
-0.106442058388131));
#41265=CARTESIAN_POINT('Ctrl Pts',(0.0914539310741352,-0.031825297365229,
-0.108558355169679));
#41266=CARTESIAN_POINT('Ctrl Pts',(0.0809397501708469,-0.0620390841846885,
-0.110674651951227));
#41267=CARTESIAN_POINT('Ctrl Pts',(0.0539730031806786,-0.0865274981759914,
-0.112790948732776));
#41268=CARTESIAN_POINT('Ctrl Pts',(0.0228885882000559,-0.0940892387737843,
-0.114907245514324));
#41269=CARTESIAN_POINT('Ctrl Pts',(-0.0081958267805677,-0.101650979371577,
-0.117023542295873));
#41270=CARTESIAN_POINT('Ctrl Pts',(-0.0433979097516469,-0.0922860465758598,
-0.119139839077421));
#41271=CARTESIAN_POINT('Ctrl Pts',(-0.0666157953617716,-0.0702780761256944,
-0.12125613585897));
#41272=CARTESIAN_POINT('Ctrl Pts',(-0.0855234765231589,-0.0523556995894131,
-0.122979560009657));
#41273=CARTESIAN_POINT('Ctrl Pts',(-0.0964834816009508,-0.0260487174793249,
-0.124702984160345));
#41274=CARTESIAN_POINT('Ctrl Pts',(-0.0967207250391251,8.29397659327311E-5,
-0.126426408311032));
#41275=CARTESIAN_POINT('Ctrl Pts',(-0.0967054797063448,8.55434351395205E-5,
-0.132223591688966));
#41276=CARTESIAN_POINT('Ctrl Pts',(-0.0964697417468685,-0.0255494084150007,
-0.130533612630015));
#41277=CARTESIAN_POINT('Ctrl Pts',(-0.0859765770751443,-0.0513548936580699,
-0.128843633571063));
#41278=CARTESIAN_POINT('Ctrl Pts',(-0.0677151005125275,-0.0692194838422052,
-0.127153654512112));
#41279=CARTESIAN_POINT('Ctrl Pts',(-0.0448469449155209,-0.0915906336562278,
-0.125037357730563));
#41280=CARTESIAN_POINT('Ctrl Pts',(-0.00979682984462658,-0.101509185897832,
-0.122921060949015));
#41281=CARTESIAN_POINT('Ctrl Pts',(0.021402898869499,-0.0944382747481939,
-0.120804764167466));
#41282=CARTESIAN_POINT('Ctrl Pts',(0.0526026275836238,-0.087367363598556,
-0.118688467385918));
#41283=CARTESIAN_POINT('Ctrl Pts',(0.0799519699409812,-0.0633069890576768,
-0.11657217060437));
#41284=CARTESIAN_POINT('Ctrl Pts',(0.0909410097538229,-0.0332626572716202,
-0.114455873822821));
#41285=CARTESIAN_POINT('Ctrl Pts',(0.101930049566665,-0.00321832548556278,
-0.112339577041273));
#41286=CARTESIAN_POINT('Ctrl Pts',(0.0965587868349915,0.0328099635456709,
-0.110223280259724));
#41287=CARTESIAN_POINT('Ctrl Pts',(0.0772840974685356,0.0583424388332644,
-0.108106983478176));
#41288=CARTESIAN_POINT('Ctrl Pts',(0.0580094081020797,0.0838749141208579,
-0.105990686696628));
#41289=CARTESIAN_POINT('Ctrl Pts',(0.0248312921008405,0.0989115756648094,
-0.103874389915079));
#41290=CARTESIAN_POINT('Ctrl Pts',(-0.00707417260600754,0.0965744692966754,
-0.101758093133531));
#41291=CARTESIAN_POINT('Ctrl Pts',(-0.0389796373128547,0.0942373629285415,
-0.0996417963519824));
#41292=CARTESIAN_POINT('Ctrl Pts',(-0.0696124507253119,0.0745264886483231,
-0.0975254995704338));
#41293=CARTESIAN_POINT('Ctrl Pts',(-0.084960810759801,0.0464578455188266,
-0.0954092027888854));
#41294=CARTESIAN_POINT('Ctrl Pts',(-0.0926619842621373,0.0323741590383376,
-0.0943473324222458));
#41295=CARTESIAN_POINT('Ctrl Pts',(-0.0965151160525341,0.0161863055094454,
-0.0932854620556062));
#41296=CARTESIAN_POINT('Ctrl Pts',(-0.0965165097454088,-9.26928760177416E-7,
-0.0922235916889666));
#41297=CARTESIAN_POINT('Origin',(0.,0.,-0.593));
#41298=CARTESIAN_POINT('',(-0.0966970977580488,-8.58596968723868E-5,-0.0464264083110326));
#41299=CARTESIAN_POINT('',(-0.0967093838725941,-8.47898118814712E-5,-0.0522235916889671));
#41300=CARTESIAN_POINT('',(-0.096675,-1.1839272930757E-17,-0.593));
#41301=CARTESIAN_POINT('Ctrl Pts',(-0.0966970977580488,-8.58596968723868E-5,
-0.0464264083110326));
#41302=CARTESIAN_POINT('Ctrl Pts',(-0.096463819312519,0.0251626158010124,
-0.048090386229979));
#41303=CARTESIAN_POINT('Ctrl Pts',(-0.0863212822535982,0.0505757410207625,
-0.0497543641489254));
#41304=CARTESIAN_POINT('Ctrl Pts',(-0.0685565717469939,0.0683841308472504,
-0.0514183420678718));
#41305=CARTESIAN_POINT('Ctrl Pts',(-0.0459628827068936,0.0910333725500618,
-0.0535346388494203));
#41306=CARTESIAN_POINT('Ctrl Pts',(-0.0110399381729231,0.101381565704142,
-0.0556509356309688));
#41307=CARTESIAN_POINT('Ctrl Pts',(0.0202433730968924,0.0946936795329476,
-0.0577672324125173));
#41308=CARTESIAN_POINT('Ctrl Pts',(0.0515266843667053,0.0880057933617542,
-0.0598835291940656));
#41309=CARTESIAN_POINT('Ctrl Pts',(0.0791703623723638,0.06428182786529,
-0.061999825975614));
#41310=CARTESIAN_POINT('Ctrl Pts',(0.0905270688129109,0.0343742764785263,
-0.0641161227571623));
#41311=CARTESIAN_POINT('Ctrl Pts',(0.101883775253459,0.00446672509176077,
-0.0662324195387107));
#41312=CARTESIAN_POINT('Ctrl Pts',(0.0969535101288935,-0.031624412185305,
-0.0683487163202591));
#41313=CARTESIAN_POINT('Ctrl Pts',(0.0779929056047911,-0.0573910712254237,
-0.0704650131018076));
#41314=CARTESIAN_POINT('Ctrl Pts',(0.0590323010806893,-0.0831577302655415,
-0.072581309883356));
#41315=CARTESIAN_POINT('Ctrl Pts',(0.0260413571570511,-0.0985999110687128,
-0.0746976066649044));
#41316=CARTESIAN_POINT('Ctrl Pts',(-0.00589024604478475,-0.0966539334751514,
-0.0768139034464528));
#41317=CARTESIAN_POINT('Ctrl Pts',(-0.0378218492466215,-0.09470795588159,
-0.0789302002280012));
#41318=CARTESIAN_POINT('Ctrl Pts',(-0.068694111726656,-0.0753738198912948,
-0.0810464970095495));
#41319=CARTESIAN_POINT('Ctrl Pts',(-0.0843852803948016,-0.0474953190171464,
-0.0831627937910979));
#41320=CARTESIAN_POINT('Ctrl Pts',(-0.0924512451729286,-0.0331645186240334,
-0.0842506652977427));
#41321=CARTESIAN_POINT('Ctrl Pts',(-0.0965057253913115,-0.0165759370572375,
-0.0853385368043875));
#41322=CARTESIAN_POINT('Ctrl Pts',(-0.0965170586776495,7.4335118630045E-6,
-0.0864264083110323));
#41323=CARTESIAN_POINT('Ctrl Pts',(-0.0965165097454088,-9.26928760177416E-7,
-0.0922235916889666));
#41324=CARTESIAN_POINT('Ctrl Pts',(-0.096517893668181,-0.0160746832019732,
-0.0911691652740578));
#41325=CARTESIAN_POINT('Ctrl Pts',(-0.0927213533189873,-0.0321478270619503,
-0.090114738859149));
#41326=CARTESIAN_POINT('Ctrl Pts',(-0.0851232695060613,-0.0461595259106198,
-0.0890603124442402));
#41327=CARTESIAN_POINT('Ctrl Pts',(-0.0698734615613114,-0.0742818422317921,
-0.0869440156626918));
#41328=CARTESIAN_POINT('Ctrl Pts',(-0.0393099390152905,-0.0941000628953607,
-0.0848277188811432));
#41329=CARTESIAN_POINT('Ctrl Pts',(-0.00741288109560678,-0.0965490669160594,
-0.0827114220995947));
#41330=CARTESIAN_POINT('Ctrl Pts',(0.0244841768240779,-0.0989980709367582,
-0.0805951253180463));
#41331=CARTESIAN_POINT('Ctrl Pts',(0.0577147701174238,-0.0840778583145879,
-0.0784788285364981));
#41332=CARTESIAN_POINT('Ctrl Pts',(0.0770789316037844,-0.0586131675103347,
-0.0763625317549496));
#41333=CARTESIAN_POINT('Ctrl Pts',(0.0964430930901439,-0.033148476706083,
-0.0742462349734013));
#41334=CARTESIAN_POINT('Ctrl Pts',(0.101940822769517,0.00286069228024984,
-0.0721299381918529));
#41335=CARTESIAN_POINT('Ctrl Pts',(0.0910571913412267,0.0329434136143151,
-0.0700136414103045));
#41336=CARTESIAN_POINT('Ctrl Pts',(0.0801735599129361,0.0630261349483812,
-0.0678973446287561));
#41337=CARTESIAN_POINT('Ctrl Pts',(0.0529085673769804,0.0871824086301804,
-0.0657810478472076));
#41338=CARTESIAN_POINT('Ctrl Pts',(0.0217339318258845,0.0943626715618018,
-0.0636647510656592));
#41339=CARTESIAN_POINT('Ctrl Pts',(-0.00944070372521155,0.101542934493423,
-0.0615484542841107));
#41340=CARTESIAN_POINT('Ctrl Pts',(-0.0445249822914489,0.0917471866748669,
-0.0594321575025622));
#41341=CARTESIAN_POINT('Ctrl Pts',(-0.0674716573729478,0.0694564865140366,
-0.0573158607210138));
#41342=CARTESIAN_POINT('Ctrl Pts',(-0.085876549655346,0.0515777335399252,
-0.0556184377103316));
#41343=CARTESIAN_POINT('Ctrl Pts',(-0.0964730793250058,0.0256607282996191,
-0.0539210146996493));
#41344=CARTESIAN_POINT('Ctrl Pts',(-0.0967093838725941,-8.47898118814713E-5,
-0.0522235916889671));
#41345=CARTESIAN_POINT('Origin',(0.,0.,-1.25327725593024));
#41346=CARTESIAN_POINT('',(-0.0739168918988343,-6.56325999296408E-5,-0.0332772559302393));
#41347=CARTESIAN_POINT('',(-0.0739977701941128,4.64298677421305E-5,-0.0253727440697618));
#41348=CARTESIAN_POINT('',(-0.0739,1.16448635408261E-14,-1.25327725593024));
#41349=CARTESIAN_POINT('',(0.0740196805984139,-0.000529251440437712,-0.0133250000000002));
#41350=CARTESIAN_POINT('Ctrl Pts',(-0.0739168918988343,-6.56325999296619E-5,
-0.0332772559302393));
#41351=CARTESIAN_POINT('Ctrl Pts',(-0.0739653651344989,-0.00531204660183527,
-0.0328249370676371));
#41352=CARTESIAN_POINT('Ctrl Pts',(-0.0710621488839631,-0.0350524220873821,
-0.0302563214234866));
#41353=CARTESIAN_POINT('Ctrl Pts',(-0.0307802095667008,-0.0817325634071313,
-0.0255714089977876));
#41354=CARTESIAN_POINT('Ctrl Pts',(0.0499505858280116,-0.0704769373222424,
-0.0193729758836433));
#41355=CARTESIAN_POINT('Ctrl Pts',(0.0737375927583184,-0.0232593978427314,
-0.0152908395510475));
#41356=CARTESIAN_POINT('Ctrl Pts',(0.0740200992814442,-0.000529165593930002,
-0.0133250000000002));
#41357=CARTESIAN_POINT('',(0.0233628051714112,-0.0701098376443897,-0.013325));
#41358=CARTESIAN_POINT('Origin',(0.,0.,-0.013325));
#41359=CARTESIAN_POINT('Ctrl Pts',(-0.0739977701941128,4.64298677421305E-5,
-0.0253727440697618));
#41360=CARTESIAN_POINT('Ctrl Pts',(-0.0738275065859486,-0.0219387793141415,
-0.0234731261613896));
#41361=CARTESIAN_POINT('Ctrl Pts',(-0.0517129071029879,-0.0687047144129353,
-0.019457211471469));
#41362=CARTESIAN_POINT('Ctrl Pts',(5.63936834513772E-5,-0.0778762677080245,
-0.0154412967815484));
#41363=CARTESIAN_POINT('Ctrl Pts',(0.0233628051714112,-0.0701098376443897,
-0.013325));
#41364=CARTESIAN_POINT('Origin',(0.,0.,-1.25327725593024));
#41365=CARTESIAN_POINT('',(-0.0737792669902074,5.68230181076675E-6,-0.0732772559302393));
#41366=CARTESIAN_POINT('',(-0.073926283611944,-6.48147617952552E-5,-0.0653727440697618));
#41367=CARTESIAN_POINT('',(-0.0739,1.16448635408261E-14,-1.25327725593024));
#41368=CARTESIAN_POINT('Ctrl Pts',(-0.0737792669902074,5.68230181076119E-6,
-0.0732772559302393));
#41369=CARTESIAN_POINT('Ctrl Pts',(-0.0737706036350459,-0.012670925767046,
-0.0721893844235943));
#41370=CARTESIAN_POINT('Ctrl Pts',(-0.0646420250325405,-0.0500197750844117,
-0.0689852161354008));
#41371=CARTESIAN_POINT('Ctrl Pts',(-0.00531238129869321,-0.0871756978467261,
-0.0636647510656592));
#41372=CARTESIAN_POINT('Ctrl Pts',(0.0703441200498545,-0.0517629077348786,
-0.057315860721014));
#41373=CARTESIAN_POINT('Ctrl Pts',(0.0816504534154235,0.0310031138252487,
-0.0509669703763687));
#41374=CARTESIAN_POINT('Ctrl Pts',(0.018256572744571,0.0854081115037233,
-0.0446180800317234));
#41375=CARTESIAN_POINT('Ctrl Pts',(-0.0561247861037155,0.0633677973579271,
-0.0387215085496804));
#41376=CARTESIAN_POINT('Ctrl Pts',(-0.0737385699218513,0.0192347277754885,
-0.0349412338491856));
#41377=CARTESIAN_POINT('Ctrl Pts',(-0.0739168918988343,-6.56325999296619E-5,
-0.0332772559302393));
#41378=CARTESIAN_POINT('Ctrl Pts',(-0.073926283611944,-6.48147617952535E-5,
-0.0653727440697618));
#41379=CARTESIAN_POINT('Ctrl Pts',(-0.0739708590293254,-0.0049213324513921,
-0.0649538702988953));
#41380=CARTESIAN_POINT('Ctrl Pts',(-0.0713218094908637,-0.0342663620749641,
-0.0624186997464803));
#41381=CARTESIAN_POINT('Ctrl Pts',(-0.0320784659707213,-0.081233120284334,
-0.0577672324125169));
#41382=CARTESIAN_POINT('Ctrl Pts',(0.0508239621622661,-0.0710211228679567,
-0.0514183420678718));
#41383=CARTESIAN_POINT('Ctrl Pts',(0.0872462569835861,0.00415522130723803,
-0.0450694517232264));
#41384=CARTESIAN_POINT('Ctrl Pts',(0.0438253963339189,0.0755444771434547,
-0.0387205613785811));
#41385=CARTESIAN_POINT('Ctrl Pts',(-0.0396344344718481,0.0777967966107338,
-0.0323716710339359));
#41386=CARTESIAN_POINT('Ctrl Pts',(-0.0727847520006691,0.0295357616972233,
-0.0279223985976627));
#41387=CARTESIAN_POINT('Ctrl Pts',(-0.0740171912190449,0.0025541606756479,
-0.025589422942938));
#41388=CARTESIAN_POINT('Ctrl Pts',(-0.0739977701941128,4.64298677421305E-5,
-0.0253727440697618));
#41389=CARTESIAN_POINT('Origin',(0.,0.,-1.25327725593024));
#41390=CARTESIAN_POINT('',(-0.0739349529908596,6.34005555056232E-5,-0.113277255930239));
#41391=CARTESIAN_POINT('',(-0.0737787977284999,-7.08850327115771E-7,-0.105372744069761));
#41392=CARTESIAN_POINT('',(-0.0739,1.16448635408261E-14,-1.25327725593024));
#41393=CARTESIAN_POINT('Ctrl Pts',(-0.0739349529908596,6.3400555505621E-5,
-0.113277255930239));
#41394=CARTESIAN_POINT('Ctrl Pts',(-0.0737536001066518,-0.0199120788385964,
-0.111553831779551));
#41395=CARTESIAN_POINT('Ctrl Pts',(-0.055087718801892,-0.0647152520185491,
-0.107714110847315));
#41396=CARTESIAN_POINT('Ctrl Pts',(0.0206440375741234,-0.0848624350572862,
-0.101758093133531));
#41397=CARTESIAN_POINT('Ctrl Pts',(0.082485545799834,-0.0287043654232375,
-0.0954092027888854));
#41398=CARTESIAN_POINT('Ctrl Pts',(0.0688673405223371,0.0537131333497329,
-0.0890603124442403));
#41399=CARTESIAN_POINT('Ctrl Pts',(-0.00775246097108719,0.0869925938161997,
-0.0827114220995948));
#41400=CARTESIAN_POINT('Ctrl Pts',(-0.0653665291881379,0.0486231069838693,
-0.0774504032615947));
#41401=CARTESIAN_POINT('Ctrl Pts',(-0.0737874569403616,0.0119895830276085,
-0.0743056812051428));
#41402=CARTESIAN_POINT('Ctrl Pts',(-0.0737792669902074,5.68230181076119E-6,
-0.0732772559302393));
#41403=CARTESIAN_POINT('Ctrl Pts',(-0.0737788473771473,-7.08559957466985E-7,
-0.105372744069761));
#41404=CARTESIAN_POINT('Ctrl Pts',(-0.0737799052710505,-0.0122877588686294,
-0.104318317654852));
#41405=CARTESIAN_POINT('Ctrl Pts',(-0.065052998623995,-0.0492342451664978,
-0.101147594458394));
#41406=CARTESIAN_POINT('Ctrl Pts',(-0.00668590821907806,-0.0870810566848186,
-0.0958605744803883));
#41407=CARTESIAN_POINT('Ctrl Pts',(0.0695201691859918,-0.0528652704077562,
-0.0895116841357433));
#41408=CARTESIAN_POINT('Ctrl Pts',(0.0821278409720519,0.0297127773219571,
-0.0831627937910981));
#41409=CARTESIAN_POINT('Ctrl Pts',(0.0196023809749374,0.0851091659979851,
-0.0768139034464528));
#41410=CARTESIAN_POINT('Ctrl Pts',(-0.0555464352803673,0.0641271511758735,
-0.070883886872674));
#41411=CARTESIAN_POINT('Ctrl Pts',(-0.0737456484315234,0.0196154933679126,
-0.0670701670804437));
#41412=CARTESIAN_POINT('Ctrl Pts',(-0.073926283611944,-6.48147617952535E-5,
-0.0653727440697618));
#41413=CARTESIAN_POINT('Origin',(0.,0.,-1.25327725593024));
#41414=CARTESIAN_POINT('',(-0.0739827363743306,-4.67140627613241E-5,-0.153277255930239));
#41415=CARTESIAN_POINT('',(-0.0739232992014367,6.5390844150956E-5,-0.145372744069761));
#41416=CARTESIAN_POINT('',(-0.0739,1.16448635408261E-14,-1.25327725593024));
#41417=CARTESIAN_POINT('Ctrl Pts',(-0.0739827363743306,-4.67140627613194E-5,
-0.153277255930239));
#41418=CARTESIAN_POINT('Ctrl Pts',(-0.0740034660210599,-0.00285479276065182,
-0.153034575917057));
#41419=CARTESIAN_POINT('Ctrl Pts',(-0.0725839529818503,-0.0301296296558551,
-0.150675599122327));
#41420=CARTESIAN_POINT('Ctrl Pts',(-0.0387070745970641,-0.0782915758141884,
-0.146200325546048));
#41421=CARTESIAN_POINT('Ctrl Pts',(0.0447628522836712,-0.0749939700395087,
-0.139851435201402));
#41422=CARTESIAN_POINT('Ctrl Pts',(0.087282643466595,-0.00309007448744508,
-0.133502544856757));
#41423=CARTESIAN_POINT('Ctrl Pts',(0.0499541717674709,0.071640695279081,
-0.127153654512112));
#41424=CARTESIAN_POINT('Ctrl Pts',(-0.0330735811680512,0.0808328325728891,
-0.120804764167467));
#41425=CARTESIAN_POINT('Ctrl Pts',(-0.0715199200215679,0.0336552600966897,
-0.116179297973509));
#41426=CARTESIAN_POINT('Ctrl Pts',(-0.0739762942849946,0.00461702082311773,
-0.1136701285611));
#41427=CARTESIAN_POINT('Ctrl Pts',(-0.0739349529908596,6.3400555505621E-5,
-0.113277255930239));
#41428=CARTESIAN_POINT('Ctrl Pts',(-0.0739232992014367,6.53908441509508E-5,
-0.145372744069761));
#41429=CARTESIAN_POINT('Ctrl Pts',(-0.07374309713053,-0.0195303985711661,
-0.143682765010809));
#41430=CARTESIAN_POINT('Ctrl Pts',(-0.0556773602240881,-0.0639588547833093,
-0.139876489170309));
#41431=CARTESIAN_POINT('Ctrl Pts',(0.019304037012885,-0.0851772417740305,
-0.13395391654826));
#41432=CARTESIAN_POINT('Ctrl Pts',(0.0820229322870143,-0.03000077385872,
-0.127605026203615));
#41433=CARTESIAN_POINT('Ctrl Pts',(0.0697052809023569,0.0526211209250912,
-0.12125613585897));
#41434=CARTESIAN_POINT('Ctrl Pts',(-0.00638045292204925,0.0871039537597873,
-0.114907245514324));
#41435=CARTESIAN_POINT('Ctrl Pts',(-0.0649622332078741,0.0494091429444137,
-0.109612781584588));
#41436=CARTESIAN_POINT('Ctrl Pts',(-0.0737777820148128,0.0123730848425035,
-0.1064346144364));
#41437=CARTESIAN_POINT('Ctrl Pts',(-0.0737788473771473,-7.08559957466985E-7,
-0.105372744069761));
#41438=CARTESIAN_POINT('Origin',(0.,0.,-1.25327725593024));
#41439=CARTESIAN_POINT('',(-0.0737931157698702,-3.29456842671063E-5,-0.193277255930239));
#41440=CARTESIAN_POINT('',(-0.0739916274709214,-4.14334611891637E-5,-0.185372744069761));
#41441=CARTESIAN_POINT('',(-0.0739,1.16448635408261E-14,-1.25327725593024));
#41442=CARTESIAN_POINT('Ctrl Pts',(-0.0737931157698702,-3.29456842671078E-5,
-0.193277255930238));
#41443=CARTESIAN_POINT('Ctrl Pts',(-0.0738342834808563,-0.0102618987148308,
-0.192399023273014));
#41444=CARTESIAN_POINT('Ctrl Pts',(-0.0670782543545674,-0.0450877822495248,
-0.189404493834241));
#41445=CARTESIAN_POINT('Ctrl Pts',(-0.0138849007021918,-0.0862265504199637,
-0.184293667613919));
#41446=CARTESIAN_POINT('Ctrl Pts',(0.0648964354273228,-0.058448790699953,
-0.177944777269274));
#41447=CARTESIAN_POINT('Ctrl Pts',(0.0843089497489975,0.0227993301675411,
-0.171595886924629));
#41448=CARTESIAN_POINT('Ctrl Pts',(0.0265936067550599,0.0831900747965725,
-0.165246996579983));
#41449=CARTESIAN_POINT('Ctrl Pts',(-0.0523141649508524,0.0680771702324626,
-0.15914078624852));
#41450=CARTESIAN_POINT('Ctrl Pts',(-0.0738226926475932,0.0216331237873961,
-0.155150872698605));
#41451=CARTESIAN_POINT('Ctrl Pts',(-0.0739827363743306,-4.67140627613194E-5,
-0.153277255930239));
#41452=CARTESIAN_POINT('Ctrl Pts',(-0.0739916274709214,-4.14334611891758E-5,
-0.185372744069761));
#41453=CARTESIAN_POINT('Ctrl Pts',(-0.0740078983074159,-0.00246175039700786,
-0.185163509148315));
#41454=CARTESIAN_POINT('Ctrl Pts',(-0.0728023110800164,-0.0293458401691555,
-0.18283797744532));
#41455=CARTESIAN_POINT('Ctrl Pts',(-0.0399361399802455,-0.0776718285893026,
-0.178396148960777));
#41456=CARTESIAN_POINT('Ctrl Pts',(0.0435753889642203,-0.0756901163504716,
-0.172047258616132));
#41457=CARTESIAN_POINT('Ctrl Pts',(0.0872231027375695,-0.00446526306300281,
-0.165698368271486));
#41458=CARTESIAN_POINT('Ctrl Pts',(0.0510770219946841,0.0708445203210023,
-0.159349477926841));
#41459=CARTESIAN_POINT('Ctrl Pts',(-0.031795548652228,0.0813440307632768,
-0.153000587582196));
#41460=CARTESIAN_POINT('Ctrl Pts',(-0.0712639647312324,0.0344415315961151,
-0.148341676296503));
#41461=CARTESIAN_POINT('Ctrl Pts',(-0.0739687573602636,0.00500866648521042,
-0.145799061792358));
#41462=CARTESIAN_POINT('Ctrl Pts',(-0.0739232992014367,6.53908441509508E-5,
-0.145372744069761));
#41463=CARTESIAN_POINT('Origin',(0.,0.,-1.25327725593024));
#41464=CARTESIAN_POINT('',(-0.0738624655248401,6.50487107154854E-5,-0.233277255930239));
#41465=CARTESIAN_POINT('',(-0.0737987845039503,-3.83921374419449E-5,-0.225372744069761));
#41466=CARTESIAN_POINT('',(-0.0739,1.16448635408261E-14,-1.25327725593024));
#41467=CARTESIAN_POINT('Ctrl Pts',(-0.0738624655248401,6.50487107154811E-5,
-0.233277255930239));
#41468=CARTESIAN_POINT('Ctrl Pts',(-0.0737133429813345,-0.0175246640909993,
-0.231763470628971));
#41469=CARTESIAN_POINT('Ctrl Pts',(-0.058619291546274,-0.0599350351261229,
-0.228133388546155));
#41470=CARTESIAN_POINT('Ctrl Pts',(0.0121734464516189,-0.0864847712974369,
-0.222387009681791));
#41471=CARTESIAN_POINT('Ctrl Pts',(0.0792522861301636,-0.0366999129159682,
-0.216038119337145));
#41472=CARTESIAN_POINT('Ctrl Pts',(0.0738292261096514,0.046658909512726,
-0.2096892289925));
#41473=CARTESIAN_POINT('Ctrl Pts',(0.000865412281594935,0.0873330380008177,
-0.203340338647855));
#41474=CARTESIAN_POINT('Ctrl Pts',(-0.0626876098657592,0.0535380781434799,
-0.197869680960434));
#41475=CARTESIAN_POINT('Ctrl Pts',(-0.0737350807313948,0.0143870370758291,
-0.194515320054562));
#41476=CARTESIAN_POINT('Ctrl Pts',(-0.0737931157698702,-3.29456842671078E-5,
-0.193277255930238));
#41477=CARTESIAN_POINT('Ctrl Pts',(-0.0737987845039503,-3.83921374419458E-5,
-0.225372744069761));
#41478=CARTESIAN_POINT('Ctrl Pts',(-0.0738451402008693,-0.00987591182851651,
-0.224527956504272));
#41479=CARTESIAN_POINT('Ctrl Pts',(-0.0674366951185759,-0.0442996935847633,
-0.221566872157234));
#41480=CARTESIAN_POINT('Ctrl Pts',(-0.015242104357177,-0.0859970144113175,
-0.216489491028649));
#41481=CARTESIAN_POINT('Ctrl Pts',(0.0639672230445058,-0.0594642969265874,
-0.210140600684003));
#41482=CARTESIAN_POINT('Ctrl Pts',(0.0846577945115181,0.0214677912515853,
-0.203791710339358));
#41483=CARTESIAN_POINT('Ctrl Pts',(0.0279013770542819,0.0827606270598339,
-0.197442819994713));
#41484=CARTESIAN_POINT('Ctrl Pts',(-0.0516682189334046,0.0688172291131411,
-0.191303164571514));
#41485=CARTESIAN_POINT('Ctrl Pts',(-0.0738433276962178,0.0220184315257577,
-0.187279805929863));
#41486=CARTESIAN_POINT('Ctrl Pts',(-0.0739916274709214,-4.14334611891758E-5,
-0.185372744069761));
#41487=CARTESIAN_POINT('Origin',(0.,0.,-1.25327725593024));
#41488=CARTESIAN_POINT('',(-0.0740200911805013,-7.10989654978704E-6,-0.273277255930238));
#41489=CARTESIAN_POINT('',(-0.0738517712133742,6.30027790375354E-5,-0.265372744069761));
#41490=CARTESIAN_POINT('',(-0.0739,1.16448635408261E-14,-1.25327725593024));
#41491=CARTESIAN_POINT('Ctrl Pts',(-0.0740200911805012,-7.10989654978785E-6,
-0.273277255930238));
#41492=CARTESIAN_POINT('Ctrl Pts',(-0.0740206153105398,-0.000388921978886646,
-0.273244214766476));
#41493=CARTESIAN_POINT('Ctrl Pts',(-0.0738450493612621,-0.0252254210660426,
-0.271094876821166));
#41494=CARTESIAN_POINT('Ctrl Pts',(-0.04624019674556,-0.074092190342946,
-0.266829242094308));
#41495=CARTESIAN_POINT('Ctrl Pts',(0.0371479911127987,-0.0790432490549754,
-0.260480351749662));
#41496=CARTESIAN_POINT('Ctrl Pts',(0.0865523022001051,-0.0116836402180771,
-0.254131461405018));
#41497=CARTESIAN_POINT('Ctrl Pts',(0.0567764831078735,0.0663644440252806,
-0.247782571060372));
#41498=CARTESIAN_POINT('Ctrl Pts',(-0.0249398298746646,0.083700736858798,
-0.241433680715727));
#41499=CARTESIAN_POINT('Ctrl Pts',(-0.0697966989192059,0.0385891993466075,
-0.236598575672349));
#41500=CARTESIAN_POINT('Ctrl Pts',(-0.0739218187530394,0.00706604408899114,
-0.23387976741052));
#41501=CARTESIAN_POINT('Ctrl Pts',(-0.0738624655248401,6.50487107154811E-5,
-0.233277255930239));
#41502=CARTESIAN_POINT('Ctrl Pts',(-0.0738517712133742,6.30027790375388E-5,
-0.265372744069761));
#41503=CARTESIAN_POINT('Ctrl Pts',(-0.0737120444937011,-0.01714439698726,
-0.263892403860229));
#41504=CARTESIAN_POINT('Ctrl Pts',(-0.0591470434262601,-0.0591647511335928,
-0.260295766869149));
#41505=CARTESIAN_POINT('Ctrl Pts',(0.0108089364983639,-0.086665882126032,
-0.25458283309652));
#41506=CARTESIAN_POINT('Ctrl Pts',(0.0786640523710499,-0.0379443684553606,
-0.248233942751875));
#41507=CARTESIAN_POINT('Ctrl Pts',(0.0745553989520529,0.045489567155642,
-0.24188505240723));
#41508=CARTESIAN_POINT('Ctrl Pts',(0.00224167132305463,0.087308551371477,
-0.235536162062585));
#41509=CARTESIAN_POINT('Ctrl Pts',(-0.0622278064411262,0.0543189253670649,
-0.230032059283428));
#41510=CARTESIAN_POINT('Ctrl Pts',(-0.0737290134771772,0.0147682852585804,
-0.22664425328582));
#41511=CARTESIAN_POINT('Ctrl Pts',(-0.0737987845039503,-3.83921374419458E-5,
-0.225372744069761));
#41512=CARTESIAN_POINT('Origin',(0.,0.,-1.25327725593024));
#41513=CARTESIAN_POINT('',(-0.0738418054104652,-6.0444388606692E-5,-0.313277255930238));
#41514=CARTESIAN_POINT('',(-0.0740209430351333,8.71191224640759E-8,-0.305372744069761));
#41515=CARTESIAN_POINT('',(-0.0739,1.16448635408261E-14,-1.25327725593024));
#41516=CARTESIAN_POINT('Ctrl Pts',(-0.0738418054104652,-6.04443886067091E-5,
-0.313277255930238));
#41517=CARTESIAN_POINT('Ctrl Pts',(-0.073901771058743,-0.00783479649662774,
-0.312608662122434));
#41518=CARTESIAN_POINT('Ctrl Pts',(-0.0691933312609605,-0.0401464863470307,
-0.309823771533081));
#41519=CARTESIAN_POINT('Ctrl Pts',(-0.0223216715032739,-0.0844366712168558,
-0.304922584162179));
#41520=CARTESIAN_POINT('Ctrl Pts',(0.0588152484367718,-0.0645645027565787,
-0.298573693817534));
#41521=CARTESIAN_POINT('Ctrl Pts',(0.0861465628713941,0.0143728274994348,
-0.292224803472889));
#41522=CARTESIAN_POINT('Ctrl Pts',(0.0346689272343444,0.0801615490700074,
-0.285875913128243));
#41523=CARTESIAN_POINT('Ctrl Pts',(-0.0480917181638159,0.0726558212856807,
-0.27956006394736));
#41524=CARTESIAN_POINT('Ctrl Pts',(-0.0739870446190946,0.0240662602546987,
-0.275360511548025));
#41525=CARTESIAN_POINT('Ctrl Pts',(-0.0740200911805012,-7.10989654978785E-6,
-0.273277255930238));
#41526=CARTESIAN_POINT('Ctrl Pts',(-0.0740209430351333,8.71191224682221E-8,
-0.305372744069761));
#41527=CARTESIAN_POINT('Ctrl Pts',(-0.0740205148794295,-0.0244496669579938,
-0.303256851216186));
#41528=CARTESIAN_POINT('Ctrl Pts',(-0.0473968446054434,-0.0733546414550255,
-0.299024661581064));
#41529=CARTESIAN_POINT('Ctrl Pts',(0.0358976572459432,-0.0796188824159332,
-0.292676175164391));
#41530=CARTESIAN_POINT('Ctrl Pts',(0.0863574175401337,-0.0130462511361909,
-0.286327284819747));
#41531=CARTESIAN_POINT('Ctrl Pts',(0.0578153328344367,0.0654614048287443,
-0.279978394475101));
#41532=CARTESIAN_POINT('Ctrl Pts',(-0.0236176105063063,0.0840833913854678,
-0.273629504130456));
#41533=CARTESIAN_POINT('Ctrl Pts',(-0.0694950249696135,0.039377286418387,
-0.268760953995342));
#41534=CARTESIAN_POINT('Ctrl Pts',(-0.0739117980403768,0.00745532982536957,
-0.266008700641778));
#41535=CARTESIAN_POINT('Ctrl Pts',(-0.0738517712133742,6.30027790375388E-5,
-0.265372744069761));
#41536=CARTESIAN_POINT('Origin',(0.,0.,-1.25327725593024));
#41537=CARTESIAN_POINT('',(-0.073805155490977,4.33812301120649E-5,-0.353277255930238));
#41538=CARTESIAN_POINT('',(-0.0738520240961663,-6.3059175845967E-5,-0.345372744069761));
#41539=CARTESIAN_POINT('',(-0.0739,1.16448635408261E-14,-1.25327725593024));
#41540=CARTESIAN_POINT('Ctrl Pts',(-0.073805155490977,4.33812301120651E-5,
-0.353277255930238));
#41541=CARTESIAN_POINT('Ctrl Pts',(-0.0737238735552172,-0.0151400725974492,
-0.351973109478391));
#41542=CARTESIAN_POINT('Ctrl Pts',(-0.0617703018698818,-0.0550798102599285,
-0.348552666244995));
#41543=CARTESIAN_POINT('Ctrl Pts',(0.00358415316748011,-0.0872637514146367,
-0.343015926230051));
#41544=CARTESIAN_POINT('Ctrl Pts',(0.0752461815192336,-0.0443375758432733,
-0.336667035885405));
#41545=CARTESIAN_POINT('Ctrl Pts',(0.0780711911348368,0.0391496817314182,
-0.330318145540761));
#41546=CARTESIAN_POINT('Ctrl Pts',(0.00947479519341831,0.0868218677576465,
-0.323969255196115));
#41547=CARTESIAN_POINT('Ctrl Pts',(-0.0596527774820103,0.0584113509348891,
-0.318288958659274));
#41548=CARTESIAN_POINT('Ctrl Pts',(-0.0737119620791017,0.0167733230413832,
-0.314724958903982));
#41549=CARTESIAN_POINT('Ctrl Pts',(-0.0738418054104652,-6.04443886067091E-5,
-0.313277255930238));
#41550=CARTESIAN_POINT('Ctrl Pts',(-0.0738520240961663,-6.30591758459618E-5,
-0.345372744069761));
#41551=CARTESIAN_POINT('Ctrl Pts',(-0.0739120432883483,-0.00744593178717649,
-0.344737595353692));
#41552=CARTESIAN_POINT('Ctrl Pts',(-0.0695024008175162,-0.0393582484273959,
-0.341986149856075));
#41553=CARTESIAN_POINT('Ctrl Pts',(-0.0236496187649619,-0.0840743942302376,
-0.337118407576909));
#41554=CARTESIAN_POINT('Ctrl Pts',(0.0577904079373426,-0.0654834099856214,
-0.330769517232263));
#41555=CARTESIAN_POINT('Ctrl Pts',(0.086362377900638,0.0130133745145877,
-0.324420626887618));
#41556=CARTESIAN_POINT('Ctrl Pts',(0.0359279650068146,0.0796052106546962,
-0.318071736542973));
#41557=CARTESIAN_POINT('Ctrl Pts',(-0.0473742153988214,0.073372283242758,
-0.311722846198328));
#41558=CARTESIAN_POINT('Ctrl Pts',(-0.074018829535515,0.0244638436337662,
-0.307489848707257));
#41559=CARTESIAN_POINT('Ctrl Pts',(-0.074020943116869,4.75462372219806E-6,
-0.305373147997735));
#41560=CARTESIAN_POINT('Ctrl Pts',(-0.0740209430351333,8.71191224682221E-8,
-0.305372744069761));
#41561=CARTESIAN_POINT('Origin',(0.,0.,-1.25327725593024));
#41562=CARTESIAN_POINT('',(-0.0739994218128981,3.58154130656329E-5,-0.393277255930239));
#41563=CARTESIAN_POINT('',(-0.0737986371542887,3.82643731348629E-5,-0.385372744069761));
#41564=CARTESIAN_POINT('',(-0.0739,1.16448635408261E-14,-1.25327725593024));
#41565=CARTESIAN_POINT('Ctrl Pts',(-0.0739994218128981,3.58154130656275E-5,
-0.393277255930239));
#41566=CARTESIAN_POINT('Ctrl Pts',(-0.0738654336872465,-0.0223953451531454,
-0.391337556834348));
#41567=CARTESIAN_POINT('Ctrl Pts',(-0.0510278128527495,-0.0695361071795467,
-0.387281560956909));
#41568=CARTESIAN_POINT('Ctrl Pts',(0.0291708805188321,-0.082321735857788,
-0.381109268297923));
#41569=CARTESIAN_POINT('Ctrl Pts',(0.0849779436410596,-0.0201632725374741,
-0.374760377953277));
#41570=CARTESIAN_POINT('Ctrl Pts',(0.0630451377031669,0.0604410380194803,
-0.368411487608632));
#41571=CARTESIAN_POINT('Ctrl Pts',(-0.0165628782942129,0.0857524316127216,
-0.362062597263987));
#41572=CARTESIAN_POINT('Ctrl Pts',(-0.0677786767413996,0.0435304809960098,
-0.357017853371189));
#41573=CARTESIAN_POINT('Ctrl Pts',(-0.0738557733880947,0.00949879708052387,
-0.35408940625994));
#41574=CARTESIAN_POINT('Ctrl Pts',(-0.073805155490977,4.33812301120651E-5,
-0.353277255930238));
#41575=CARTESIAN_POINT('Ctrl Pts',(-0.0737986371542887,3.82643731348673E-5,
-0.385372744069761));
#41576=CARTESIAN_POINT('Ctrl Pts',(-0.0737291507439404,-0.0147590795369847,
-0.384102042709649));
#41577=CARTESIAN_POINT('Ctrl Pts',(-0.0622390202126849,-0.0543000773339284,
-0.380715044567989));
#41578=CARTESIAN_POINT('Ctrl Pts',(0.00220843339423072,-0.0873093984336892,
-0.375211749644781));
#41579=CARTESIAN_POINT('Ctrl Pts',(0.0745380759834756,-0.0455179465880336,
-0.368862859300135));
#41580=CARTESIAN_POINT('Ctrl Pts',(0.0786784918314324,0.0379144188408675,
-0.36251396895549));
#41581=CARTESIAN_POINT('Ctrl Pts',(0.0108419288216904,0.0866617609579614,
-0.356165078610845));
#41582=CARTESIAN_POINT('Ctrl Pts',(-0.0591344093577337,0.0591833785993506,
-0.350451336982268));
#41583=CARTESIAN_POINT('Ctrl Pts',(-0.0737120611108954,0.0171535819182837,
-0.34685389213524));
#41584=CARTESIAN_POINT('Ctrl Pts',(-0.0738520240961663,-6.30591758459618E-5,
-0.345372744069761));
#41585=CARTESIAN_POINT('Origin',(0.,0.,-1.25327725593024));
#41586=CARTESIAN_POINT('',(-0.0739118163224249,-6.66974575854458E-5,-0.433277255930238));
#41587=CARTESIAN_POINT('',(-0.0739914229668183,4.15668966620335E-5,-0.42537274406976));
#41588=CARTESIAN_POINT('',(-0.0739,1.16448635408261E-14,-1.25327725593024));
#41589=CARTESIAN_POINT('Ctrl Pts',(-0.0739118163224248,-6.66974575854462E-5,
-0.433277255930238));
#41590=CARTESIAN_POINT('Ctrl Pts',(-0.0739609375286694,-0.00539053570481102,
-0.432818300971854));
#41591=CARTESIAN_POINT('Ctrl Pts',(-0.0710073599783538,-0.0352091741461071,
-0.430243049231921));
#41592=CARTESIAN_POINT('Ctrl Pts',(-0.0305407719561762,-0.0818234056563543,
-0.425551500710439));
#41593=CARTESIAN_POINT('Ctrl Pts',(0.0521605230517608,-0.0700506124159539,
-0.419202610365794));
#41594=CARTESIAN_POINT('Ctrl Pts',(0.0871441155782282,0.00580616783876835,
-0.412853720021149));
#41595=CARTESIAN_POINT('Ctrl Pts',(0.0424061727963488,0.0763513259455898,
-0.406504829676504));
#41596=CARTESIAN_POINT('Ctrl Pts',(-0.0411259579745188,0.0770484525838227,
-0.400155939331858));
#41597=CARTESIAN_POINT('Ctrl Pts',(-0.0730090199367733,0.0285814762061514,
-0.395746748083104));
#41598=CARTESIAN_POINT('Ctrl Pts',(-0.0740116206085493,0.00207803477121929,
-0.393453853615897));
#41599=CARTESIAN_POINT('Ctrl Pts',(-0.0739994218128981,3.58154130656275E-5,
-0.393277255930239));
#41600=CARTESIAN_POINT('Ctrl Pts',(-0.0739914229668183,4.15668966620296E-5,
-0.42537274406976));
#41601=CARTESIAN_POINT('Ctrl Pts',(-0.0738428054161868,-0.0220091137494347,
-0.423466490065606));
#41602=CARTESIAN_POINT('Ctrl Pts',(-0.0516839443637501,-0.068799393046605,
-0.419443939279904));
#41603=CARTESIAN_POINT('Ctrl Pts',(0.0278698686279614,-0.0827712429263309,
-0.413305091712652));
#41604=CARTESIAN_POINT('Ctrl Pts',(0.0846496157370046,-0.0215000183368973,
-0.406956201368007));
#41605=CARTESIAN_POINT('Ctrl Pts',(0.0639898560584943,0.0594399407345146,
-0.400607311023361));
#41606=CARTESIAN_POINT('Ctrl Pts',(-0.0152093647792003,0.0860028107443161,
-0.394258420678717));
#41607=CARTESIAN_POINT('Ctrl Pts',(-0.0674281327856323,0.0443187318135554,
-0.389180231694183));
#41608=CARTESIAN_POINT('Ctrl Pts',(-0.0738448772798502,0.00988524073800117,
-0.386218339491197));
#41609=CARTESIAN_POINT('Ctrl Pts',(-0.0737986371542887,3.82643731348673E-5,
-0.385372744069761));
#41610=CARTESIAN_POINT('Origin',(0.,0.,-1.25327725593024));
#41611=CARTESIAN_POINT('',(-0.0737794295953435,6.93418815541041E-6,-0.473277255930238));
#41612=CARTESIAN_POINT('',(-0.0739235825009513,-6.53505266424922E-5,-0.46537274406976));
#41613=CARTESIAN_POINT('',(-0.0739,1.16448635408261E-14,-1.25327725593024));
#41614=CARTESIAN_POINT('Ctrl Pts',(-0.0737794295953435,6.9341881554115E-6,
-0.473277255930238));
#41615=CARTESIAN_POINT('Ctrl Pts',(-0.0737687447719428,-0.0127469243178594,
-0.472182748327811));
#41616=CARTESIAN_POINT('Ctrl Pts',(-0.0645593346287235,-0.0501755960073792,
-0.468971943943835));
#41617=CARTESIAN_POINT('Ctrl Pts',(-0.0050400910778892,-0.0871917768302152,
-0.463644842778311));
#41618=CARTESIAN_POINT('Ctrl Pts',(0.070506311846667,-0.0515428797668893,
-0.457295952433666));
#41619=CARTESIAN_POINT('Ctrl Pts',(0.0815518429447203,0.0312586848284312,
-0.45094706208902));
#41620=CARTESIAN_POINT('Ctrl Pts',(0.0179917843980893,0.0854640518525547,
-0.444598171744375));
#41621=CARTESIAN_POINT('Ctrl Pts',(-0.0562430707592223,0.0632182791999014,
-0.438708236358114));
#41622=CARTESIAN_POINT('Ctrl Pts',(-0.0737344337099786,0.0191583258822792,
-0.434934597753402));
#41623=CARTESIAN_POINT('Ctrl Pts',(-0.0739118163224248,-6.66974575854462E-5,
-0.433277255930238));
#41624=CARTESIAN_POINT('Ctrl Pts',(-0.0739235825009513,-6.53505266424888E-5,
-0.46537274406976));
#41625=CARTESIAN_POINT('Ctrl Pts',(-0.0739689452559117,-0.00499921021186099,
-0.464947234203111));
#41626=CARTESIAN_POINT('Ctrl Pts',(-0.0712702306590702,-0.0344225349892039,
-0.462405427554914));
#41627=CARTESIAN_POINT('Ctrl Pts',(-0.0318265133113365,-0.0813319204454977,
-0.45774732412517));
#41628=CARTESIAN_POINT('Ctrl Pts',(0.0510500481910435,-0.070863959899244,
-0.451398433780523));
#41629=CARTESIAN_POINT('Ctrl Pts',(0.0872247963540974,0.00443205752395941,
-0.445049543435879));
#41630=CARTESIAN_POINT('Ctrl Pts',(0.0436042004922963,0.0756735220029905,
-0.438700653091233));
#41631=CARTESIAN_POINT('Ctrl Pts',(-0.0399065679425262,0.0776870263812308,
-0.432351762746588));
#41632=CARTESIAN_POINT('Ctrl Pts',(-0.0727971149138888,0.0293647663870503,
-0.427909126406097));
#41633=CARTESIAN_POINT('Ctrl Pts',(-0.0740077985615901,0.00247124636028123,
-0.425582786847154));
#41634=CARTESIAN_POINT('Ctrl Pts',(-0.0739914229668183,4.15668966620296E-5,
-0.42537274406976));
#41635=CARTESIAN_POINT('Origin',(0.,0.,-1.25327725593024));
#41636=CARTESIAN_POINT('',(-0.0739372416732134,6.29279406287392E-5,-0.513277255930238));
#41637=CARTESIAN_POINT('',(-0.0737788291172461,5.56757125268528E-7,-0.505372744069761));
#41638=CARTESIAN_POINT('',(-0.0739,1.16448635408261E-14,-1.25327725593024));
#41639=CARTESIAN_POINT('Ctrl Pts',(-0.0739372416732135,6.29279406287363E-5,
-0.513277255930238));
#41640=CARTESIAN_POINT('Ctrl Pts',(-0.0737558839958198,-0.0199878652888913,
-0.511547195683768));
#41641=CARTESIAN_POINT('Ctrl Pts',(-0.0549695186936256,-0.0648650221978919,
-0.50770083865575));
#41642=CARTESIAN_POINT('Ctrl Pts',(0.0209093093381367,-0.0847974601499693,
-0.501738184846182));
#41643=CARTESIAN_POINT('Ctrl Pts',(0.0825749204933152,-0.0284462821895266,
-0.495389294501537));
#41644=CARTESIAN_POINT('Ctrl Pts',(0.0686990060272686,0.0539282396870952,
-0.489040404156892));
#41645=CARTESIAN_POINT('Ctrl Pts',(-0.00802441338286892,0.0869679093386998,
-0.482691513812247));
#41646=CARTESIAN_POINT('Ctrl Pts',(-0.0654458135203799,0.0484671034431539,
-0.477437131070029));
#41647=CARTESIAN_POINT('Ctrl Pts',(-0.0737894045255381,0.0119134340467115,
-0.474299045109359));
#41648=CARTESIAN_POINT('Ctrl Pts',(-0.0737794295953435,6.9341881554115E-6,
-0.473277255930238));
#41649=CARTESIAN_POINT('Ctrl Pts',(-0.0737788400683315,5.56706807122026E-7,
-0.505372744069761));
#41650=CARTESIAN_POINT('Ctrl Pts',(-0.0737780088266581,-0.0123638253439393,
-0.504311681559069));
#41651=CARTESIAN_POINT('Ctrl Pts',(-0.0649721116611022,-0.0493901687656836,
-0.501134322266829));
#41652=CARTESIAN_POINT('Ctrl Pts',(-0.00641360530457873,-0.0871015149116623,
-0.49584066619304));
#41653=CARTESIAN_POINT('Ctrl Pts',(0.0696852396434252,-0.0526476553015217,
-0.489491775848395));
#41654=CARTESIAN_POINT('Ctrl Pts',(0.0820343493873717,0.0299695471020194,
-0.48314288550375));
#41655=CARTESIAN_POINT('Ctrl Pts',(0.0193364609744337,0.0851698861681384,
-0.476793995159104));
#41656=CARTESIAN_POINT('Ctrl Pts',(-0.0556632358337177,0.0639771560029762,
-0.470870614681109));
#41657=CARTESIAN_POINT('Ctrl Pts',(-0.0737433310931167,0.01953961295263,
-0.46706353098466));
#41658=CARTESIAN_POINT('Ctrl Pts',(-0.0739235825009513,-6.53505266424888E-5,
-0.46537274406976));
#41659=CARTESIAN_POINT('Origin',(0.,0.,-1.25327725593024));
#41660=CARTESIAN_POINT('',(-0.073980874458951,-4.77002733273939E-5,-0.553277255930238));
#41661=CARTESIAN_POINT('',(-0.0739256241017582,6.50482031668356E-5,-0.545372744069761));
#41662=CARTESIAN_POINT('',(-0.0739,1.16448635408261E-14,-1.25327725593024));
#41663=CARTESIAN_POINT('Ctrl Pts',(-0.0739808744589511,-4.77002733273914E-5,
-0.553277255930238));
#41664=CARTESIAN_POINT('Ctrl Pts',(-0.0740025130732811,-0.0029327564029972,
-0.553027939821274));
#41665=CARTESIAN_POINT('Ctrl Pts',(-0.0725398341957257,-0.0302852066985371,
-0.550662326930761));
#41666=CARTESIAN_POINT('Ctrl Pts',(-0.0384620532909962,-0.0784122370649128,
-0.5461804172587));
#41667=CARTESIAN_POINT('Ctrl Pts',(0.0449971529934493,-0.0748536217384812,
-0.539831526914054));
#41668=CARTESIAN_POINT('Ctrl Pts',(0.0872918802153685,-0.00281711081593204,
-0.533482636569409));
#41669=CARTESIAN_POINT('Ctrl Pts',(0.0497298934808031,0.0717965609153495,
-0.527133746224764));
#41670=CARTESIAN_POINT('Ctrl Pts',(-0.0333261972756367,0.0807290099036824,
-0.520784855880119));
#41671=CARTESIAN_POINT('Ctrl Pts',(-0.0715698711116002,0.0334992973532661,
-0.516166025781943));
#41672=CARTESIAN_POINT('Ctrl Pts',(-0.0739777298360213,0.00453927430968902,
-0.513663492465317));
#41673=CARTESIAN_POINT('Ctrl Pts',(-0.0739372416732135,6.29279406287363E-5,
-0.513277255930238));
#41674=CARTESIAN_POINT('Ctrl Pts',(-0.0739256241017582,6.50482031668361E-5,
-0.545372744069761));
#41675=CARTESIAN_POINT('Ctrl Pts',(-0.0737450480884514,-0.0196060964085107,
-0.543676128915026));
#41676=CARTESIAN_POINT('Ctrl Pts',(-0.0555611653360301,-0.064109143640121,
-0.539863216978743));
#41677=CARTESIAN_POINT('Ctrl Pts',(0.0195703062739464,-0.085116457546431,
-0.533934008260913));
#41678=CARTESIAN_POINT('Ctrl Pts',(0.0821163510431211,-0.0297441275594417,
-0.527585117916266));
#41679=CARTESIAN_POINT('Ctrl Pts',(0.0695403805661829,0.052838846539454,
-0.521236227571622));
#41680=CARTESIAN_POINT('Ctrl Pts',(-0.00665280454283421,0.0870835714967197,
-0.514887337226976));
#41681=CARTESIAN_POINT('Ctrl Pts',(-0.0650431584057082,0.0492532338086213,
-0.509599509393023));
#41682=CARTESIAN_POINT('Ctrl Pts',(-0.0737796667441326,0.0122970232640985,
-0.506427978340618));
#41683=CARTESIAN_POINT('Ctrl Pts',(-0.0737788400683315,5.56706807122026E-7,
-0.505372744069761));
#41684=CARTESIAN_POINT('Origin',(0.,0.,-1.25327725593024));
#41685=CARTESIAN_POINT('',(-0.0737920974294479,-3.18290494924771E-5,-0.593277255930238));
#41686=CARTESIAN_POINT('',(-0.0739899318680459,-4.25211598454808E-5,-0.585372744069761));
#41687=CARTESIAN_POINT('',(-0.0739,1.16448635408261E-14,-1.25327725593024));
#41688=CARTESIAN_POINT('Ctrl Pts',(-0.0737920974294479,-3.18290494924836E-5,
-0.593277255930238));
#41689=CARTESIAN_POINT('Ctrl Pts',(-0.0738321381747954,-0.0103384296985671,
-0.592392387177231));
#41690=CARTESIAN_POINT('Ctrl Pts',(-0.06700616371982,-0.0452441277251543,
-0.589391221642675));
#41691=CARTESIAN_POINT('Ctrl Pts',(-0.0136151867463331,-0.0862695494061835,
-0.584273759326571));
#41692=CARTESIAN_POINT('Ctrl Pts',(0.06507889807261,-0.058245561981479,
-0.577924868981926));
#41693=CARTESIAN_POINT('Ctrl Pts',(0.0842372398743852,0.0230628680616442,
-0.57157597863728));
#41694=CARTESIAN_POINT('Ctrl Pts',(0.0263333262574912,0.083272831062118,
-0.565227088292636));
#41695=CARTESIAN_POINT('Ctrl Pts',(-0.0524410953307806,0.0679299339365414,
-0.559127514056954));
#41696=CARTESIAN_POINT('Ctrl Pts',(-0.0738188356925693,0.0215567762917269,
-0.555144236602822));
#41697=CARTESIAN_POINT('Ctrl Pts',(-0.0739808744589511,-4.77002733273914E-5,
-0.553277255930238));
#41698=CARTESIAN_POINT('Ctrl Pts',(-0.0739899318680459,-4.25211598455012E-5,
-0.585372744069761));
#41699=CARTESIAN_POINT('Ctrl Pts',(-0.0740070680983731,-0.0025397515316431,
-0.585156873052532));
#41700=CARTESIAN_POINT('Ctrl Pts',(-0.0727595129678202,-0.0295013175423853,
-0.582824705253755));
#41701=CARTESIAN_POINT('Ctrl Pts',(-0.0396930507999507,-0.0777963363604095,
-0.578376240673428));
#41702=CARTESIAN_POINT('Ctrl Pts',(0.0438118725954223,-0.0755534780972525,
-0.572027350328785));
#41703=CARTESIAN_POINT('Ctrl Pts',(0.0872366399772161,-0.00419247878885715,
-0.565678459984137));
#41704=CARTESIAN_POINT('Ctrl Pts',(0.0508552285025388,0.0710039010679274,
-0.559329569639494));
#41705=CARTESIAN_POINT('Ctrl Pts',(-0.0320497705692809,0.0812442024969535,
-0.552980679294847));
#41706=CARTESIAN_POINT('Ctrl Pts',(-0.0713153122300141,0.0342854907512878,
-0.548328404104937));
#41707=CARTESIAN_POINT('Ctrl Pts',(-0.0739702921190258,0.00493098256010466,
-0.545792425696575));
#41708=CARTESIAN_POINT('Ctrl Pts',(-0.0739256241017582,6.50482031668361E-5,
-0.545372744069761));
#41709=CARTESIAN_POINT('Origin',(0.,0.,-1.25327725593024));
#41710=CARTESIAN_POINT('',(-0.0738646379472932,6.53830851695627E-5,-0.633277255930239));
#41711=CARTESIAN_POINT('',(-0.0737975891722939,-3.73368331001503E-5,-0.625372744069761));
#41712=CARTESIAN_POINT('',(-0.0739,1.16448635408261E-14,-1.25327725593024));
#41713=CARTESIAN_POINT('Ctrl Pts',(-0.0738646379472931,6.53830851695594E-5,
-0.633277255930239));
#41714=CARTESIAN_POINT('Ctrl Pts',(-0.0737137520287097,-0.0176001212798387,
-0.631756834533189));
#41715=CARTESIAN_POINT('Ctrl Pts',(-0.0585134263150157,-0.0600876505745179,
-0.62812011635459));
#41716=CARTESIAN_POINT('Ctrl Pts',(0.0124438404931729,-0.0864462798428249,
-0.622367101394442));
#41717=CARTESIAN_POINT('Ctrl Pts',(0.0793666658984961,-0.0364518971939734,
-0.616018211049798));
#41718=CARTESIAN_POINT('Ctrl Pts',(0.073682954238757,0.0468895587474729,
-0.609669320705152));
#41719=CARTESIAN_POINT('Ctrl Pts',(0.000592301800611145,0.087335317274631,
-0.603320430360507));
#41720=CARTESIAN_POINT('Ctrl Pts',(-0.0627777631997439,0.053383016163664,
-0.59785640876887));
#41721=CARTESIAN_POINT('Ctrl Pts',(-0.0737363747067989,0.0143113567338424,
-0.59450868395878));
#41722=CARTESIAN_POINT('Ctrl Pts',(-0.0737920974294479,-3.18290494924836E-5,
-0.593277255930238));
#41723=CARTESIAN_POINT('Ctrl Pts',(-0.0737975891722939,-3.73368331001503E-5,
-0.625372744069761));
#41724=CARTESIAN_POINT('Ctrl Pts',(-0.0738429811604534,-0.00995253562942452,
-0.624521320408489));
#41725=CARTESIAN_POINT('Ctrl Pts',(-0.0673662201976671,-0.0444560792889662,
-0.62155359996567));
#41726=CARTESIAN_POINT('Ctrl Pts',(-0.0149731015673857,-0.0860442587414302,
-0.6164695827413));
#41727=CARTESIAN_POINT('Ctrl Pts',(0.0641528659084539,-0.0592639690591287,
-0.610120692396656));
#41728=CARTESIAN_POINT('Ctrl Pts',(0.0845902468891876,0.0217324265588487,
-0.60377180205201));
#41729=CARTESIAN_POINT('Ctrl Pts',(0.027642433133917,0.0828474750571577,
-0.597422911707366));
#41730=CARTESIAN_POINT('Ctrl Pts',(-0.0517972143618181,0.0686706564364598,
-0.591289892379948));
#41731=CARTESIAN_POINT('Ctrl Pts',(-0.0738390726464825,0.0219419073147564,
-0.58727316983408));
#41732=CARTESIAN_POINT('Ctrl Pts',(-0.0739899318680459,-4.25211598455012E-5,
-0.585372744069761));
#41733=CARTESIAN_POINT('Origin',(0.,0.,-1.25327725593024));
#41734=CARTESIAN_POINT('',(-0.0740197207812738,-8.52928078186594E-6,-0.673277255930238));
#41735=CARTESIAN_POINT('',(-0.0738538568161215,6.34559343100465E-5,-0.665372744069761));
#41736=CARTESIAN_POINT('',(-0.0739,1.16448635408261E-14,-1.25327725593024));
#41737=CARTESIAN_POINT('Ctrl Pts',(-0.0740197207812738,-8.5292807818521E-6,
-0.673277255930238));
#41738=CARTESIAN_POINT('Ctrl Pts',(-0.0740204699529474,-0.00046703193262174,
-0.673237578670693));
#41739=CARTESIAN_POINT('Ctrl Pts',(-0.073808986523765,-0.0253803366732234,
-0.671081604629601));
#41740=CARTESIAN_POINT('Ctrl Pts',(-0.0460082709303986,-0.0742364295402099,
-0.66680933380696));
#41741=CARTESIAN_POINT('Ctrl Pts',(0.037394992047993,-0.0789266940560291,
-0.660460443462315));
#41742=CARTESIAN_POINT('Ctrl Pts',(0.0865884158521809,-0.0114129183425305,
-0.654111553117668));
#41743=CARTESIAN_POINT('Ctrl Pts',(0.0565686718383231,0.0665416698868583,
-0.647762662773025));
#41744=CARTESIAN_POINT('Ctrl Pts',(-0.0252014553124982,0.0836223362207471,
-0.641413772428377));
#41745=CARTESIAN_POINT('Ctrl Pts',(-0.0698556617272321,0.0384328507297029,
-0.636585303480784));
#41746=CARTESIAN_POINT('Ctrl Pts',(-0.0739237723457736,0.00698875263671575,
-0.633873131314737));
#41747=CARTESIAN_POINT('Ctrl Pts',(-0.0738646379472931,6.53830851695594E-5,
-0.633277255930239));
#41748=CARTESIAN_POINT('Ctrl Pts',(-0.0738538568161215,6.34559343100473E-5,
-0.665372744069761));
#41749=CARTESIAN_POINT('Ctrl Pts',(-0.0737122022775332,-0.0172198463724857,
-0.663885767764447));
#41750=CARTESIAN_POINT('Ctrl Pts',(-0.0590430950891427,-0.0593177345607098,
-0.660282494677584));
#41751=CARTESIAN_POINT('Ctrl Pts',(0.011079903578258,-0.0866316568559436,
-0.654562924809171));
#41752=CARTESIAN_POINT('Ctrl Pts',(0.0787823266538737,-0.0376981861620926,
-0.648214034464528));
#41753=CARTESIAN_POINT('Ctrl Pts',(0.0744127802759426,0.0457224929822708,
-0.641865144119881));
#41754=CARTESIAN_POINT('Ctrl Pts',(0.00196863068701841,0.0873151345765873,
-0.635516253775237));
#41755=CARTESIAN_POINT('Ctrl Pts',(-0.0623197635665918,0.0541640793943838,
-0.630018787091862));
#41756=CARTESIAN_POINT('Ctrl Pts',(-0.0737301549344281,0.0146926607111806,
-0.626637617190037));
#41757=CARTESIAN_POINT('Ctrl Pts',(-0.0737975891722939,-3.73368331001503E-5,
-0.625372744069761));
#41758=CARTESIAN_POINT('Origin',(0.,0.,-1.25327725593024));
#41759=CARTESIAN_POINT('',(-0.0738398419805284,-5.98587458514904E-5,-0.713277255930238));
#41760=CARTESIAN_POINT('',(-0.0740209121467327,-1.34404130546634E-6,-0.705372744069761));
#41761=CARTESIAN_POINT('',(-0.0739,1.16448635408261E-14,-1.25327725593024));
#41762=CARTESIAN_POINT('Ctrl Pts',(-0.0738398419805284,-5.98587458514712E-5,
-0.713277255930238));
#41763=CARTESIAN_POINT('Ctrl Pts',(-0.0738997053742793,-0.00791190180289649,
-0.712602026026651));
#41764=CARTESIAN_POINT('Ctrl Pts',(-0.0691310979633685,-0.0403029009963255,
-0.709810499341516));
#41765=CARTESIAN_POINT('Ctrl Pts',(-0.0220575135733365,-0.0845060622668312,
-0.704902675874831));
#41766=CARTESIAN_POINT('Ctrl Pts',(0.0590168657611575,-0.064380261110165,
-0.698553785530186));
#41767=CARTESIAN_POINT('Ctrl Pts',(0.0861011952070565,0.0146421531476717,
-0.692204895185541));
#41768=CARTESIAN_POINT('Ctrl Pts',(0.0344180780130461,0.080269573131862,
-0.685856004840895));
#41769=CARTESIAN_POINT('Ctrl Pts',(-0.0482317589869109,0.0725132326990022,
-0.679546791755795));
#41770=CARTESIAN_POINT('Ctrl Pts',(-0.0739805108020415,0.0239884798028173,
-0.675353875452242));
#41771=CARTESIAN_POINT('Ctrl Pts',(-0.0740197207812738,-8.5292807818521E-6,
-0.673277255930238));
#41772=CARTESIAN_POINT('Ctrl Pts',(-0.0740209121467327,-1.34404130547942E-6,
-0.705372744069761));
#41773=CARTESIAN_POINT('Ctrl Pts',(-0.0740209314587002,-7.33586246526099E-5,
-0.705366511901952));
#41774=CARTESIAN_POINT('Ctrl Pts',(-0.0739882313484256,-0.0245998043267833,
-0.703243982952595));
#41775=CARTESIAN_POINT('Ctrl Pts',(-0.047172520489486,-0.0735021193135168,
-0.699005157221689));
#41776=CARTESIAN_POINT('Ctrl Pts',(0.0361464644047429,-0.0795062346231174,
-0.692656266877045));
#41777=CARTESIAN_POINT('Ctrl Pts',(0.0863977932766005,-0.0127761320376415,
-0.686307376532398));
#41778=CARTESIAN_POINT('Ctrl Pts',(0.0576103404526291,0.065641883777369,
-0.679958486187753));
#41779=CARTESIAN_POINT('Ctrl Pts',(-0.0238804390394198,0.0840091236961439,
-0.673609595843108));
#41780=CARTESIAN_POINT('Ctrl Pts',(-0.0695554825620404,0.0392209024120294,
-0.668747681803777));
#41781=CARTESIAN_POINT('Ctrl Pts',(-0.0739138080751741,0.00737812261711985,
-0.666002064545995));
#41782=CARTESIAN_POINT('Ctrl Pts',(-0.0738538568161215,6.34559343100473E-5,
-0.665372744069761));
#41783=CARTESIAN_POINT('Origin',(0.,0.,-1.25327725593024));
#41784=CARTESIAN_POINT('',(-0.0738065481177383,4.4352265423165E-5,-0.753277255930239));
#41785=CARTESIAN_POINT('',(-0.0738499552817868,-6.25858527072351E-5,-0.745372744069761));
#41786=CARTESIAN_POINT('',(-0.0739,1.16448635408261E-14,-1.25327725593024));
#41787=CARTESIAN_POINT('Ctrl Pts',(-0.0738065481177383,4.43522654231662E-5,
-0.753277255930239));
#41788=CARTESIAN_POINT('Ctrl Pts',(-0.0737229278950059,-0.0152156401028241,
-0.751966473382609));
#41789=CARTESIAN_POINT('Ctrl Pts',(-0.06167620653198,-0.0552343787480568,
-0.74853939405343));
#41790=CARTESIAN_POINT('Ctrl Pts',(0.00385702521968538,-0.0872521164289911,
-0.742996017942701));
#41791=CARTESIAN_POINT('Ctrl Pts',(0.0753844652332581,-0.0441020505915453,
-0.736647127598059));
#41792=CARTESIAN_POINT('Ctrl Pts',(0.0779483812393019,0.0393936330776424,
-0.730298237253411));
#41793=CARTESIAN_POINT('Ctrl Pts',(0.00920324113794826,0.086851072632641,
-0.723949346908768));
#41794=CARTESIAN_POINT('Ctrl Pts',(-0.059754493504533,0.0582579636900757,
-0.718275686467709));
#41795=CARTESIAN_POINT('Ctrl Pts',(-0.0737120823041892,0.0166978694200925,
-0.714718322808199));
#41796=CARTESIAN_POINT('Ctrl Pts',(-0.0738398419805284,-5.98587458514712E-5,
-0.713277255930238));
#41797=CARTESIAN_POINT('Ctrl Pts',(-0.0738499552817868,-6.25858527072334E-5,
-0.745372744069761));
#41798=CARTESIAN_POINT('Ctrl Pts',(-0.0739100242568725,-0.00752312406464893,
-0.74473095925791));
#41799=CARTESIAN_POINT('Ctrl Pts',(-0.0694416811052649,-0.0395146377430722,
-0.74197287766451));
#41800=CARTESIAN_POINT('Ctrl Pts',(-0.0233865872476794,-0.084147939783551,
-0.737098499289559));
#41801=CARTESIAN_POINT('Ctrl Pts',(0.0579949038623966,-0.0653023687081939,
-0.730749608944917));
#41802=CARTESIAN_POINT('Ctrl Pts',(0.0863212604370854,0.0132833817028017,
-0.724400718600269));
#41803=CARTESIAN_POINT('Ctrl Pts',(0.035678849400398,0.079717174676309,
-0.718051828255625));
#41804=CARTESIAN_POINT('Ctrl Pts',(-0.0475216810321705,0.0732301507334676,
-0.711709170078789));
#41805=CARTESIAN_POINT('Ctrl Pts',(-0.0740143735713409,0.0243810905554448,
-0.707482808683501));
#41806=CARTESIAN_POINT('Ctrl Pts',(-0.0740209121467327,-1.34404130547942E-6,
-0.705372744069761));
#41807=CARTESIAN_POINT('Origin',(0.,0.,-1.25327725593024));
#41808=CARTESIAN_POINT('',(-0.074000888164484,3.46214213901279E-5,-0.793277255930238));
#41809=CARTESIAN_POINT('',(-0.0737998625275067,3.93079929045179E-5,-0.785372744069761));
#41810=CARTESIAN_POINT('',(-0.0739,1.16448635408261E-14,-1.25327725593024));
#41811=CARTESIAN_POINT('Ctrl Pts',(-0.074000888164484,3.46214213901347E-5,
-0.793277255930238));
#41812=CARTESIAN_POINT('Ctrl Pts',(-0.0738701707844107,-0.0224721008728551,
-0.791330920738565));
#41813=CARTESIAN_POINT('Ctrl Pts',(-0.0508963789367996,-0.0696818637307418,
-0.787268288765345));
#41814=CARTESIAN_POINT('Ctrl Pts',(0.0294281728820954,-0.0822301106998219,
-0.781089360010573));
#41815=CARTESIAN_POINT('Ctrl Pts',(0.0850405823393773,-0.0198974325042983,
-0.77474046966593));
#41816=CARTESIAN_POINT('Ctrl Pts',(0.0628558193470167,0.0606378960642491,
-0.768391579321283));
#41817=CARTESIAN_POINT('Ctrl Pts',(-0.0168309607139535,0.0857002171895078,
-0.762042688976639));
#41818=CARTESIAN_POINT('Ctrl Pts',(-0.0678472753579036,0.0433740631041454,
-0.757004581179623));
#41819=CARTESIAN_POINT('Ctrl Pts',(-0.0738579351916478,0.00942206414016046,
-0.754082770164157));
#41820=CARTESIAN_POINT('Ctrl Pts',(-0.0738065481177383,4.43522654231662E-5,
-0.753277255930239));
#41821=CARTESIAN_POINT('Ctrl Pts',(-0.0737998625275067,3.93079929045092E-5,
-0.785372744069761));
#41822=CARTESIAN_POINT('Ctrl Pts',(-0.0737280372000447,-0.014834695020822,
-0.784095406613867));
#41823=CARTESIAN_POINT('Ctrl Pts',(-0.0621467471385402,-0.0544548837730268,
-0.780701772376424));
#41824=CARTESIAN_POINT('Ctrl Pts',(0.00248145491972144,-0.0873020653500868,
-0.775191841357431));
#41825=CARTESIAN_POINT('Ctrl Pts',(0.0746800543932818,-0.0452846299391521,
-0.768842951012788));
#41826=CARTESIAN_POINT('Ctrl Pts',(0.0785595418575094,0.0381602753665082,
-0.762494060668141));
#41827=CARTESIAN_POINT('Ctrl Pts',(0.0105708687644261,0.0866952418906293,
-0.756145170323498));
#41828=CARTESIAN_POINT('Ctrl Pts',(-0.0592380251362248,0.0590303333329511,
-0.750438064790702));
#41829=CARTESIAN_POINT('Ctrl Pts',(-0.0737119457478501,0.0170781327974444,
-0.746847256039458));
#41830=CARTESIAN_POINT('Ctrl Pts',(-0.0738499552817868,-6.25858527072334E-5,
-0.745372744069761));
#41831=CARTESIAN_POINT('Origin',(0.,0.,-1.25327725593024));
#41832=CARTESIAN_POINT('',(-0.0739094769521497,-6.68860282600848E-5,-0.833277255930239));
#41833=CARTESIAN_POINT('',(-0.0739930868845781,4.0462490936608E-5,-0.825372744069761));
#41834=CARTESIAN_POINT('',(-0.0739,1.16448635408261E-14,-1.25327725593024));
#41835=CARTESIAN_POINT('Ctrl Pts',(-0.0739094769521496,-6.68860282600822E-5,
-0.833277255930239));
#41836=CARTESIAN_POINT('Ctrl Pts',(-0.0739592933962805,-0.005468140800202,
-0.832811664876072));
#41837=CARTESIAN_POINT('Ctrl Pts',(-0.0709543523443195,-0.0353652993575146,
-0.830229777040356));
#41838=CARTESIAN_POINT('Ctrl Pts',(-0.0302847459931343,-0.081918512102057,
-0.825531592423091));
#41839=CARTESIAN_POINT('Ctrl Pts',(0.0523793289752858,-0.0698871544776452,
-0.819182702078447));
#41840=CARTESIAN_POINT('Ctrl Pts',(0.0871255325346814,0.00607865490315511,
-0.812833811733801));
#41841=CARTESIAN_POINT('Ctrl Pts',(0.0421672010014363,0.0764835644082308,
-0.806484921389155));
#41842=CARTESIAN_POINT('Ctrl Pts',(-0.041366701368516,0.0769194675148722,
-0.800136031044511));
#41843=CARTESIAN_POINT('Ctrl Pts',(-0.0730502848478739,0.0284261194000154,
-0.795733475891537));
#41844=CARTESIAN_POINT('Ctrl Pts',(-0.074012302916597,0.00199999630665251,
-0.793447217520114));
#41845=CARTESIAN_POINT('Ctrl Pts',(-0.074000888164484,3.46214213901347E-5,
-0.793277255930238));
#41846=CARTESIAN_POINT('Ctrl Pts',(-0.0739930868845781,4.04624909366076E-5,
-0.825372744069761));
#41847=CARTESIAN_POINT('Ctrl Pts',(-0.0738471310185028,-0.0220856706569688,
-0.823459853969824));
#41848=CARTESIAN_POINT('Ctrl Pts',(-0.0515545879708975,-0.0689458471408334,
-0.819430667088338));
#41849=CARTESIAN_POINT('Ctrl Pts',(0.0281285730428364,-0.0826836840705789,
-0.813285183425303));
#41850=CARTESIAN_POINT('Ctrl Pts',(0.0847164362872849,-0.0212351985084165,
-0.80693629308066));
#41851=CARTESIAN_POINT('Ctrl Pts',(0.0638036636957854,0.0596397579799298,
-0.800587402736013));
#41852=CARTESIAN_POINT('Ctrl Pts',(-0.015478236798094,0.0859548277790816,
-0.794238512391369));
#41853=CARTESIAN_POINT('Ctrl Pts',(-0.0674983278290557,0.0441623403232539,
-0.789166959502617));
#41854=CARTESIAN_POINT('Ctrl Pts',(-0.0738470376322641,0.00980860073585892,
-0.786211703395415));
#41855=CARTESIAN_POINT('Ctrl Pts',(-0.0737998625275067,3.93079929045092E-5,
-0.785372744069761));
#41856=CARTESIAN_POINT('Origin',(0.,0.,-1.25327725593024));
#41857=CARTESIAN_POINT('',(-0.0737796652821541,8.19419257115589E-6,-0.873277255930239));
#41858=CARTESIAN_POINT('',(-0.0739212535704956,-6.56703637913897E-5,-0.865372744069761));
#41859=CARTESIAN_POINT('',(-0.0739,1.16448635408261E-14,-1.25327725593024));
#41860=CARTESIAN_POINT('Ctrl Pts',(-0.0737796652821541,8.1941925711617E-6,
-0.873277255930239));
#41861=CARTESIAN_POINT('Ctrl Pts',(-0.0737669601095564,-0.0128228898212472,
-0.872176112232029));
#41862=CARTESIAN_POINT('Ctrl Pts',(-0.0644763991334308,-0.0503313595727542,
-0.868958671752271));
#41863=CARTESIAN_POINT('Ctrl Pts',(-0.00476740193378281,-0.087207111772408,
-0.863624934490961));
#41864=CARTESIAN_POINT('Ctrl Pts',(0.0706671510291381,-0.0513221417159152,
-0.857276044146319));
#41865=CARTESIAN_POINT('Ctrl Pts',(0.0814536926085207,0.0315135593883026,
-0.850927153801671));
#41866=CARTESIAN_POINT('Ctrl Pts',(0.0177244348341756,0.0855198975367287,
-0.844578263457028));
#41867=CARTESIAN_POINT('Ctrl Pts',(-0.0563569303426115,0.063067413190051,
-0.838694964166549));
#41868=CARTESIAN_POINT('Ctrl Pts',(-0.0737328578163039,0.0190827134051602,
-0.83492796165762));
#41869=CARTESIAN_POINT('Ctrl Pts',(-0.0739094769521496,-6.68860282600822E-5,
-0.833277255930239));
#41870=CARTESIAN_POINT('Ctrl Pts',(-0.0739212535704956,-6.56703637913767E-5,
-0.865372744069761));
#41871=CARTESIAN_POINT('Ctrl Pts',(-0.0739673937800244,-0.00507688280706297,
-0.864940598107329));
#41872=CARTESIAN_POINT('Ctrl Pts',(-0.0712186382622782,-0.0345785889264521,
-0.862392155363349));
#41873=CARTESIAN_POINT('Ctrl Pts',(-0.0315720180248721,-0.081431050040796,
-0.857727415837822));
#41874=CARTESIAN_POINT('Ctrl Pts',(0.0512714030294883,-0.0707039706402494,
-0.851378525493174));
#41875=CARTESIAN_POINT('Ctrl Pts',(0.0872105100082235,0.00470480361067377,
-0.845029635148532));
#41876=CARTESIAN_POINT('Ctrl Pts',(0.0433673424553154,0.0758095102297389,
-0.838680744803884));
#41877=CARTESIAN_POINT('Ctrl Pts',(-0.040149314234986,0.0775618514436692,
-0.832331854459241));
#41878=CARTESIAN_POINT('Ctrl Pts',(-0.0728396843020035,0.0292093066790861,
-0.827895854214532));
#41879=CARTESIAN_POINT('Ctrl Pts',(-0.0740086070644259,0.0023932392242425,
-0.825576150751372));
#41880=CARTESIAN_POINT('Ctrl Pts',(-0.0739930868845781,4.04624909366076E-5,
-0.825372744069761));
#41881=CARTESIAN_POINT('Origin',(0.,0.,-1.25327725593024));
#41882=CARTESIAN_POINT('',(-0.07393952028251,6.24297301232157E-5,-0.913277255930239));
#41883=CARTESIAN_POINT('',(-0.073778853988547,1.82460500730459E-6,-0.905372744069761));
#41884=CARTESIAN_POINT('',(-0.0739,1.16448635408261E-14,-1.25327725593024));
#41885=CARTESIAN_POINT('Ctrl Pts',(-0.07393952028251,6.24297301232151E-5,
-0.913277255930239));
#41886=CARTESIAN_POINT('Ctrl Pts',(-0.0737582361283602,-0.0200636709074026,
-0.911540559587986));
#41887=CARTESIAN_POINT('Ctrl Pts',(-0.0548509230184253,-0.0650146852071005,
-0.907687566464185));
#41888=CARTESIAN_POINT('Ctrl Pts',(0.0211743841364114,-0.0847316583180511,
-0.901718276558834));
#41889=CARTESIAN_POINT('Ctrl Pts',(0.0826634734150078,-0.0281879163445984,
-0.89536938621419));
#41890=CARTESIAN_POINT('Ctrl Pts',(0.0685300267273087,0.0541428102488016,
-0.889020495869544));
#41891=CARTESIAN_POINT('Ctrl Pts',(-0.00829633857195642,0.0869423903006062,
-0.882671605524899));
#41892=CARTESIAN_POINT('Ctrl Pts',(-0.0655246901945275,0.0483110572051783,
-0.877423858878463));
#41893=CARTESIAN_POINT('Ctrl Pts',(-0.0737913782812458,0.011837272014451,
-0.874292409013577));
#41894=CARTESIAN_POINT('Ctrl Pts',(-0.0737796652821541,8.1941925711617E-6,
-0.873277255930239));
#41895=CARTESIAN_POINT('Ctrl Pts',(-0.0737788771442885,1.82425625390881E-6,
-0.905372744069761));
#41896=CARTESIAN_POINT('Ctrl Pts',(-0.0737761361603925,-0.0124398715006289,
-0.904305045463286));
#41897=CARTESIAN_POINT('Ctrl Pts',(-0.0648908980282674,-0.0495460619161376,
-0.901121050075263));
#41898=CARTESIAN_POINT('Ctrl Pts',(-0.00614119170986879,-0.0871211455233005,
-0.895820757905693));
#41899=CARTESIAN_POINT('Ctrl Pts',(0.0698495376741126,-0.0524294794902851,
-0.889471867561047));
#41900=CARTESIAN_POINT('Ctrl Pts',(0.0819402280593655,0.0302259368504705,
-0.883122977216402));
#41901=CARTESIAN_POINT('Ctrl Pts',(0.0190700247449796,0.0852299383382114,
-0.876774086871756));
#41902=CARTESIAN_POINT('Ctrl Pts',(-0.0557790826493524,0.0638267794753937,
-0.870857342489544));
#41903=CARTESIAN_POINT('Ctrl Pts',(-0.0737414368455285,0.0194639290651083,
-0.867056894888878));
#41904=CARTESIAN_POINT('Ctrl Pts',(-0.0739212535704956,-6.56703637913767E-5,
-0.865372744069761));
#41905=CARTESIAN_POINT('Origin',(0.,0.,-1.25327725593024));
#41906=CARTESIAN_POINT('',(-0.0739789826382999,-4.8665297793311E-5,-0.953277255930239));
#41907=CARTESIAN_POINT('',(-0.0739279435619739,6.46796249051864E-5,-0.94537274406976));
#41908=CARTESIAN_POINT('',(-0.0739,1.16448635408261E-14,-1.25327725593024));
#41909=CARTESIAN_POINT('Ctrl Pts',(-0.0739789826382999,-4.86652977933102E-5,
-0.953277255930239));
#41910=CARTESIAN_POINT('Ctrl Pts',(-0.0740015361495537,-0.00301071199880904,
-0.953021303725492));
#41911=CARTESIAN_POINT('Ctrl Pts',(-0.0724954516939983,-0.0304408031514225,
-0.950649054739196));
#41912=CARTESIAN_POINT('Ctrl Pts',(-0.0382166559382933,-0.0785321314734518,
-0.946160508971351));
#41913=CARTESIAN_POINT('Ctrl Pts',(0.0452310138244137,-0.0747125414725162,
-0.939811618626707));
#41914=CARTESIAN_POINT('Ctrl Pts',(0.087300263005714,-0.00254411949997818,
-0.933462728282061));
#41915=CARTESIAN_POINT('Ctrl Pts',(0.0495051294517987,0.0719517242520363,
-0.927113837937416));
#41916=CARTESIAN_POINT('Ctrl Pts',(-0.0335784885779334,0.0806243981044391,
-0.920764947592771));
#41917=CARTESIAN_POINT('Ctrl Pts',(-0.0716195454802255,0.0333433502862432,
-0.916152753590378));
#41918=CARTESIAN_POINT('Ctrl Pts',(-0.0739791446790601,0.00446151577495216,
-0.913656856369534));
#41919=CARTESIAN_POINT('Ctrl Pts',(-0.07393952028251,6.24297301232151E-5,
-0.913277255930239));
#41920=CARTESIAN_POINT('Ctrl Pts',(-0.0739279435619739,6.4679624905186E-5,
-0.94537274406976));
#41921=CARTESIAN_POINT('Ctrl Pts',(-0.0737470642738756,-0.019681810576853,
-0.943669492819243));
#41922=CARTESIAN_POINT('Ctrl Pts',(-0.0554445745886888,-0.0642593312559459,
-0.939849944787179));
#41923=CARTESIAN_POINT('Ctrl Pts',(0.0198363851821647,-0.085054841460156,
-0.933914099973564));
#41924=CARTESIAN_POINT('Ctrl Pts',(0.0822089648049221,-0.0294871893983564,
-0.927565209628919));
#41925=CARTESIAN_POINT('Ctrl Pts',(0.0693748038821494,0.0530560535586862,
-0.921216319284275));
#41926=CARTESIAN_POINT('Ctrl Pts',(-0.00692509813514159,0.0870623411626859,
-0.914867428939627));
#41927=CARTESIAN_POINT('Ctrl Pts',(-0.0651237345087083,0.0490972963047915,
-0.909586237201459));
#41928=CARTESIAN_POINT('Ctrl Pts',(-0.0737815690937712,0.0122209461942086,
-0.906421342244835));
#41929=CARTESIAN_POINT('Ctrl Pts',(-0.0737788771442885,1.82425625390881E-6,
-0.905372744069761));
#41930=CARTESIAN_POINT('Origin',(0.,0.,-1.25327725593024));
#41931=CARTESIAN_POINT('',(-0.0737911150624599,-3.07014270853876E-5,-0.993277255930239));
#41932=CARTESIAN_POINT('',(-0.0739882011667107,-4.35894684875718E-5,-0.985372744069761));
#41933=CARTESIAN_POINT('',(-0.0739,1.16448635408261E-14,-1.25327725593024));
#41934=CARTESIAN_POINT('Ctrl Pts',(-0.0737911150624599,-3.07014270853837E-5,
-0.993277255930239));
#41935=CARTESIAN_POINT('Ctrl Pts',(-0.07382999686459,-0.0104149423206292,
-0.992385751081449));
#41936=CARTESIAN_POINT('Ctrl Pts',(-0.0669337505610335,-0.0454004637637484,
-0.989377949451111));
#41937=CARTESIAN_POINT('Ctrl Pts',(-0.0133453396325877,-0.0863117047392357,
-0.984253851039223));
#41938=CARTESIAN_POINT('Ctrl Pts',(0.0652607242893321,-0.0580417636628946,
-0.977904960694579));
#41939=CARTESIAN_POINT('Ctrl Pts',(0.0841647062166166,0.0233261804187959,
-0.971556070349931));
#41940=CARTESIAN_POINT('Ctrl Pts',(0.0260727882493475,0.0833547729751633,
-0.965207180005289));
#41941=CARTESIAN_POINT('Ctrl Pts',(-0.0525676172963071,0.0677825693615826,
-0.959114241865388));
#41942=CARTESIAN_POINT('Ctrl Pts',(-0.0738150563209228,0.0214804616808422,
-0.95513760050704));
#41943=CARTESIAN_POINT('Ctrl Pts',(-0.0739789826382999,-4.86652977933102E-5,
-0.953277255930239));
#41944=CARTESIAN_POINT('Ctrl Pts',(-0.0739882011667107,-4.35894684875739E-5,
-0.985372744069761));
#41945=CARTESIAN_POINT('Ctrl Pts',(-0.0740062132812438,-0.00261774564105659,
-0.985150236956749));
#41946=CARTESIAN_POINT('Ctrl Pts',(-0.0727164539171304,-0.0296568149264066,
-0.982811433062189));
#41947=CARTESIAN_POINT('Ctrl Pts',(-0.0394495734597775,-0.077920083333527,
-0.978356332386082));
#41948=CARTESIAN_POINT('Ctrl Pts',(0.0440479277989371,-0.075416100995714,
-0.972007442041435));
#41949=CARTESIAN_POINT('Ctrl Pts',(0.0872493240631923,-0.00391965349424783,
-0.965658551696792));
#41950=CARTESIAN_POINT('Ctrl Pts',(0.0506329377619281,0.0711625874072329,
-0.959309661352143));
#41951=CARTESIAN_POINT('Ctrl Pts',(-0.032303679213407,0.0811435797963708,
-0.952960771007503));
#41952=CARTESIAN_POINT('Ctrl Pts',(-0.0713663810806487,0.0341294648344994,
-0.948315131913371));
#41953=CARTESIAN_POINT('Ctrl Pts',(-0.073971807543628,0.00485328584428242,
-0.945785789600792));
#41954=CARTESIAN_POINT('Ctrl Pts',(-0.0739279435619739,6.4679624905186E-5,
-0.94537274406976));
#41955=CARTESIAN_POINT('Origin',(0.,0.,-1.25327725593024));
#41956=CARTESIAN_POINT('',(-0.073866824948156,6.56932150246621E-5,-1.03327725593024));
#41957=CARTESIAN_POINT('',(-0.0737964283105518,-3.62685935665213E-5,-1.02537274406976));
#41958=CARTESIAN_POINT('',(-0.0739,1.16448635408261E-14,-1.25327725593024));
#41959=CARTESIAN_POINT('Ctrl Pts',(-0.073866824948156,6.56932150246616E-5,
-1.03327725593024));
#41960=CARTESIAN_POINT('Ctrl Pts',(-0.0737142120031003,-0.0176755814077243,
-1.03175019843741));
#41961=CARTESIAN_POINT('Ctrl Pts',(-0.058407180002613,-0.0602401901634181,
-1.02810684416302));
#41962=CARTESIAN_POINT('Ctrl Pts',(0.0127141134428745,-0.0864069431030045,
-1.0223471931071));
#41963=CARTESIAN_POINT('Ctrl Pts',(0.0794802692010834,-0.0362035249468621,
-1.01599830276245));
#41964=CARTESIAN_POINT('Ctrl Pts',(0.0735359619677752,0.0471197494086118,
-1.0096494124178));
#41965=CARTESIAN_POINT('Ctrl Pts',(0.000319185439644519,0.0873367424855461,
-1.00330052207316));
#41966=CARTESIAN_POINT('Ctrl Pts',(-0.0628675604855332,0.0532279134888255,
-0.997843136577303));
#41967=CARTESIAN_POINT('Ctrl Pts',(-0.0737376973859944,0.0142356645848239,
-0.994502047862997));
#41968=CARTESIAN_POINT('Ctrl Pts',(-0.0737911150624599,-3.07014270853837E-5,
-0.993277255930239));
#41969=CARTESIAN_POINT('Ctrl Pts',(-0.0737964283105518,-3.62685935665187E-5,
-1.02537274406976));
#41970=CARTESIAN_POINT('Ctrl Pts',(-0.073840823994672,-0.0100291409910542,
-1.02451468431271));
#41971=CARTESIAN_POINT('Ctrl Pts',(-0.0672954261095734,-0.0446124579298668,
-1.0215403277741));
#41972=CARTESIAN_POINT('Ctrl Pts',(-0.0147039522670727,-0.0860906616485553,
-1.01644967445395));
#41973=CARTESIAN_POINT('Ctrl Pts',(0.0643378813590148,-0.0590630616174244,
-1.01010078410931));
#41974=CARTESIAN_POINT('Ctrl Pts',(0.0845218720571315,0.0219968493309595,
-1.00375189376466));
#41975=CARTESIAN_POINT('Ctrl Pts',(0.0273832188795813,0.0829335128685668,
-0.997403003420017));
#41976=CARTESIAN_POINT('Ctrl Pts',(-0.0519257991877054,0.0685239498085602,
-0.991276620188384));
#41977=CARTESIAN_POINT('Ctrl Pts',(-0.0738348974994724,0.0218654196361237,
-0.987266533738298));
#41978=CARTESIAN_POINT('Ctrl Pts',(-0.0739882011667107,-4.35894684875739E-5,
-0.985372744069761));
#41979=CARTESIAN_POINT('Origin',(0.,0.,-1.25327725593024));
#41980=CARTESIAN_POINT('',(-0.0740192616259655,-9.94807855793969E-6,-1.07327725593024));
#41981=CARTESIAN_POINT('',(-0.0738559566843222,6.38844806161408E-5,-1.06537274406976));
#41982=CARTESIAN_POINT('',(-0.0739,1.16448635408261E-14,-1.25327725593024));
#41983=CARTESIAN_POINT('Ctrl Pts',(-0.0740192616259655,-9.94807855795362E-6,
-1.07327725593024));
#41984=CARTESIAN_POINT('Ctrl Pts',(-0.074020272762249,-0.0005451446973743,
-1.07323094257491));
#41985=CARTESIAN_POINT('Ctrl Pts',(-0.0737726260818757,-0.0255352823793165,
-1.07106833243804));
#41986=CARTESIAN_POINT('Ctrl Pts',(-0.0457759481553394,-0.074379934125127,
-1.06678942551961));
#41987=CARTESIAN_POINT('Ctrl Pts',(0.037641655214997,-0.0788093717621258,
-1.06044053517497));
#41988=CARTESIAN_POINT('Ctrl Pts',(0.0866236680057719,-0.0111420824567537,
-1.05409164483032));
#41989=CARTESIAN_POINT('Ctrl Pts',(0.0563603151316931,0.0667182437528911,
-1.04774275448568));
#41990=CARTESIAN_POINT('Ctrl Pts',(-0.0254628383918398,0.0835431184830735,
-1.04139386414103));
#41991=CARTESIAN_POINT('Ctrl Pts',(-0.0699143291817533,0.0382765099988127,
-1.03657203128922));
#41992=CARTESIAN_POINT('Ctrl Pts',(-0.0739257130670484,0.0069114446609779,
-1.03386649521896));
#41993=CARTESIAN_POINT('Ctrl Pts',(-0.073866824948156,6.56932150246616E-5,
-1.03327725593024));
#41994=CARTESIAN_POINT('Ctrl Pts',(-0.0738559566843223,6.38844806161391E-5,
-1.06537274406976));
#41995=CARTESIAN_POINT('Ctrl Pts',(-0.0737124056741182,-0.0172952975271126,
-1.06387913166866));
#41996=CARTESIAN_POINT('Ctrl Pts',(-0.0589387738984228,-0.0594706446064186,
-1.06026922248602));
#41997=CARTESIAN_POINT('Ctrl Pts',(0.0113507662365832,-0.0865965857232952,
-1.05454301652183));
#41998=CARTESIAN_POINT('Ctrl Pts',(0.0788998284283993,-0.0374516345044027,
-1.04819412617718));
#41999=CARTESIAN_POINT('Ctrl Pts',(0.0742694349891011,0.045954971304813,
-1.04184523583253));
#42000=CARTESIAN_POINT('Ctrl Pts',(0.00169557022275755,0.087320864097371,
-1.03549634548789));
#42001=CARTESIAN_POINT('Ctrl Pts',(-0.062411361346758,0.0540091890348234,
-1.0300055149003));
#42002=CARTESIAN_POINT('Ctrl Pts',(-0.0737313276074497,0.0146170255717787,
-1.02663098109426));
#42003=CARTESIAN_POINT('Ctrl Pts',(-0.0737964283105518,-3.62685935665187E-5,
-1.02537274406976));
#42004=CARTESIAN_POINT('Origin',(0.,0.,-1.25327725593024));
#42005=CARTESIAN_POINT('',(-0.0738384445906279,-5.9163082798582E-5,-1.11327725593024));
#42006=CARTESIAN_POINT('',(-0.0740206415646085,-2.83210792082628E-6,-1.10537274406976));
#42007=CARTESIAN_POINT('',(-0.0739,1.16448635408261E-14,-1.25327725593024));
#42008=CARTESIAN_POINT('Ctrl Pts',(-0.0738384445906279,-5.91630827985745E-5,
-1.11327725593024));
#42009=CARTESIAN_POINT('Ctrl Pts',(-0.0738974492120266,-0.0079890193914202,
-1.11259538993087));
#42010=CARTESIAN_POINT('Ctrl Pts',(-0.0690655000923834,-0.0404598186853639,
-1.10979722714995));
#42011=CARTESIAN_POINT('Ctrl Pts',(-0.0217956051609413,-0.0845742251201784,
-1.10488276758748));
#42012=CARTESIAN_POINT('Ctrl Pts',(0.0592192057513427,-0.0641956017183869,
-1.09853387724284));
#42013=CARTESIAN_POINT('Ctrl Pts',(0.0860543001947688,0.0149114473055614,
-1.09218498689819));
#42014=CARTESIAN_POINT('Ctrl Pts',(0.0341672535616166,0.0803767533194929,
-1.08583609655355));
#42015=CARTESIAN_POINT('Ctrl Pts',(-0.048371565664984,0.0723705090856044,
-1.07953351956423));
#42016=CARTESIAN_POINT('Ctrl Pts',(-0.0739740687148976,0.0239107573613757,
-1.07534723935646));
#42017=CARTESIAN_POINT('Ctrl Pts',(-0.0740192616259655,-9.94807855795362E-6,
-1.07327725593024));
#42018=CARTESIAN_POINT('Ctrl Pts',(-0.0740206415646085,-2.8321079208263E-6,
-1.10537274406976));
#42019=CARTESIAN_POINT('Ctrl Pts',(-0.074020722247648,-0.000151529651826495,
-1.10535987580617));
#42020=CARTESIAN_POINT('Ctrl Pts',(-0.0739528370466597,-0.0247547414900179,
-1.10323071076103));
#42021=CARTESIAN_POINT('Ctrl Pts',(-0.0469427823151367,-0.0736491592978005,
-1.09898524893434));
#42022=CARTESIAN_POINT('Ctrl Pts',(0.0363951010157612,-0.07939287134855,
-1.09263635858969));
#42023=CARTESIAN_POINT('Ctrl Pts',(0.0864372276420334,-0.0125058552883607,
-1.08628746824505));
#42024=CARTESIAN_POINT('Ctrl Pts',(0.0574048355464994,0.0658217035478255,
-1.0799385779004));
#42025=CARTESIAN_POINT('Ctrl Pts',(-0.0241430608589063,0.0839340435518515,
-1.07358968755576));
#42026=CARTESIAN_POINT('Ctrl Pts',(-0.0696156377881968,0.0390645232381797,
-1.06873440961221));
#42027=CARTESIAN_POINT('Ctrl Pts',(-0.0739158028477489,0.00730089689808365,
-1.06599542845021));
#42028=CARTESIAN_POINT('Ctrl Pts',(-0.0738559566843223,6.38844806161391E-5,
-1.06537274406976));
#42029=CARTESIAN_POINT('Origin',(0.,0.,-1.25327725593024));
#42030=CARTESIAN_POINT('',(-0.0739,1.16448635408261E-14,-1.149325));
#42031=CARTESIAN_POINT('',(-0.0738510899558415,-6.10647340483564E-5,-1.14537274406976));
#42032=CARTESIAN_POINT('',(-0.0739,1.16448635408261E-14,-1.25327725593024));
#42033=CARTESIAN_POINT('',(-0.060110435027941,-0.0429877377952328,-1.149325));
#42034=CARTESIAN_POINT('Origin',(0.,0.,-1.149325));
#42035=CARTESIAN_POINT('Ctrl Pts',(-0.0601104350279426,-0.0429877377952305,
-1.149325));
#42036=CARTESIAN_POINT('Ctrl Pts',(-0.0458201451106566,-0.0629700766588213,
-1.14720870321845));
#42037=CARTESIAN_POINT('Ctrl Pts',(0.00400364749018219,-0.0872208216030551,
-1.14297610965536));
#42038=CARTESIAN_POINT('Ctrl Pts',(0.075583875527885,-0.0438759620050528,
-1.13662721931071));
#42039=CARTESIAN_POINT('Ctrl Pts',(0.0777927499997916,0.0396423987382078,
-1.13027832896607));
#42040=CARTESIAN_POINT('Ctrl Pts',(0.00894843417834478,0.0868766870214709,
-1.12392943862142));
#42041=CARTESIAN_POINT('Ctrl Pts',(-0.0598619431359153,0.0581055068125897,
-1.11826241427615));
#42042=CARTESIAN_POINT('Ctrl Pts',(-0.0737143174962966,0.0166227509558038,
-1.11471168671242));
#42043=CARTESIAN_POINT('Ctrl Pts',(-0.0738384445906279,-5.91630827985745E-5,
-1.11327725593024));
#42044=CARTESIAN_POINT('Ctrl Pts',(-0.0738510899558415,-6.10647340483625E-5,
-1.14537274406976));
#42045=CARTESIAN_POINT('Ctrl Pts',(-0.0739066365669056,-0.00760080692696395,
-1.14472432316213));
#42046=CARTESIAN_POINT('Ctrl Pts',(-0.0693607406337676,-0.0396777682903678,
-1.14195960547294));
#42047=CARTESIAN_POINT('Ctrl Pts',(-0.0231394877402551,-0.0842151856723098,
-1.13707859100221));
#42048=CARTESIAN_POINT('Ctrl Pts',(0.0582073462645349,-0.0651235753210661,
-1.13072970065757));
#42049=CARTESIAN_POINT('Ctrl Pts',(0.0862748105718152,0.0135547808574791,
-1.12438081031292));
#42050=CARTESIAN_POINT('Ctrl Pts',(0.0354317513839886,0.0798275566707828,
-1.11803191996827));
#42051=CARTESIAN_POINT('Ctrl Pts',(-0.0476646650497281,0.0730886637154228,
-1.11169589788723));
#42052=CARTESIAN_POINT('Ctrl Pts',(-0.0740074532268815,0.0243030621703926,
-1.10747617258772));
#42053=CARTESIAN_POINT('Ctrl Pts',(-0.0740206415646085,-2.8321079208263E-6,
-1.10537274406976));
#42054=CARTESIAN_POINT('Origin',(2.39206768658147E-17,-5.43753587379397E-18,
-0.013325));
#42055=CARTESIAN_POINT('',(-0.0452560140322605,0.0854280329804675,-0.013325));
#42056=CARTESIAN_POINT('Ctrl Pts',(0.0740200992814443,-0.000529165593927905,
-0.013325));
#42057=CARTESIAN_POINT('Ctrl Pts',(0.0743044627852839,0.00121921260606306,
-0.013325));
#42058=CARTESIAN_POINT('Ctrl Pts',(0.0745210416674805,0.00297514272191292,
-0.0133249999999998));
#42059=CARTESIAN_POINT('Ctrl Pts',(0.0746683292766584,0.00473514820652526,
-0.0133249999999998));
#42060=CARTESIAN_POINT('Ctrl Pts',(0.0750051149292103,0.00875955052345067,
-0.0133249999999999));
#42061=CARTESIAN_POINT('Ctrl Pts',(0.0749803322318632,0.0128050196487043,
-0.0133250000000001));
#42062=CARTESIAN_POINT('Ctrl Pts',(0.0746223571827205,0.0168365255250177,
-0.0133250000000001));
#42063=CARTESIAN_POINT('Ctrl Pts',(0.0743701515064359,0.0196768594209578,
-0.0133250000000001));
#42064=CARTESIAN_POINT('Ctrl Pts',(0.073951828239943,0.0225100795751238,
-0.0133250000000001));
#42065=CARTESIAN_POINT('Ctrl Pts',(0.0733791204930561,0.0253103719483463,
-0.0133250000000002));
#42066=CARTESIAN_POINT('Ctrl Pts',(0.0725805310638456,0.029215127733666,
-0.0133250000000003));
#42067=CARTESIAN_POINT('Ctrl Pts',(0.0714817005281231,0.0330626442864868,
-0.0133250000000001));
#42068=CARTESIAN_POINT('Ctrl Pts',(0.0701052438006905,0.0368218413152237,
-0.013325));
#42069=CARTESIAN_POINT('Ctrl Pts',(0.0691330418171139,0.0394769911177245,
-0.0133249999999999));
#42070=CARTESIAN_POINT('Ctrl Pts',(0.068021277102673,0.0420888634409962,
-0.0133249999999998));
#42071=CARTESIAN_POINT('Ctrl Pts',(0.0667846606791258,0.0446313284838127,
-0.0133249999999998));
#42072=CARTESIAN_POINT('Ctrl Pts',(0.063828770169334,0.0507085955720025,
-0.013325));
#42073=CARTESIAN_POINT('Ctrl Pts',(0.0601564831066114,0.0564106861323656,
-0.013325));
#42074=CARTESIAN_POINT('Ctrl Pts',(0.0558589764451619,0.061596620111266,
-0.0133249999999998));
#42075=CARTESIAN_POINT('Ctrl Pts',(0.054311387560419,0.0634641434020967,
-0.0133249999999997));
#42076=CARTESIAN_POINT('Ctrl Pts',(0.0526804759702182,0.06526640368048,
-0.0133249999999999));
#42077=CARTESIAN_POINT('Ctrl Pts',(0.0509747383512297,0.066990486897638,
-0.0133249999999999));
#42078=CARTESIAN_POINT('Ctrl Pts',(0.048133402035997,0.0698623824347133,
-0.0133249999999999));
#42079=CARTESIAN_POINT('Ctrl Pts',(0.0450946231233207,0.0725083069172221,
-0.0133250000000003));
#42080=CARTESIAN_POINT('Ctrl Pts',(0.0418777543778179,0.074900292157355,
-0.0133250000000002));
#42081=CARTESIAN_POINT('Ctrl Pts',(0.0376846139865073,0.0780182092125168,
-0.0133250000000001));
#42082=CARTESIAN_POINT('Ctrl Pts',(0.0331893030001897,0.0807054966328726,
-0.0133249999999999));
#42083=CARTESIAN_POINT('Ctrl Pts',(0.0284599480374241,0.0829678801923137,
-0.0133249999999997));
#42084=CARTESIAN_POINT('Ctrl Pts',(0.0255937901488642,0.0843389653692335,
-0.0133249999999996));
#42085=CARTESIAN_POINT('Ctrl Pts',(0.022637959968407,0.085554329703683,
-0.0133249999999998));
#42086=CARTESIAN_POINT('Ctrl Pts',(0.0196310938735226,0.0866056603112436,
-0.0133249999999998));
#42087=CARTESIAN_POINT('Ctrl Pts',(0.0144385045732225,0.0884212144103054,
-0.0133249999999999));
#42088=CARTESIAN_POINT('Ctrl Pts',(0.00908161914042202,0.0897557224136673,
-0.0133249999999999));
#42089=CARTESIAN_POINT('Ctrl Pts',(0.00363540148731718,0.0906157263666272,
-0.0133249999999999));
#42090=CARTESIAN_POINT('Ctrl Pts',(-0.000357205864503874,0.0912461929259696,
-0.0133249999999998));
#42091=CARTESIAN_POINT('Ctrl Pts',(-0.00439819318417859,0.0916213813352182,
-0.0133250000000001));
#42092=CARTESIAN_POINT('Ctrl Pts',(-0.00846098990337325,0.0917385588593169,
-0.013325));
#42093=CARTESIAN_POINT('Ctrl Pts',(-0.0113225184174696,0.0918210898963328,
-0.013325));
#42094=CARTESIAN_POINT('Ctrl Pts',(-0.0141871645686146,0.0917750525558502,
-0.0133250000000003));
#42095=CARTESIAN_POINT('Ctrl Pts',(-0.0170374024637594,0.0916013767188937,
-0.0133250000000002));
#42096=CARTESIAN_POINT('Ctrl Pts',(-0.0245300683346267,0.0911448200860685,
-0.013325));
#42097=CARTESIAN_POINT('Ctrl Pts',(-0.0319391506798941,0.0898104051975574,
-0.0133250000000003));
#42098=CARTESIAN_POINT('Ctrl Pts',(-0.0390995076077797,0.0875866732068192,
-0.0133250000000004));
#42099=CARTESIAN_POINT('Ctrl Pts',(-0.0411738518072883,0.0869424615281688,
-0.0133250000000005));
#42100=CARTESIAN_POINT('Ctrl Pts',(-0.0432273660238442,0.086223285901193,
-0.013325));
#42101=CARTESIAN_POINT('Ctrl Pts',(-0.0452560140322605,0.0854280329804675,
-0.013325));
#42102=CARTESIAN_POINT('',(-0.096675,-1.1839272930757E-17,-0.013325));
#42103=CARTESIAN_POINT('Origin',(0.,0.,-0.013325));
#42104=CARTESIAN_POINT('',(-0.0953132884602481,0.016639320268274,-0.013325));
#42105=CARTESIAN_POINT('Origin',(0.,0.,-0.013325));
#42106=CARTESIAN_POINT('Ctrl Pts',(-0.0953948120465086,0.0166363274765932,
-0.013325));
#42107=CARTESIAN_POINT('Ctrl Pts',(-0.0955400881374255,0.0143581077064726,
-0.013325));
#42108=CARTESIAN_POINT('Ctrl Pts',(-0.0955985924312004,0.0120778234632231,
-0.0133249999999999));
#42109=CARTESIAN_POINT('Ctrl Pts',(-0.0955674386515142,0.00979904378813855,
-0.0133249999999999));
#42110=CARTESIAN_POINT('Ctrl Pts',(-0.0954981213062938,0.00472874544841861,
-0.013325));
#42111=CARTESIAN_POINT('Ctrl Pts',(-0.0949855510048348,-0.000334448640519777,
-0.0133250000000001));
#42112=CARTESIAN_POINT('Ctrl Pts',(-0.0940540581382921,-0.00534172392063533,
-0.0133250000000002));
#42113=CARTESIAN_POINT('Ctrl Pts',(-0.0934623572121308,-0.00852243472069274,
-0.0133250000000003));
#42114=CARTESIAN_POINT('Ctrl Pts',(-0.0927007925980538,-0.0116809531331341,
-0.0133250000000003));
#42115=CARTESIAN_POINT('Ctrl Pts',(-0.0917795646923028,-0.0147890698658072,
-0.0133250000000002));
#42116=CARTESIAN_POINT('Ctrl Pts',(-0.0902526281395622,-0.0199407777327483,
-0.0133250000000002));
#42117=CARTESIAN_POINT('Ctrl Pts',(-0.088286029031168,-0.0249651054813939,
-0.013325));
#42118=CARTESIAN_POINT('Ctrl Pts',(-0.0859055131334032,-0.029799907615255,
-0.013325));
#42119=CARTESIAN_POINT('Ctrl Pts',(-0.0846952816011176,-0.0322578748148248,
-0.013325));
#42120=CARTESIAN_POINT('Ctrl Pts',(-0.0833776616024067,-0.0346663040964685,
-0.0133250000000004));
#42121=CARTESIAN_POINT('Ctrl Pts',(-0.0819632215061403,-0.037004905631243,
-0.0133250000000004));
#42122=CARTESIAN_POINT('Ctrl Pts',(-0.0783562873120896,-0.0429685246380169,
-0.0133250000000003));
#42123=CARTESIAN_POINT('Ctrl Pts',(-0.0741117287112331,-0.0485023320358176,
-0.0133250000000002));
#42124=CARTESIAN_POINT('Ctrl Pts',(-0.0692831287782071,-0.0534603643174138,
-0.0133250000000004));
#42125=CARTESIAN_POINT('Ctrl Pts',(-0.0675298846535145,-0.0552606047780678,
-0.0133250000000004));
#42126=CARTESIAN_POINT('Ctrl Pts',(-0.0656994071220876,-0.0569845310122871,
-0.013325));
#42127=CARTESIAN_POINT('Ctrl Pts',(-0.0637936345292532,-0.0586235633435691,
-0.013325));
#42128=CARTESIAN_POINT('Ctrl Pts',(-0.0618569431530899,-0.0602891869301303,
-0.013325));
#42129=CARTESIAN_POINT('Ctrl Pts',(-0.0598492146310193,-0.0618612346315886,
-0.013325));
#42130=CARTESIAN_POINT('Ctrl Pts',(-0.0577760214915456,-0.0633304149469573,
-0.013325));
#42131=CARTESIAN_POINT('Ctrl Pts',(-0.0562706950449255,-0.0643971732443243,
-0.0133249999999999));
#42132=CARTESIAN_POINT('Ctrl Pts',(-0.0547304006007948,-0.0654100638618711,
-0.013325));
#42133=CARTESIAN_POINT('Ctrl Pts',(-0.053156133026322,-0.0663660545506018,
-0.013325));
#42134=CARTESIAN_POINT('Ctrl Pts',(-0.0496177962615322,-0.0685147470953649,
-0.013325));
#42135=CARTESIAN_POINT('Ctrl Pts',(-0.0459078250945438,-0.0703764577179876,
-0.0133249999999997));
#42136=CARTESIAN_POINT('Ctrl Pts',(-0.0420623737642596,-0.0719462705416227,
-0.0133249999999998));
#42137=CARTESIAN_POINT('Ctrl Pts',(-0.0395974908876075,-0.0729524995681232,
-0.0133249999999998));
#42138=CARTESIAN_POINT('Ctrl Pts',(-0.0370748935076417,-0.0738392450007706,
-0.0133249999999998));
#42139=CARTESIAN_POINT('Ctrl Pts',(-0.0345107759053943,-0.0746018375885252,
-0.0133249999999998));
#42140=CARTESIAN_POINT('Ctrl Pts',(-0.0281794651533031,-0.0764848286986382,
-0.0133249999999996));
#42141=CARTESIAN_POINT('Ctrl Pts',(-0.0216430486600933,-0.0776015958572515,
-0.0133249999999997));
#42142=CARTESIAN_POINT('Ctrl Pts',(-0.0150531338947347,-0.0779342001631726,
-0.0133249999999997));
#42143=CARTESIAN_POINT('Ctrl Pts',(-0.0120753298759454,-0.0780844950416504,
-0.0133249999999997));
#42144=CARTESIAN_POINT('Ctrl Pts',(-0.00908668828005284,-0.0780739840860596,
-0.0133249999999997));
#42145=CARTESIAN_POINT('Ctrl Pts',(-0.00610252359415805,-0.0778977331119931,
-0.0133249999999997));
#42146=CARTESIAN_POINT('Ctrl Pts',(-0.00399701693690746,-0.0777733775089,
-0.0133249999999997));
#42147=CARTESIAN_POINT('Ctrl Pts',(-0.0018959538125692,-0.0775663788512026,
-0.0133249999999997));
#42148=CARTESIAN_POINT('Ctrl Pts',(0.000186776601496543,-0.0772767405557303,
-0.0133249999999997));
#42149=CARTESIAN_POINT('Ctrl Pts',(0.00624411631421537,-0.076434366747944,
-0.0133249999999998));
#42150=CARTESIAN_POINT('Ctrl Pts',(0.0121700652423237,-0.0748949340523382,
-0.0133249999999999));
#42151=CARTESIAN_POINT('Ctrl Pts',(0.0178272270255753,-0.0726202066517544,
-0.0133250000000001));
#42152=CARTESIAN_POINT('Ctrl Pts',(0.0197042518379329,-0.0718654607321863,
-0.0133250000000002));
#42153=CARTESIAN_POINT('Ctrl Pts',(0.021551428218358,-0.0710294440312932,
-0.013325));
#42154=CARTESIAN_POINT('Ctrl Pts',(0.0233628051714112,-0.0701098376443897,
-0.013325));
#42155=CARTESIAN_POINT('Ctrl Pts',(0.0663714283216862,0.032496822960703,
-1.16247415238079));
#42156=CARTESIAN_POINT('Ctrl Pts',(0.0555686030204049,0.0545604858000743,
-1.16035785559925));
#42157=CARTESIAN_POINT('Ctrl Pts',(0.0104211156604289,0.0866885407409115,
-1.15612526203615));
#42158=CARTESIAN_POINT('Ctrl Pts',(-0.0673222376269667,0.0557291632982185,
-1.1497763716915));
#42159=CARTESIAN_POINT('Ctrl Pts',(-0.0832609374865553,-0.0262839541860632,
-1.14342748134686));
#42160=CARTESIAN_POINT('Ctrl Pts',(-0.0231394877402551,-0.0842151856723098,
-1.13707859100221));
#42161=CARTESIAN_POINT('Ctrl Pts',(0.0582073462645349,-0.0651235753210661,
-1.13072970065757));
#42162=CARTESIAN_POINT('Ctrl Pts',(0.0862748105718152,0.0135547808574791,
-1.12438081031292));
#42163=CARTESIAN_POINT('Ctrl Pts',(0.0354317513839886,0.0798275566707828,
-1.11803191996827));
#42164=CARTESIAN_POINT('Ctrl Pts',(-0.0478334312845205,0.0730749772336279,
-1.11168302962363));
#42165=CARTESIAN_POINT('Ctrl Pts',(-0.0873350606334346,-0.000529835700201266,
-1.10533413927899));
#42166=CARTESIAN_POINT('Ctrl Pts',(-0.0469427823151367,-0.0736491592978005,
-1.09898524893434));
#42167=CARTESIAN_POINT('Ctrl Pts',(0.0363951010157612,-0.07939287134855,
-1.09263635858969));
#42168=CARTESIAN_POINT('Ctrl Pts',(0.0864372276420334,-0.0125058552883607,
-1.08628746824505));
#42169=CARTESIAN_POINT('Ctrl Pts',(0.0574048355464994,0.0658217035478255,
-1.0799385779004));
#42170=CARTESIAN_POINT('Ctrl Pts',(-0.0241430608589063,0.0839340435518515,
-1.07358968755576));
#42171=CARTESIAN_POINT('Ctrl Pts',(-0.0836042097301358,0.0252614675221138,
-1.06724079721112));
#42172=CARTESIAN_POINT('Ctrl Pts',(-0.0665822640251934,-0.0565208904508504,
-1.06089190686647));
#42173=CARTESIAN_POINT('Ctrl Pts',(0.0113507662365832,-0.0865965857232952,
-1.05454301652183));
#42174=CARTESIAN_POINT('Ctrl Pts',(0.0788998284283993,-0.0374516345044027,
-1.04819412617718));
#42175=CARTESIAN_POINT('Ctrl Pts',(0.0742694349891011,0.045954971304813,
-1.04184523583253));
#42176=CARTESIAN_POINT('Ctrl Pts',(0.00169557022275755,0.087320864097371,
-1.03549634548789));
#42177=CARTESIAN_POINT('Ctrl Pts',(-0.0724294409889089,0.0488035270943797,
-1.02914745514324));
#42178=CARTESIAN_POINT('Ctrl Pts',(-0.0802942565935507,-0.034360451292179,
-1.0227985647986));
#42179=CARTESIAN_POINT('Ctrl Pts',(-0.0147039522670727,-0.0860906616485553,
-1.01644967445395));
#42180=CARTESIAN_POINT('Ctrl Pts',(0.0643378813590148,-0.0590630616174244,
-1.01010078410931));
#42181=CARTESIAN_POINT('Ctrl Pts',(0.0845218720571315,0.0219968493309595,
-1.00375189376466));
#42182=CARTESIAN_POINT('Ctrl Pts',(0.0273832188795813,0.0829335128685668,
-0.997403003420017));
#42183=CARTESIAN_POINT('Ctrl Pts',(-0.0548062622568154,0.0680006018306399,
-0.991054113075372));
#42184=CARTESIAN_POINT('Ctrl Pts',(-0.086857655002089,-0.00914089716737991,
-0.984705222730726));
#42185=CARTESIAN_POINT('Ctrl Pts',(-0.0394495734597775,-0.077920083333527,
-0.978356332386082));
#42186=CARTESIAN_POINT('Ctrl Pts',(0.0440479277989371,-0.075416100995714,
-0.972007442041435));
#42187=CARTESIAN_POINT('Ctrl Pts',(0.0872493240631923,-0.00391965349424783,
-0.965658551696792));
#42188=CARTESIAN_POINT('Ctrl Pts',(0.0506329377619281,0.0711625874072329,
-0.959309661352143));
#42189=CARTESIAN_POINT('Ctrl Pts',(-0.032303679213407,0.0811435797963708,
-0.952960771007503));
#42190=CARTESIAN_POINT('Ctrl Pts',(-0.0856881125918317,0.0168924714998301,
-0.946611880662853));
#42191=CARTESIAN_POINT('Ctrl Pts',(-0.0606829972532737,-0.0628122764852983,
-0.940262990318211));
#42192=CARTESIAN_POINT('Ctrl Pts',(0.0198363851821647,-0.085054841460156,
-0.933914099973564));
#42193=CARTESIAN_POINT('Ctrl Pts',(0.0822089648049221,-0.0294871893983564,
-0.927565209628919));
#42194=CARTESIAN_POINT('Ctrl Pts',(0.0693748038821494,0.0530560535586862,
-0.921216319284275));
#42195=CARTESIAN_POINT('Ctrl Pts',(-0.00692509813514159,0.0870623411626859,
-0.914867428939627));
#42196=CARTESIAN_POINT('Ctrl Pts',(-0.0768897536262579,0.0414219026627595,
-0.908518538594985));
#42197=CARTESIAN_POINT('Ctrl Pts',(-0.0765138110414937,-0.042112289807323,
-0.902169648250337));
#42198=CARTESIAN_POINT('Ctrl Pts',(-0.00614119170986879,-0.0871211455233005,
-0.895820757905693));
#42199=CARTESIAN_POINT('Ctrl Pts',(0.0698495376741126,-0.0524294794902851,
-0.889471867561047));
#42200=CARTESIAN_POINT('Ctrl Pts',(0.0819402280593655,0.0302259368504705,
-0.883122977216402));
#42201=CARTESIAN_POINT('Ctrl Pts',(0.0190700247449796,0.0852299383382114,
-0.876774086871756));
#42202=CARTESIAN_POINT('Ctrl Pts',(-0.061245896400729,0.0622635399489994,
-0.870425196527112));
#42203=CARTESIAN_POINT('Ctrl Pts',(-0.0855325967550582,-0.0176630440537883,
-0.864076306182466));
#42204=CARTESIAN_POINT('Ctrl Pts',(-0.0315720180248721,-0.081431050040796,
-0.857727415837822));
#42205=CARTESIAN_POINT('Ctrl Pts',(0.0512714030294883,-0.0707039706402494,
-0.851378525493174));
#42206=CARTESIAN_POINT('Ctrl Pts',(0.0872105100082235,0.00470480361067377,
-0.845029635148532));
#42207=CARTESIAN_POINT('Ctrl Pts',(0.0433673424553154,0.0758095102297389,
-0.838680744803884));
#42208=CARTESIAN_POINT('Ctrl Pts',(-0.040149314234986,0.0775618514436692,
-0.832331854459241));
#42209=CARTESIAN_POINT('Ctrl Pts',(-0.0869364114920166,0.00835874331464967,
-0.825982964114595));
#42210=CARTESIAN_POINT('Ctrl Pts',(-0.0541919861401563,-0.0684911444720746,
-0.819634073769949));
#42211=CARTESIAN_POINT('Ctrl Pts',(0.0281285730428364,-0.0826836840705789,
-0.813285183425303));
#42212=CARTESIAN_POINT('Ctrl Pts',(0.0847164362872849,-0.0212351985084165,
-0.80693629308066));
#42213=CARTESIAN_POINT('Ctrl Pts',(0.0638036636957854,0.0596397579799298,
-0.800587402736013));
#42214=CARTESIAN_POINT('Ctrl Pts',(-0.015478236798094,0.0859548277790816,
-0.794238512391369));
#42215=CARTESIAN_POINT('Ctrl Pts',(-0.0806002735625345,0.033636351385875,
-0.787889622046722));
#42216=CARTESIAN_POINT('Ctrl Pts',(-0.0719872392663277,-0.0494534691980449,
-0.781540731702079));
#42217=CARTESIAN_POINT('Ctrl Pts',(0.00248145491972144,-0.0873020653500868,
-0.775191841357431));
#42218=CARTESIAN_POINT('Ctrl Pts',(0.0746800543932818,-0.0452846299391521,
-0.768842951012788));
#42219=CARTESIAN_POINT('Ctrl Pts',(0.0785595418575094,0.0381602753665082,
-0.762494060668141));
#42220=CARTESIAN_POINT('Ctrl Pts',(0.0105708687644261,0.0866952418906293,
-0.756145170323498));
#42221=CARTESIAN_POINT('Ctrl Pts',(-0.0670882896144543,0.0559193135644258,
-0.749796279978851));
#42222=CARTESIAN_POINT('Ctrl Pts',(-0.0833734652087589,-0.0260129493136267,
-0.743447389634208));
#42223=CARTESIAN_POINT('Ctrl Pts',(-0.0233865872476794,-0.084147939783551,
-0.737098499289559));
#42224=CARTESIAN_POINT('Ctrl Pts',(0.0579949038623966,-0.0653023687081939,
-0.730749608944917));
#42225=CARTESIAN_POINT('Ctrl Pts',(0.0863212604370854,0.0132833817028017,
-0.724400718600269));
#42226=CARTESIAN_POINT('Ctrl Pts',(0.035678849400398,0.079717174676309,
-0.718051828255625));
#42227=CARTESIAN_POINT('Ctrl Pts',(-0.0476034321928007,0.0732237767147732,
-0.71170293791098));
#42228=CARTESIAN_POINT('Ctrl Pts',(-0.0873369477542859,-0.00025649536951448,
-0.705354047566334));
#42229=CARTESIAN_POINT('Ctrl Pts',(-0.047172520489486,-0.0735021193135168,
-0.699005157221689));
#42230=CARTESIAN_POINT('Ctrl Pts',(0.0361464644047429,-0.0795062346231174,
-0.692656266877045));
#42231=CARTESIAN_POINT('Ctrl Pts',(0.0863977932766005,-0.0127761320376415,
-0.686307376532398));
#42232=CARTESIAN_POINT('Ctrl Pts',(0.0576103404526291,0.065641883777369,
-0.679958486187753));
#42233=CARTESIAN_POINT('Ctrl Pts',(-0.0238804390394198,0.0840091236961439,
-0.673609595843108));
#42234=CARTESIAN_POINT('Ctrl Pts',(-0.0835248178717377,0.0255227943690046,
-0.667260705498462));
#42235=CARTESIAN_POINT('Ctrl Pts',(-0.0667586820880982,-0.0563124018202895,
-0.660911815153819));
#42236=CARTESIAN_POINT('Ctrl Pts',(0.011079903578258,-0.0866316568559436,
-0.654562924809171));
#42237=CARTESIAN_POINT('Ctrl Pts',(0.0787823266538737,-0.0376981861620926,
-0.648214034464528));
#42238=CARTESIAN_POINT('Ctrl Pts',(0.0744127802759426,0.0457224929822708,
-0.641865144119881));
#42239=CARTESIAN_POINT('Ctrl Pts',(0.00196863068701841,0.0873151345765873,
-0.635516253775237));
#42240=CARTESIAN_POINT('Ctrl Pts',(-0.0722764696578212,0.0490297885648256,
-0.62916736343059));
#42241=CARTESIAN_POINT('Ctrl Pts',(-0.0804013151861886,-0.0341091886335733,
-0.622818473085947));
#42242=CARTESIAN_POINT('Ctrl Pts',(-0.0149731015673857,-0.0860442587414302,
-0.6164695827413));
#42243=CARTESIAN_POINT('Ctrl Pts',(0.0641528659084539,-0.0592639690591287,
-0.610120692396656));
#42244=CARTESIAN_POINT('Ctrl Pts',(0.0845902468891876,0.0217324265588487,
-0.60377180205201));
#42245=CARTESIAN_POINT('Ctrl Pts',(0.027642433133917,0.0828474750571577,
-0.597422911707366));
#42246=CARTESIAN_POINT('Ctrl Pts',(-0.0545933440652645,0.0681716584562908,
-0.591074021362719));
#42247=CARTESIAN_POINT('Ctrl Pts',(-0.0868858155389696,-0.0088692328325284,
-0.584725131018075));
#42248=CARTESIAN_POINT('Ctrl Pts',(-0.0396930507999507,-0.0777963363604095,
-0.578376240673428));
#42249=CARTESIAN_POINT('Ctrl Pts',(0.0438118725954223,-0.0755534780972525,
-0.572027350328785));
#42250=CARTESIAN_POINT('Ctrl Pts',(0.0872366399772161,-0.00419247878885715,
-0.565678459984137));
#42251=CARTESIAN_POINT('Ctrl Pts',(0.0508552285025388,0.0710039010679274,
-0.559329569639494));
#42252=CARTESIAN_POINT('Ctrl Pts',(-0.0320497705692809,0.0812442024969535,
-0.552980679294847));
#42253=CARTESIAN_POINT('Ctrl Pts',(-0.0856348677853095,0.017160351170707,
-0.546631788950203));
#42254=CARTESIAN_POINT('Ctrl Pts',(-0.0608791259157248,-0.0626222026173367,
-0.540282898605557));
#42255=CARTESIAN_POINT('Ctrl Pts',(0.0195703062739464,-0.085116457546431,
-0.533934008260913));
#42256=CARTESIAN_POINT('Ctrl Pts',(0.0821163510431211,-0.0297441275594417,
-0.527585117916266));
#42257=CARTESIAN_POINT('Ctrl Pts',(0.0695403805661829,0.052838846539454,
-0.521236227571622));
#42258=CARTESIAN_POINT('Ctrl Pts',(-0.00665280454283421,0.0870835714967197,
-0.514887337226976));
#42259=CARTESIAN_POINT('Ctrl Pts',(-0.0767598438605726,0.0416621483292682,
-0.508538446882331));
#42260=CARTESIAN_POINT('Ctrl Pts',(-0.0766451296842338,-0.0418728113290297,
-0.502189556537686));
#42261=CARTESIAN_POINT('Ctrl Pts',(-0.00641360530457873,-0.0871015149116623,
-0.49584066619304));
#42262=CARTESIAN_POINT('Ctrl Pts',(0.0696852396434252,-0.0526476553015217,
-0.489491775848395));
#42263=CARTESIAN_POINT('Ctrl Pts',(0.0820343493873717,0.0299695471020194,
-0.48314288550375));
#42264=CARTESIAN_POINT('Ctrl Pts',(0.0193364609744337,0.0851698861681384,
-0.476793995159104));
#42265=CARTESIAN_POINT('Ctrl Pts',(-0.0610508875481533,0.0624547625285068,
-0.47044510481446));
#42266=CARTESIAN_POINT('Ctrl Pts',(-0.0855874140733924,-0.0173954817449568,
-0.464096214469814));
#42267=CARTESIAN_POINT('Ctrl Pts',(-0.0318265133113365,-0.0813319204454977,
-0.45774732412517));
#42268=CARTESIAN_POINT('Ctrl Pts',(0.0510500481910435,-0.070863959899244,
-0.451398433780523));
#42269=CARTESIAN_POINT('Ctrl Pts',(0.0872247963540974,0.00443205752395941,
-0.445049543435879));
#42270=CARTESIAN_POINT('Ctrl Pts',(0.0436042004922963,0.0756735220029905,
-0.438700653091233));
#42271=CARTESIAN_POINT('Ctrl Pts',(-0.0399065679425262,0.0776870263812308,
-0.432351762746588));
#42272=CARTESIAN_POINT('Ctrl Pts',(-0.0869098470976033,0.00863056836950265,
-0.426002872401942));
#42273=CARTESIAN_POINT('Ctrl Pts',(-0.054405905391453,-0.0683213414054914,
-0.419653982057298));
#42274=CARTESIAN_POINT('Ctrl Pts',(0.0278698686279614,-0.0827712429263309,
-0.413305091712652));
#42275=CARTESIAN_POINT('Ctrl Pts',(0.0846496157370046,-0.0215000183368973,
-0.406956201368007));
#42276=CARTESIAN_POINT('Ctrl Pts',(0.0639898560584943,0.0594399407345146,
-0.400607311023361));
#42277=CARTESIAN_POINT('Ctrl Pts',(-0.0152093647792003,0.0860028107443161,
-0.394258420678717));
#42278=CARTESIAN_POINT('Ctrl Pts',(-0.0804946924846155,0.0338882385897622,
-0.387909530334071));
#42279=CARTESIAN_POINT('Ctrl Pts',(-0.0721415372417917,-0.0492281102349125,
-0.381560639989426));
#42280=CARTESIAN_POINT('Ctrl Pts',(0.00220843339423072,-0.0873093984336892,
-0.375211749644781));
#42281=CARTESIAN_POINT('Ctrl Pts',(0.0745380759834756,-0.0455179465880336,
-0.368862859300135));
#42282=CARTESIAN_POINT('Ctrl Pts',(0.0786784918314324,0.0379144188408675,
-0.36251396895549));
#42283=CARTESIAN_POINT('Ctrl Pts',(0.0108419288216904,0.0866617609579614,
-0.356165078610845));
#42284=CARTESIAN_POINT('Ctrl Pts',(-0.0669130917411956,0.0561288373881358,
-0.349816188266199));
#42285=CARTESIAN_POINT('Ctrl Pts',(-0.0834544047526216,-0.0257520981726755,
-0.343467297921554));
#42286=CARTESIAN_POINT('Ctrl Pts',(-0.0236496187649619,-0.0840743942302376,
-0.337118407576909));
#42287=CARTESIAN_POINT('Ctrl Pts',(0.0577904079373426,-0.0654834099856214,
-0.330769517232263));
#42288=CARTESIAN_POINT('Ctrl Pts',(0.086362377900638,0.0130133745145877,
-0.324420626887618));
#42289=CARTESIAN_POINT('Ctrl Pts',(0.0359279650068146,0.0796052106546962,
-0.318071736542973));
#42290=CARTESIAN_POINT('Ctrl Pts',(-0.0473742153988214,0.073372283242758,
-0.311722846198328));
#42291=CARTESIAN_POINT('Ctrl Pts',(-0.0873373228152785,1.66243603213149E-5,
-0.305373955853682));
#42292=CARTESIAN_POINT('Ctrl Pts',(-0.0474021442906221,-0.073354242887242,
-0.299025065509037));
#42293=CARTESIAN_POINT('Ctrl Pts',(0.0358976572459432,-0.0796188824159332,
-0.292676175164391));
#42294=CARTESIAN_POINT('Ctrl Pts',(0.0863574175401337,-0.0130462511361909,
-0.286327284819747));
#42295=CARTESIAN_POINT('Ctrl Pts',(0.0578153328344367,0.0654614048287443,
-0.279978394475101));
#42296=CARTESIAN_POINT('Ctrl Pts',(-0.0236176105063063,0.0840833913854678,
-0.273629504130456));
#42297=CARTESIAN_POINT('Ctrl Pts',(-0.083444595058164,0.0257838668257644,
-0.267280613785811));
#42298=CARTESIAN_POINT('Ctrl Pts',(-0.0669344547556335,-0.0561033599660063,
-0.260931723441166));
#42299=CARTESIAN_POINT('Ctrl Pts',(0.0108089364983639,-0.086665882126032,
-0.25458283309652));
#42300=CARTESIAN_POINT('Ctrl Pts',(0.0786640523710499,-0.0379443684553606,
-0.248233942751875));
#42301=CARTESIAN_POINT('Ctrl Pts',(0.0745553989520529,0.045489567155642,
-0.24188505240723));
#42302=CARTESIAN_POINT('Ctrl Pts',(0.00224167132305463,0.087308551371477,
-0.235536162062585));
#42303=CARTESIAN_POINT('Ctrl Pts',(-0.0721227912104874,0.0492555704558522,
-0.229187271717939));
#42304=CARTESIAN_POINT('Ctrl Pts',(-0.0805075876714163,-0.0338575923571341,
-0.222838381373294));
#42305=CARTESIAN_POINT('Ctrl Pts',(-0.015242104357177,-0.0859970144113175,
-0.216489491028649));
#42306=CARTESIAN_POINT('Ctrl Pts',(0.0639672230445058,-0.0594642969265874,
-0.210140600684003));
#42307=CARTESIAN_POINT('Ctrl Pts',(0.0846577945115181,0.0214677912515853,
-0.203791710339358));
#42308=CARTESIAN_POINT('Ctrl Pts',(0.0279013770542819,0.0827606270598339,
-0.197442819994713));
#42309=CARTESIAN_POINT('Ctrl Pts',(-0.0543798919864373,0.0683420484111352,
-0.191093929650068));
#42310=CARTESIAN_POINT('Ctrl Pts',(-0.0869131263917905,-0.00859748176483909,
-0.184745039305422));
#42311=CARTESIAN_POINT('Ctrl Pts',(-0.0399361399802455,-0.0776718285893026,
-0.178396148960777));
#42312=CARTESIAN_POINT('Ctrl Pts',(0.0435753889642203,-0.0756901163504716,
-0.172047258616132));
#42313=CARTESIAN_POINT('Ctrl Pts',(0.0872231027375695,-0.00446526306300281,
-0.165698368271486));
#42314=CARTESIAN_POINT('Ctrl Pts',(0.0510770219946841,0.0708445203210023,
-0.159349477926841));
#42315=CARTESIAN_POINT('Ctrl Pts',(-0.031795548652228,0.0813440307632768,
-0.153000587582196));
#42316=CARTESIAN_POINT('Ctrl Pts',(-0.0855807852442883,0.0174280628811339,
-0.146651697237551));
#42317=CARTESIAN_POINT('Ctrl Pts',(-0.0610746597672231,-0.0624315160748942,
-0.140302806892905));
#42318=CARTESIAN_POINT('Ctrl Pts',(0.019304037012885,-0.0851772417740305,
-0.13395391654826));
#42319=CARTESIAN_POINT('Ctrl Pts',(0.0820229322870143,-0.03000077385872,
-0.127605026203615));
#42320=CARTESIAN_POINT('Ctrl Pts',(0.0697052809023569,0.0526211209250912,
-0.12125613585897));
#42321=CARTESIAN_POINT('Ctrl Pts',(-0.00638045292204925,0.0871039537597873,
-0.114907245514324));
#42322=CARTESIAN_POINT('Ctrl Pts',(-0.0766291701037609,0.0419019798479763,
-0.108558355169679));
#42323=CARTESIAN_POINT('Ctrl Pts',(-0.0767757240810127,-0.0416329106169278,
-0.102209464825034));
#42324=CARTESIAN_POINT('Ctrl Pts',(-0.00668590821907806,-0.0870810566848186,
-0.0958605744803883));
#42325=CARTESIAN_POINT('Ctrl Pts',(0.0695201691859918,-0.0528652704077562,
-0.0895116841357433));
#42326=CARTESIAN_POINT('Ctrl Pts',(0.0821278409720519,0.0297127773219571,
-0.0831627937910981));
#42327=CARTESIAN_POINT('Ctrl Pts',(0.0196023809749374,0.0851091659979851,
-0.0768139034464528));
#42328=CARTESIAN_POINT('Ctrl Pts',(-0.0608546612607467,0.0626450616134637,
-0.0704650131018075));
#42329=CARTESIAN_POINT('Ctrl Pts',(-0.0856425709892414,-0.0171271562291846,
-0.0641161227571622));
#42330=CARTESIAN_POINT('Ctrl Pts',(-0.0320784659707213,-0.081233120284334,
-0.0577672324125169));
#42331=CARTESIAN_POINT('Ctrl Pts',(0.0508239621622661,-0.0710211228679567,
-0.0514183420678718));
#42332=CARTESIAN_POINT('Ctrl Pts',(0.0872462569835861,0.00415522130723803,
-0.0450694517232264));
#42333=CARTESIAN_POINT('Ctrl Pts',(0.0438253963339189,0.0755444771434547,
-0.0387205613785811));
#42334=CARTESIAN_POINT('Ctrl Pts',(-0.0396344344718481,0.0777967966107338,
-0.0323716710339359));
#42335=CARTESIAN_POINT('Ctrl Pts',(-0.0869382878310626,0.00893070154157359,
-0.0260227806892905));
#42336=CARTESIAN_POINT('Ctrl Pts',(-0.0545061222546148,-0.0682098628070873,
-0.0196738903446452));
#42337=CARTESIAN_POINT('Ctrl Pts',(5.63936834513772E-5,-0.0778762677080245,
-0.0154412967815484));
#42338=CARTESIAN_POINT('Ctrl Pts',(0.0233628051714112,-0.0701098376443897,
-0.013325));
#42339=CARTESIAN_POINT('Ctrl Pts',(0.0731896930038075,0.0358351862576369,
-1.1580911015872));
#42340=CARTESIAN_POINT('Ctrl Pts',(0.0612771052025858,0.0601654251960909,
-1.15597480480565));
#42341=CARTESIAN_POINT('Ctrl Pts',(0.0114916655439019,0.0955939602960504,
-1.15174221124255));
#42342=CARTESIAN_POINT('Ctrl Pts',(-0.0742381779154394,0.0614541596632013,
-1.14539332089791));
#42343=CARTESIAN_POINT('Ctrl Pts',(-0.0918142430853653,-0.0289840762275061,
-1.13904443055326));
#42344=CARTESIAN_POINT('Ctrl Pts',(-0.0255165821619241,-0.0928665201499235,
-1.13269554020862));
#42345=CARTESIAN_POINT('Ctrl Pts',(0.0641869236717294,-0.0718136494209175,
-1.12634664986397));
#42346=CARTESIAN_POINT('Ctrl Pts',(0.0951377280764297,0.0149472487601828,
-1.11999775951933));
#42347=CARTESIAN_POINT('Ctrl Pts',(0.0390716166874169,0.0880281547906619,
-1.11364886917468));
#42348=CARTESIAN_POINT('Ctrl Pts',(-0.05274730768283,0.0805818902083492,
-1.10729997883004));
#42349=CARTESIAN_POINT('Ctrl Pts',(-0.0963068964743298,-0.000584265145724099,
-1.10095108848539));
#42350=CARTESIAN_POINT('Ctrl Pts',(-0.051765163313003,-0.0812150573718085,
-1.09460219814075));
#42351=CARTESIAN_POINT('Ctrl Pts',(0.0401339301796505,-0.0875488147178018,
-1.0882533077961));
#42352=CARTESIAN_POINT('Ctrl Pts',(0.0953168300757157,-0.0137905682075853,
-1.08190441745145));
#42353=CARTESIAN_POINT('Ctrl Pts',(0.063301971900001,0.0725834956015103,
-1.07555552710681));
#42354=CARTESIAN_POINT('Ctrl Pts',(-0.0266232512561183,0.0925564966050465,
-1.06920663676216));
#42355=CARTESIAN_POINT('Ctrl Pts',(-0.092192779313374,0.0278565506200653,
-1.06285774641752));
#42356=CARTESIAN_POINT('Ctrl Pts',(-0.0734221876299457,-0.0623272200855746,
-1.05650885607287));
#42357=CARTESIAN_POINT('Ctrl Pts',(0.0125168181131665,-0.0954925588394342,
-1.05015996572822));
#42358=CARTESIAN_POINT('Ctrl Pts',(0.0870051220344295,-0.041299000205068,
-1.04381107538358));
#42359=CARTESIAN_POINT('Ctrl Pts',(0.0818990533106015,0.0506758755513958,
-1.03746218503893));
#42360=CARTESIAN_POINT('Ctrl Pts',(0.00186975430856264,0.0962912415435487,
-1.03111329469429));
#42361=CARTESIAN_POINT('Ctrl Pts',(-0.0798700387269449,0.0538170603806867,
-1.02476440434965));
#42362=CARTESIAN_POINT('Ctrl Pts',(-0.0885427982891663,-0.03789026310174,
-1.018415514005));
#42363=CARTESIAN_POINT('Ctrl Pts',(-0.0162144732994691,-0.0949346617344636,
-1.01206662366035));
#42364=CARTESIAN_POINT('Ctrl Pts',(0.0709472419722389,-0.06513054573261,
-1.00571773331571));
#42365=CARTESIAN_POINT('Ctrl Pts',(0.0932047120936722,0.0242565617509546,
-0.999368842971063));
#42366=CARTESIAN_POINT('Ctrl Pts',(0.030196267188026,0.0914531824923003,
-0.993019952626421));
#42367=CARTESIAN_POINT('Ctrl Pts',(-0.060436450001061,0.0749862297363351,
-0.986671062281772));
#42368=CARTESIAN_POINT('Ctrl Pts',(-0.0957804474814418,-0.0100799315967322,
-0.98032217193713));
#42369=CARTESIAN_POINT('Ctrl Pts',(-0.0435021852574599,-0.0859247287909974,
-0.973973281592482));
#42370=CARTESIAN_POINT('Ctrl Pts',(0.0485729235392217,-0.0831635150695851,
-0.967624391247839));
#42371=CARTESIAN_POINT('Ctrl Pts',(0.0962123522794268,-0.00432231523683321,
-0.961275500903193));
#42372=CARTESIAN_POINT('Ctrl Pts',(0.0558344044174431,0.0784730426539623,
-0.954926610558547));
#42373=CARTESIAN_POINT('Ctrl Pts',(-0.0356222010631393,0.0894793715413515,
-0.948577720213903));
#42374=CARTESIAN_POINT('Ctrl Pts',(-0.0944907592507357,0.0186278167339679,
-0.942228829869257));
#42375=CARTESIAN_POINT('Ctrl Pts',(-0.0669168955953715,-0.0692649133682613,
-0.935879939524612));
#42376=CARTESIAN_POINT('Ctrl Pts',(0.0218741554686966,-0.0937924328641027,
-0.929531049179966));
#42377=CARTESIAN_POINT('Ctrl Pts',(0.0906542023937006,-0.032516376311064,
-0.923182158835321));
#42378=CARTESIAN_POINT('Ctrl Pts',(0.0765016020707636,0.0585064442659452,
-0.916833268490676));
#42379=CARTESIAN_POINT('Ctrl Pts',(-0.00763650593860646,0.096006160828812,
-0.910484378146031));
#42380=CARTESIAN_POINT('Ctrl Pts',(-0.0847885544329253,0.0456771296954345,
-0.904135487801385));
#42381=CARTESIAN_POINT('Ctrl Pts',(-0.0843739916750971,-0.046438439560873,
-0.897786597456739));
#42382=CARTESIAN_POINT('Ctrl Pts',(-0.00677206965841167,-0.0960710060974691,
-0.891437707112095));
#42383=CARTESIAN_POINT('Ctrl Pts',(0.0770251047491154,-0.0578155029246153,
-0.885088816767449));
#42384=CARTESIAN_POINT('Ctrl Pts',(0.0903578586144035,0.0333310144858777,
-0.878739926422805));
#42385=CARTESIAN_POINT('Ctrl Pts',(0.0210290676568723,0.0939855172541015,
-0.872391036078158));
#42386=CARTESIAN_POINT('Ctrl Pts',(-0.0675376207603448,0.068659805724093,
-0.866042145733514));
#42387=CARTESIAN_POINT('Ctrl Pts',(-0.0943192674411041,-0.0194775493687425,
-0.859693255388868));
#42388=CARTESIAN_POINT('Ctrl Pts',(-0.0348153771160591,-0.0897963732914918,
-0.853344365044223));
#42389=CARTESIAN_POINT('Ctrl Pts',(0.0565384585278954,-0.0779673126850463,
-0.846995474699577));
#42390=CARTESIAN_POINT('Ctrl Pts',(0.0961695508987841,0.00518812297122139,
-0.840646584354933));
#42391=CARTESIAN_POINT('Ctrl Pts',(0.0478224224030806,0.0835973388065655,
-0.834297694010287));
#42392=CARTESIAN_POINT('Ctrl Pts',(-0.0442738096418514,0.085529696128511,
-0.827948803665642));
#42393=CARTESIAN_POINT('Ctrl Pts',(-0.0958672945399675,0.00921742792895202,
-0.821599913320997));
#42394=CARTESIAN_POINT('Ctrl Pts',(-0.0597590699666867,-0.0755271652900795,
-0.81525102297635));
#42395=CARTESIAN_POINT('Ctrl Pts',(0.0310181907742342,-0.0911776890534718,
-0.808902132631707));
#42396=CARTESIAN_POINT('Ctrl Pts',(0.0934192636956881,-0.0234166673673649,
-0.80255324228706));
#42397=CARTESIAN_POINT('Ctrl Pts',(0.0703581447091877,0.065766485485537,
-0.796204351942415));
#42398=CARTESIAN_POINT('Ctrl Pts',(-0.0170682992386754,0.0947848737992373,
-0.78985546159777));
#42399=CARTESIAN_POINT('Ctrl Pts',(-0.0888802520487178,0.037091777199195,
-0.783506571253126));
#42400=CARTESIAN_POINT('Ctrl Pts',(-0.0793824101020987,-0.0545337703301412,
-0.777157680908479));
#42401=CARTESIAN_POINT('Ctrl Pts',(0.00273637208614892,-0.0962705116213914,
-0.770808790563835));
#42402=CARTESIAN_POINT('Ctrl Pts',(0.0823518551998093,-0.0499366707459357,
-0.764459900219189));
#42403=CARTESIAN_POINT('Ctrl Pts',(0.086629878194021,0.0420804389726088,
-0.758111009874544));
#42404=CARTESIAN_POINT('Ctrl Pts',(0.011656802621483,0.0956013498475942,
-0.751762119529899));
#42405=CARTESIAN_POINT('Ctrl Pts',(-0.0739801966779158,0.0616638438595523,
-0.745413229185254));
#42406=CARTESIAN_POINT('Ctrl Pts',(-0.0919383306581472,-0.0286852313191213,
-0.739064338840609));
#42407=CARTESIAN_POINT('Ctrl Pts',(-0.0257890659331354,-0.0927923661641124,
-0.732715448495962));
#42408=CARTESIAN_POINT('Ctrl Pts',(0.0639526572925559,-0.0720108100583468,
-0.726366558151318));
#42409=CARTESIAN_POINT('Ctrl Pts',(0.0951889496858655,0.0146479690653711,
-0.720017667806673));
#42410=CARTESIAN_POINT('Ctrl Pts',(0.039344098814443,0.0879064333738871,
-0.713668777462027));
#42411=CARTESIAN_POINT('Ctrl Pts',(-0.0524936810344394,0.0807459756984393,
-0.707319887117383));
#42412=CARTESIAN_POINT('Ctrl Pts',(-0.0963089774570548,-0.000282844860001636,
-0.700970996772735));
#42413=CARTESIAN_POINT('Ctrl Pts',(-0.0520185022402654,-0.0810529121297798,
-0.694622106428093));
#42414=CARTESIAN_POINT('Ctrl Pts',(0.0398597513998638,-0.0876738236783333,
-0.688273216083445));
#42415=CARTESIAN_POINT('Ctrl Pts',(0.095273344660789,-0.0140886101935142,
-0.681924325738802));
#42416=CARTESIAN_POINT('Ctrl Pts',(0.0635285881017423,0.0723852031415087,
-0.675575435394155));
#42417=CARTESIAN_POINT('Ctrl Pts',(-0.0263336505826002,0.0926392896509459,
-0.669226545049511));
#42418=CARTESIAN_POINT('Ctrl Pts',(-0.092105231615666,0.0281447232898606,
-0.662877654704864));
#42419=CARTESIAN_POINT('Ctrl Pts',(-0.0736167289286767,-0.0620973136446348,
-0.656528764360221));
#42420=CARTESIAN_POINT('Ctrl Pts',(0.012218130028394,-0.0955312327914153,
-0.650179874015573));
#42421=CARTESIAN_POINT('Ctrl Pts',(0.0868755494303378,-0.0415708798465372,
-0.64383098367093));
#42422=CARTESIAN_POINT('Ctrl Pts',(0.0820571243029361,0.0504195149834954,
-0.637482093326283));
#42423=CARTESIAN_POINT('Ctrl Pts',(0.00217086597748532,0.0962849234353234,
-0.63113320298164));
#42424=CARTESIAN_POINT('Ctrl Pts',(-0.0797013528173027,0.0540665654460328,
-0.624784312636992));
#42425=CARTESIAN_POINT('Ctrl Pts',(-0.0886608548946474,-0.0376131885033519,
-0.618435422292349));
#42426=CARTESIAN_POINT('Ctrl Pts',(-0.0165112720148233,-0.0948834919071322,
-0.612086531947702));
#42427=CARTESIAN_POINT('Ctrl Pts',(0.0707432200855638,-0.0653520921774031,
-0.605737641603058));
#42428=CARTESIAN_POINT('Ctrl Pts',(0.0932801109978982,0.0239649751149068,
-0.599388751258413));
#42429=CARTESIAN_POINT('Ctrl Pts',(0.0304821102409294,0.091358306110053,
-0.593039860913766));
#42430=CARTESIAN_POINT('Ctrl Pts',(-0.0602016589551456,0.0751748588231912,
-0.586690970569124));
#42431=CARTESIAN_POINT('Ctrl Pts',(-0.0958115009196643,-0.00978035948007525,
-0.580342080224475));
#42432=CARTESIAN_POINT('Ctrl Pts',(-0.0437706747601158,-0.0857882694258514,
-0.573993189879833));
#42433=CARTESIAN_POINT('Ctrl Pts',(0.0483126186412545,-0.0833150047714283,
-0.567644299535184));
#42434=CARTESIAN_POINT('Ctrl Pts',(0.0961983651710867,-0.00462316757738183,
-0.561295409190541));
#42435=CARTESIAN_POINT('Ctrl Pts',(0.0560795308441945,0.0782980546395207,
-0.554946518845895));
#42436=CARTESIAN_POINT('Ctrl Pts',(-0.0353422086600146,0.0895903311025827,
-0.54859762850125));
#42437=CARTESIAN_POINT('Ctrl Pts',(-0.0944320446631196,0.0189232153922341,
-0.542248738156605));
#42438=CARTESIAN_POINT('Ctrl Pts',(-0.0671331723421136,-0.0690553134184647,
-0.53589984781196));
#42439=CARTESIAN_POINT('Ctrl Pts',(0.0215807425634793,-0.0938603787039407,
-0.529550957467314));
#42440=CARTESIAN_POINT('Ctrl Pts',(0.090552074520826,-0.0327997094501317,
-0.52320206712267));
#42441=CARTESIAN_POINT('Ctrl Pts',(0.0766841882675571,0.0582669238057431,
-0.516853176778024));
#42442=CARTESIAN_POINT('Ctrl Pts',(-0.00733623992155941,0.0960295721319826,
-0.510504286433379));
#42443=CARTESIAN_POINT('Ctrl Pts',(-0.0846452991782301,0.0459420555381036,
-0.504155396088733));
#42444=CARTESIAN_POINT('Ctrl Pts',(-0.0845188005392554,-0.0461743597188309,
-0.497806505744088));
#42445=CARTESIAN_POINT('Ctrl Pts',(-0.00707246800557763,-0.0960493588544368,
-0.491457615399443));
#42446=CARTESIAN_POINT('Ctrl Pts',(0.0768439285603362,-0.0580560916997712,
-0.485108725054797));
#42447=CARTESIAN_POINT('Ctrl Pts',(0.0904616489241209,0.0330482860972778,
-0.478759834710152));
#42448=CARTESIAN_POINT('Ctrl Pts',(0.0213228745905474,0.0939192959898768,
-0.472410944365507));
#42449=CARTESIAN_POINT('Ctrl Pts',(-0.0673225788603292,0.0688706723913238,
-0.466062054020862));
#42450=CARTESIAN_POINT('Ctrl Pts',(-0.0943797160829615,-0.0191825006747795,
-0.459713163676217));
#42451=CARTESIAN_POINT('Ctrl Pts',(-0.0350960164266517,-0.0896870602206277,
-0.453364273331571));
#42452=CARTESIAN_POINT('Ctrl Pts',(0.0562943641475219,-0.0781437374667004,
-0.447015382986926));
#42453=CARTESIAN_POINT('Ctrl Pts',(0.0961853048654396,0.00488735797550875,
-0.440666492642281));
#42454=CARTESIAN_POINT('Ctrl Pts',(0.0480836126087228,0.0834473806571098,
-0.434317602297635));
#42455=CARTESIAN_POINT('Ctrl Pts',(-0.0440061262866458,0.0856677301513364,
-0.42796871195299));
#42456=CARTESIAN_POINT('Ctrl Pts',(-0.0958380012141929,0.00951717727620129,
-0.421619821608344));
#42457=CARTESIAN_POINT('Ctrl Pts',(-0.0599949649101275,-0.0753399185390514,
-0.4152709312637));
#42458=CARTESIAN_POINT('Ctrl Pts',(0.030732909936045,-0.091274242735294,
-0.408922040919054));
#42459=CARTESIAN_POINT('Ctrl Pts',(0.0933455787429149,-0.023708691848952,
-0.402573150574409));
#42460=CARTESIAN_POINT('Ctrl Pts',(0.0705634644109166,0.0655461412317127,
-0.396224260229763));
#42461=CARTESIAN_POINT('Ctrl Pts',(-0.0167718062895594,0.0948377860023304,
-0.389875369885119));
#42462=CARTESIAN_POINT('Ctrl Pts',(-0.0887638247414365,0.0373695405017222,
-0.383526479540473));
#42463=CARTESIAN_POINT('Ctrl Pts',(-0.0795525589408519,-0.0542852604857035,
-0.377177589195828));
#42464=CARTESIAN_POINT('Ctrl Pts',(0.00243530335613392,-0.0962785980247009,
-0.370828698851183));
#42465=CARTESIAN_POINT('Ctrl Pts',(0.0821952915023019,-0.0501939557605288,
-0.364479808506538));
#42466=CARTESIAN_POINT('Ctrl Pts',(0.0867610477694602,0.0418093258733485,
-0.358130918161892));
#42467=CARTESIAN_POINT('Ctrl Pts',(0.0119557083837728,0.0955644294551089,
-0.351782027817247));
#42468=CARTESIAN_POINT('Ctrl Pts',(-0.0737870009175868,0.0618948918379082,
-0.345433137472602));
#42469=CARTESIAN_POINT('Ctrl Pts',(-0.0920275850333652,-0.0283975832240196,
-0.339084247127956));
#42470=CARTESIAN_POINT('Ctrl Pts',(-0.0260791183922587,-0.0927112653560552,
-0.332735356783311));
#42471=CARTESIAN_POINT('Ctrl Pts',(0.0637271537234194,-0.0722104495094026,
-0.326386466438666));
#42472=CARTESIAN_POINT('Ctrl Pts',(0.095234291101752,0.0143502243322243,
-0.32003757609402));
#42473=CARTESIAN_POINT('Ctrl Pts',(0.0396188057963046,0.087782967410045,
-0.313688685749375));
#42474=CARTESIAN_POINT('Ctrl Pts',(-0.0522409170483859,0.0809097381406094,
-0.30733979540473));
#42475=CARTESIAN_POINT('Ctrl Pts',(-0.0963093910476554,1.83321627840156E-5,
-0.300990905060085));
#42476=CARTESIAN_POINT('Ctrl Pts',(-0.0522717150448785,-0.0808898445189835,
-0.294642014715439));
#42477=CARTESIAN_POINT('Ctrl Pts',(0.0395853845521076,-0.087798043656451,
-0.288293124370794));
#42478=CARTESIAN_POINT('Ctrl Pts',(0.0952288211688058,-0.0143864783334232,
-0.281944234026149));
#42479=CARTESIAN_POINT('Ctrl Pts',(0.063754639128095,0.0721861837866822,
-0.275595343681504));
#42480=CARTESIAN_POINT('Ctrl Pts',(-0.0260438219599888,0.092721186779261,
-0.269246453336858));
#42481=CARTESIAN_POINT('Ctrl Pts',(-0.0920167675996606,0.0284326154363034,
-0.262897562992213));
#42482=CARTESIAN_POINT('Ctrl Pts',(-0.0738105585312733,-0.061866797147901,
-0.256548672647567));
#42483=CARTESIAN_POINT('Ctrl Pts',(0.0119193267949383,-0.0955689739862951,
-0.250199782302923));
#42484=CARTESIAN_POINT('Ctrl Pts',(0.0867451249590103,-0.041842352179179,
-0.243850891958277));
#42485=CARTESIAN_POINT('Ctrl Pts',(0.0822143940406088,0.0501626609399,-0.237502001613632));
#42486=CARTESIAN_POINT('Ctrl Pts',(0.00247195578125156,0.0962776639447085,
-0.231153111268987));
#42487=CARTESIAN_POINT('Ctrl Pts',(-0.0795318871501312,0.0543155416652873,
-0.224804220924341));
#42488=CARTESIAN_POINT('Ctrl Pts',(-0.0887780446367585,-0.0373357460149329,
-0.218455330579696));
#42489=CARTESIAN_POINT('Ctrl Pts',(-0.0168079091687892,-0.0948313942183441,
-0.212106440235051));
#42490=CARTESIAN_POINT('Ctrl Pts',(0.0705385063320063,-0.0655729995089186,
-0.205757549890406));
#42491=CARTESIAN_POINT('Ctrl Pts',(0.0933545977140429,0.0236731541102014,
-0.19940865954576));
#42492=CARTESIAN_POINT('Ctrl Pts',(0.0307676551887473,0.0912625363123725,
-0.193059769201115));
#42493=CARTESIAN_POINT('Ctrl Pts',(-0.0599662791762946,0.0753627527528736,
-0.18671087885647));
#42494=CARTESIAN_POINT('Ctrl Pts',(-0.0958416173867071,-0.00948069172061055,
-0.180361988511825));
#42495=CARTESIAN_POINT('Ctrl Pts',(-0.044038736227651,-0.0856509711067653,
-0.174013098167179));
#42496=CARTESIAN_POINT('Ctrl Pts',(0.0480518413036898,-0.0834656797238674,
-0.167664207822534));
#42497=CARTESIAN_POINT('Ctrl Pts',(0.0961834372655269,-0.00492397468347903,
-0.161315317477889));
#42498=CARTESIAN_POINT('Ctrl Pts',(0.0563241089406863,0.0781223008817196,
-0.154966427133243));
#42499=CARTESIAN_POINT('Ctrl Pts',(-0.0350618708017759,0.0897004146181866,
-0.148617536788598));
#42500=CARTESIAN_POINT('Ctrl Pts',(-0.0943724062814499,0.0192184288356559,
-0.142268646443953));
#42501=CARTESIAN_POINT('Ctrl Pts',(-0.0673487931736204,-0.0688450378548037,
-0.135919756099307));
#42502=CARTESIAN_POINT('Ctrl Pts',(0.0212871197506783,-0.0939274072291657,
-0.129570865754662));
#42503=CARTESIAN_POINT('Ctrl Pts',(0.0904490589574556,-0.0330827207447464,
-0.123221975410017));
#42504=CARTESIAN_POINT('Ctrl Pts',(0.0768660286360105,0.0580268314756966,
-0.116873085065372));
#42505=CARTESIAN_POINT('Ctrl Pts',(-0.00703590991483225,0.0960520482427784,
-0.110524194720726));
#42506=CARTESIAN_POINT('Ctrl Pts',(-0.0845012014484307,0.0462065246880186,
-0.104175304376081));
#42507=CARTESIAN_POINT('Ctrl Pts',(-0.0846628107564522,-0.04590981426736,
-0.0978264140314358));
#42508=CARTESIAN_POINT('Ctrl Pts',(-0.00737274430247539,-0.0960267989761889,
-0.0914775236867905));
#42509=CARTESIAN_POINT('Ctrl Pts',(0.0766619005942514,-0.0582960621693097,
-0.0851286333421456));
#42510=CARTESIAN_POINT('Ctrl Pts',(0.0905647447976647,0.0327651386368324,
-0.0787797429975001));
#42511=CARTESIAN_POINT('Ctrl Pts',(0.0216161122636334,0.0938523381026498,
-0.072430852652855));
#42512=CARTESIAN_POINT('Ctrl Pts',(-0.0671061944597261,0.0690805206944129,
-0.0660819623082095));
#42513=CARTESIAN_POINT('Ctrl Pts',(-0.094440539208817,-0.0188866103704566,
-0.0597330719635644));
#42514=CARTESIAN_POINT('Ctrl Pts',(-0.0353738519088489,-0.0895781104263087,
-0.0533841816189191));
#42515=CARTESIAN_POINT('Ctrl Pts',(0.0560450525467761,-0.0783170456163444,
-0.0470352912742739));
#42516=CARTESIAN_POINT('Ctrl Pts',(0.0962089701220667,0.00458208267517972,
-0.0406864009296285));
#42517=CARTESIAN_POINT('Ctrl Pts',(0.0483275316587034,0.0833050791594327,
-0.0343375105849833));
#42518=CARTESIAN_POINT('Ctrl Pts',(-0.0437060368403489,0.08578877695719,
-0.027988620240338));
#42519=CARTESIAN_POINT('Ctrl Pts',(-0.095869363633284,0.00984814280277796,
-0.0216397298956927));
#42520=CARTESIAN_POINT('Ctrl Pts',(-0.0601054769427006,-0.0752169878654165,
-0.0152908395510473));
#42521=CARTESIAN_POINT('Ctrl Pts',(6.21869452505711E-5,-0.0858764120339165,
-0.0110582459879505));
#42522=CARTESIAN_POINT('Ctrl Pts',(0.0257628407500271,-0.0773121450523775,
-0.00894194920640216));
#42523=CARTESIAN_POINT('Ctrl Pts',(0.0800079576859287,0.0391735495545708,
-1.1537080507936));
#42524=CARTESIAN_POINT('Ctrl Pts',(0.0669856073847669,0.0657703645921076,
-1.15159175401205));
#42525=CARTESIAN_POINT('Ctrl Pts',(0.0125622154273748,0.104499379851189,
-1.14735916044895));
#42526=CARTESIAN_POINT('Ctrl Pts',(-0.0811541182039119,0.0671791560281841,
-1.14101027010431));
#42527=CARTESIAN_POINT('Ctrl Pts',(-0.100367548684175,-0.0316841982689489,
-1.13466137975966));
#42528=CARTESIAN_POINT('Ctrl Pts',(-0.0278936765835931,-0.101517854627537,
-1.12831248941502));
#42529=CARTESIAN_POINT('Ctrl Pts',(0.0701665010789239,-0.078503723520769,
-1.12196359907037));
#42530=CARTESIAN_POINT('Ctrl Pts',(0.104000645581044,0.0163397166628863,
-1.11561470872573));
#42531=CARTESIAN_POINT('Ctrl Pts',(0.0427114819908452,0.0962287529105411,
-1.10926581838108));
#42532=CARTESIAN_POINT('Ctrl Pts',(-0.0576611840811396,0.0880888031830703,
-1.10291692803644));
#42533=CARTESIAN_POINT('Ctrl Pts',(-0.105278732315225,-0.000638694591246696,
-1.09656803769179));
#42534=CARTESIAN_POINT('Ctrl Pts',(-0.0565875443108695,-0.0887809554458167,
-1.09021914734715));
#42535=CARTESIAN_POINT('Ctrl Pts',(0.0438727593435398,-0.0957047580870532,
-1.0838702570025));
#42536=CARTESIAN_POINT('Ctrl Pts',(0.104196432509398,-0.0150752811268102,
-1.07752136665786));
#42537=CARTESIAN_POINT('Ctrl Pts',(0.0691991082535025,0.0793452876551954,
-1.07117247631321));
#42538=CARTESIAN_POINT('Ctrl Pts',(-0.0291034416533303,0.101178949658241,
-1.06482358596857));
#42539=CARTESIAN_POINT('Ctrl Pts',(-0.100781348896612,0.0304516337180169,
-1.05847469562392));
#42540=CARTESIAN_POINT('Ctrl Pts',(-0.080262111234698,-0.068133549720299,
-1.05212580527927));
#42541=CARTESIAN_POINT('Ctrl Pts',(0.0136828699897497,-0.104388531955573,
-1.04577691493463));
#42542=CARTESIAN_POINT('Ctrl Pts',(0.0951104156404598,-0.0451463659057333,
-1.03942802458998));
#42543=CARTESIAN_POINT('Ctrl Pts',(0.0895286716321017,0.0553967797979785,
-1.03307913424534));
#42544=CARTESIAN_POINT('Ctrl Pts',(0.00204393839436774,0.105261618989727,
-1.02673024390069));
#42545=CARTESIAN_POINT('Ctrl Pts',(-0.087310636464981,0.0588305936669936,
-1.02038135355605));
#42546=CARTESIAN_POINT('Ctrl Pts',(-0.0967913399847819,-0.041420074911301,
-1.0140324632114));
#42547=CARTESIAN_POINT('Ctrl Pts',(-0.0177249943318654,-0.103778661820372,
-1.00768357286676));
#42548=CARTESIAN_POINT('Ctrl Pts',(0.0775566025854628,-0.0711980298477954,
-1.00133468252211));
#42549=CARTESIAN_POINT('Ctrl Pts',(0.101887552130213,0.0265162741709498,
-0.994985792177467));
#42550=CARTESIAN_POINT('Ctrl Pts',(0.0330093154964704,0.0999728521160336,
-0.988636901832822));
#42551=CARTESIAN_POINT('Ctrl Pts',(-0.0660666377453062,0.0819718576420304,
-0.982288011488176));
#42552=CARTESIAN_POINT('Ctrl Pts',(-0.104703239960795,-0.0110189660260845,
-0.97593912114353));
#42553=CARTESIAN_POINT('Ctrl Pts',(-0.0475547970551419,-0.0939293742484679,
-0.969590230798886));
#42554=CARTESIAN_POINT('Ctrl Pts',(0.0530979192795061,-0.0909109291434562,
-0.96324134045424));
#42555=CARTESIAN_POINT('Ctrl Pts',(0.105175380495662,-0.0047249769794186,
-0.956892450109596));
#42556=CARTESIAN_POINT('Ctrl Pts',(0.061035871072958,0.0857834979006917,
-0.950543559764949));
#42557=CARTESIAN_POINT('Ctrl Pts',(-0.0389407229128716,0.0978151632863322,
-0.944194669420305));
#42558=CARTESIAN_POINT('Ctrl Pts',(-0.10329340590964,0.0203631619681055,
-0.937845779075658));
#42559=CARTESIAN_POINT('Ctrl Pts',(-0.0731507939374694,-0.0757175502512242,
-0.931496888731016));
#42560=CARTESIAN_POINT('Ctrl Pts',(0.0239119257552284,-0.102530024268049,
-0.925147998386367));
#42561=CARTESIAN_POINT('Ctrl Pts',(0.0990994399824792,-0.0355455632237716,
-0.918799108041724));
#42562=CARTESIAN_POINT('Ctrl Pts',(0.0836284002593778,0.0639568349732043,
-0.912450217697077));
#42563=CARTESIAN_POINT('Ctrl Pts',(-0.00834791374207134,0.104949980494938,
-0.906101327352435));
#42564=CARTESIAN_POINT('Ctrl Pts',(-0.0926873552395928,0.0499323567281097,
-0.899752437007785));
#42565=CARTESIAN_POINT('Ctrl Pts',(-0.0922341723087004,-0.0507645893144231,
-0.893403546663144));
#42566=CARTESIAN_POINT('Ctrl Pts',(-0.00740294760695452,-0.105020866671638,
-0.887054656318496));
#42567=CARTESIAN_POINT('Ctrl Pts',(0.0842006718241181,-0.0632015263589454,
-0.880705765973852));
#42568=CARTESIAN_POINT('Ctrl Pts',(0.0987754891694415,0.0364360921212848,
-0.874356875629206));
#42569=CARTESIAN_POINT('Ctrl Pts',(0.022988110568765,0.102741096169992,
-0.868007985284561));
#42570=CARTESIAN_POINT('Ctrl Pts',(-0.0738293451199607,0.0750560714991865,
-0.861659094939917));
#42571=CARTESIAN_POINT('Ctrl Pts',(-0.10310593812715,-0.0212920546836966,
-0.85531020459527));
#42572=CARTESIAN_POINT('Ctrl Pts',(-0.0380587362072462,-0.0981616965421876,
-0.848961314250626));
#42573=CARTESIAN_POINT('Ctrl Pts',(0.0618055140263025,-0.0852306547298433,
-0.842612423905979));
#42574=CARTESIAN_POINT('Ctrl Pts',(0.105128591789345,0.00567144233176898,
-0.836263533561335));
#42575=CARTESIAN_POINT('Ctrl Pts',(0.0522775023508458,0.0913851673833921,
-0.829914643216689));
#42576=CARTESIAN_POINT('Ctrl Pts',(-0.048398305048717,0.0934975408133528,
-0.823565752872045));
#42577=CARTESIAN_POINT('Ctrl Pts',(-0.104798177587918,0.0100761125432544,
-0.817216862527398));
#42578=CARTESIAN_POINT('Ctrl Pts',(-0.0653261537932172,-0.0825631861080844,
-0.810867972182754));
#42579=CARTESIAN_POINT('Ctrl Pts',(0.033907808505632,-0.0996716940363645,
-0.804519081838107));
#42580=CARTESIAN_POINT('Ctrl Pts',(0.102122091104091,-0.0255981362263135,
-0.798170191493465));
#42581=CARTESIAN_POINT('Ctrl Pts',(0.07691262572259,0.0718932129911442,
-0.791821301148816));
#42582=CARTESIAN_POINT('Ctrl Pts',(-0.0186583616792568,0.103614919819393,
-0.785472410804175));
#42583=CARTESIAN_POINT('Ctrl Pts',(-0.0971602305349011,0.0405472030125148,
-0.779123520459527));
#42584=CARTESIAN_POINT('Ctrl Pts',(-0.0867775809378697,-0.0596140714622373,
-0.772774630114882));
#42585=CARTESIAN_POINT('Ctrl Pts',(0.00299128925257632,-0.105238957892696,
-0.766425739770237));
#42586=CARTESIAN_POINT('Ctrl Pts',(0.090023656006337,-0.0545887115527192,
-0.760076849425591));
#42587=CARTESIAN_POINT('Ctrl Pts',(0.0947002145305326,0.0460006025787094,
-0.753727959080947));
#42588=CARTESIAN_POINT('Ctrl Pts',(0.0127427364785399,0.104507457804559,
-0.7473790687363));
#42589=CARTESIAN_POINT('Ctrl Pts',(-0.0808721037413772,0.0674083741546789,
-0.741030178391657));
#42590=CARTESIAN_POINT('Ctrl Pts',(-0.100503196107536,-0.0313575133246159,
-0.73468128804701));
#42591=CARTESIAN_POINT('Ctrl Pts',(-0.0281915446185915,-0.101436792544674,
-0.728332397702365));
#42592=CARTESIAN_POINT('Ctrl Pts',(0.0699104107227152,-0.0787192514084998,
-0.721983507357721));
#42593=CARTESIAN_POINT('Ctrl Pts',(0.104056638934646,0.0160125564279404,
-0.715634617013074));
#42594=CARTESIAN_POINT('Ctrl Pts',(0.043009348228488,0.0960956920714652,
-0.70928572666843));
#42595=CARTESIAN_POINT('Ctrl Pts',(-0.0573839298760781,0.0882681746821054,
-0.702936836323783));
#42596=CARTESIAN_POINT('Ctrl Pts',(-0.105281007159824,-0.000309194350488767,
-0.696587945979139));
#42597=CARTESIAN_POINT('Ctrl Pts',(-0.0568644839910446,-0.0886037049460429,
-0.690239055634493));
#42598=CARTESIAN_POINT('Ctrl Pts',(0.0435730383949847,-0.0958414127335492,
-0.683890165289848));
#42599=CARTESIAN_POINT('Ctrl Pts',(0.104148896044978,-0.015401088349387,
-0.677541274945203));
#42600=CARTESIAN_POINT('Ctrl Pts',(0.0694468357508554,0.0791285225056486,
-0.671192384600558));
#42601=CARTESIAN_POINT('Ctrl Pts',(-0.0287868621257805,0.101269455605748,
-0.664843494255913));
#42602=CARTESIAN_POINT('Ctrl Pts',(-0.100685645359594,0.0307666522107167,
-0.658494603911267));
#42603=CARTESIAN_POINT('Ctrl Pts',(-0.0804747757692551,-0.06788222546898,
-0.652145713566622));
#42604=CARTESIAN_POINT('Ctrl Pts',(0.01335635647853,-0.104430808726887,
-0.645796823221977));
#42605=CARTESIAN_POINT('Ctrl Pts',(0.094968772206802,-0.0454435735309818,
-0.639447932877331));
#42606=CARTESIAN_POINT('Ctrl Pts',(0.0897014683299295,0.0551165369847199,
-0.633099042532686));
#42607=CARTESIAN_POINT('Ctrl Pts',(0.00237310126795229,0.10525471229406,
-0.626750152188041));
#42608=CARTESIAN_POINT('Ctrl Pts',(-0.0871262359767842,0.05910334232724,
-0.620401261843395));
#42609=CARTESIAN_POINT('Ctrl Pts',(-0.0969203946031063,-0.0411171883731305,
-0.61405237149875));
#42610=CARTESIAN_POINT('Ctrl Pts',(-0.0180494424622608,-0.103722725072834,
-0.607703481154104));
#42611=CARTESIAN_POINT('Ctrl Pts',(0.0773335742626736,-0.0714402152956775,
-0.601354590809461));
#42612=CARTESIAN_POINT('Ctrl Pts',(0.101969975106609,0.0261975236709649,
-0.595005700464813));
#42613=CARTESIAN_POINT('Ctrl Pts',(0.033321787347942,0.0998691371629481,
-0.58865681012017));
#42614=CARTESIAN_POINT('Ctrl Pts',(-0.0658099738450268,0.0821780591900918,
-0.582307919775524));
#42615=CARTESIAN_POINT('Ctrl Pts',(-0.104737186300359,-0.0106914861276222,
-0.575959029430879));
#42616=CARTESIAN_POINT('Ctrl Pts',(-0.047848298720281,-0.0937802024912932,
-0.569610139086233));
#42617=CARTESIAN_POINT('Ctrl Pts',(0.0528133646870868,-0.0910765314456041,
-0.563261248741589));
#42618=CARTESIAN_POINT('Ctrl Pts',(0.105160090364957,-0.00505385636590638,
-0.556912358396943));
#42619=CARTESIAN_POINT('Ctrl Pts',(0.0613038331858501,0.0855922082111139,
-0.550563468052297));
#42620=CARTESIAN_POINT('Ctrl Pts',(-0.0386346467507483,0.0979364597082119,
-0.544214577707653));
#42621=CARTESIAN_POINT('Ctrl Pts',(-0.10322922154093,0.0206860796137611,
-0.537865687363007));
#42622=CARTESIAN_POINT('Ctrl Pts',(-0.0733872187685025,-0.0754884242195927,
-0.531516797018362));
#42623=CARTESIAN_POINT('Ctrl Pts',(0.0235911788530122,-0.10260429986145,
-0.525167906673717));
#42624=CARTESIAN_POINT('Ctrl Pts',(0.098987797998531,-0.0358552913408218,
-0.518819016329071));
#42625=CARTESIAN_POINT('Ctrl Pts',(0.083827995968931,0.0636950010720324,
-0.512470125984427));
#42626=CARTESIAN_POINT('Ctrl Pts',(-0.00801967530028448,0.104975572767245,
-0.50612123563978));
#42627=CARTESIAN_POINT('Ctrl Pts',(-0.0925307544958878,0.050221962746939,
-0.499772345295136));
#42628=CARTESIAN_POINT('Ctrl Pts',(-0.0923924713942769,-0.050475908108632,
-0.49342345495049));
#42629=CARTESIAN_POINT('Ctrl Pts',(-0.0077313307065766,-0.104997202797211,
-0.487074564605845));
#42630=CARTESIAN_POINT('Ctrl Pts',(0.0840026174772474,-0.0634645280980206,
-0.480725674261199));
#42631=CARTESIAN_POINT('Ctrl Pts',(0.0988889484608699,0.0361270250925362,
-0.474376783916555));
#42632=CARTESIAN_POINT('Ctrl Pts',(0.0233092882066613,0.102668705811615,
-0.468027893571909));
#42633=CARTESIAN_POINT('Ctrl Pts',(-0.0735942701725054,0.0752865822541408,
-0.461679003227264));
#42634=CARTESIAN_POINT('Ctrl Pts',(-0.10317201809253,-0.0209695196046023,
-0.455330112882619));
#42635=CARTESIAN_POINT('Ctrl Pts',(-0.0383655195419671,-0.0980421999957576,
-0.448981222537972));
#42636=CARTESIAN_POINT('Ctrl Pts',(0.0615386801040004,-0.085423515034157,
-0.442632332193329));
#42637=CARTESIAN_POINT('Ctrl Pts',(0.105145813376782,0.00534265842705816,
-0.436283441848682));
#42638=CARTESIAN_POINT('Ctrl Pts',(0.0525630247251494,0.0912212393112291,
-0.429934551504037));
#42639=CARTESIAN_POINT('Ctrl Pts',(-0.0481056846307652,0.0936484339214419,
-0.423585661159393));
#42640=CARTESIAN_POINT('Ctrl Pts',(-0.104766155330783,0.0104037861829001,
-0.417236770814747));
#42641=CARTESIAN_POINT('Ctrl Pts',(-0.0655840244288016,-0.0823584956726115,
-0.410887880470102));
#42642=CARTESIAN_POINT('Ctrl Pts',(0.0335959512441284,-0.0997772425442569,
-0.404538990125456));
#42643=CARTESIAN_POINT('Ctrl Pts',(0.102041541748826,-0.0259173653610067,
-0.398190099780811));
#42644=CARTESIAN_POINT('Ctrl Pts',(0.0771370727633386,0.0716523417289106,
-0.391841209436165));
#42645=CARTESIAN_POINT('Ctrl Pts',(-0.0183342477999184,0.103672761260345,
-0.385492319091521));
#42646=CARTESIAN_POINT('Ctrl Pts',(-0.0970329569982577,0.0408508424136822,
-0.379143428746875));
#42647=CARTESIAN_POINT('Ctrl Pts',(-0.0869635806399119,-0.0593424107364946,
-0.37279453840223));
#42648=CARTESIAN_POINT('Ctrl Pts',(0.00266217331803697,-0.105247797615712,
-0.366445648057585));
#42649=CARTESIAN_POINT('Ctrl Pts',(0.0898525070211284,-0.054869964933024,
-0.36009675771294));
#42650=CARTESIAN_POINT('Ctrl Pts',(0.0948436037074879,0.0457042329058294,
-0.353747867368294));
#42651=CARTESIAN_POINT('Ctrl Pts',(0.0130694879458553,0.104467097952257,
-0.347398977023649));
#42652=CARTESIAN_POINT('Ctrl Pts',(-0.080660910093978,0.0676609462876806,
-0.341050086679004));
#42653=CARTESIAN_POINT('Ctrl Pts',(-0.100600765314109,-0.0310430682753637,
-0.334701196334358));
#42654=CARTESIAN_POINT('Ctrl Pts',(-0.0285086180195555,-0.101348136481873,
-0.328352305989713));
#42655=CARTESIAN_POINT('Ctrl Pts',(0.0696638995094961,-0.078937489033184,
-0.322003415645068));
#42656=CARTESIAN_POINT('Ctrl Pts',(0.104106204302866,0.015687074149861,
-0.315654525300422));
#42657=CARTESIAN_POINT('Ctrl Pts',(0.0433096465857946,0.0959607241653938,
-0.309305634955778));
#42658=CARTESIAN_POINT('Ctrl Pts',(-0.0571076186979503,0.0884471930384607,
-0.302956744611132));
#42659=CARTESIAN_POINT('Ctrl Pts',(-0.105281459280032,2.00399652468685E-5,
-0.296607854266487));
#42660=CARTESIAN_POINT('Ctrl Pts',(-0.0571412857991351,-0.0884254461507251,
-0.290258963921841));
#42661=CARTESIAN_POINT('Ctrl Pts',(0.043273111858272,-0.0959772048969685,
-0.283910073577196));
#42662=CARTESIAN_POINT('Ctrl Pts',(0.104100224797478,-0.0157267055306558,
-0.277561183232551));
#42663=CARTESIAN_POINT('Ctrl Pts',(0.0696939454217535,0.0789109627446204,
-0.271212292887905));
#42664=CARTESIAN_POINT('Ctrl Pts',(-0.0284700334136715,0.101358982173054,
-0.264863402543261));
#42665=CARTESIAN_POINT('Ctrl Pts',(-0.100588940141157,0.0310813640468423,
-0.258514512198615));
#42666=CARTESIAN_POINT('Ctrl Pts',(-0.0806866623069133,-0.0676302343297956,
-0.25216562185397));
#42667=CARTESIAN_POINT('Ctrl Pts',(0.0130297170915128,-0.104472065846558,
-0.245816731509324));
#42668=CARTESIAN_POINT('Ctrl Pts',(0.0948261975469705,-0.0457403359029975,
-0.239467841164679));
#42669=CARTESIAN_POINT('Ctrl Pts',(0.0898733891291647,0.0548357547241582,
-0.233118950820034));
#42670=CARTESIAN_POINT('Ctrl Pts',(0.00270224023944843,0.10524677651794,
-0.226770060475389));
#42671=CARTESIAN_POINT('Ctrl Pts',(-0.086940983089775,0.0593755128747225,
-0.220421170130743));
#42672=CARTESIAN_POINT('Ctrl Pts',(-0.0970485016021008,-0.0408138996727319,
-0.214072279786098));
#42673=CARTESIAN_POINT('Ctrl Pts',(-0.0183737139804013,-0.103665774025371,
-0.207723389441453));
#42674=CARTESIAN_POINT('Ctrl Pts',(0.0771097896195066,-0.0716817020912496,
-0.201374499096807));
#42675=CARTESIAN_POINT('Ctrl Pts',(0.102051400916568,0.0258785169688173,
-0.195025608752163));
#42676=CARTESIAN_POINT('Ctrl Pts',(0.0336339333232127,0.0997644455649112,
-0.188676718407517));
#42677=CARTESIAN_POINT('Ctrl Pts',(-0.0655526663661519,0.082383457094612,
-0.182327828062872));
#42678=CARTESIAN_POINT('Ctrl Pts',(-0.104770108381624,-0.010363901676382,
-0.175978937718226));
#42679=CARTESIAN_POINT('Ctrl Pts',(-0.0481413324750565,-0.0936301136242282,
-0.169630047373582));
#42680=CARTESIAN_POINT('Ctrl Pts',(0.0525282936431593,-0.0912412430972631,
-0.163281157028936));
#42681=CARTESIAN_POINT('Ctrl Pts',(0.105143771793484,-0.00538268630395523,
-0.156932266684291));
#42682=CARTESIAN_POINT('Ctrl Pts',(0.0615711958866884,0.0854000814424367,
-0.150583376339645));
#42683=CARTESIAN_POINT('Ctrl Pts',(-0.0383281929513239,0.0980567984730965,
-0.144234485995));
#42684=CARTESIAN_POINT('Ctrl Pts',(-0.103164027318611,0.0210087947901778,
-0.137885595650355));
#42685=CARTESIAN_POINT('Ctrl Pts',(-0.0736229265800177,-0.0752585596347131,
-0.13153670530571));
#42686=CARTESIAN_POINT('Ctrl Pts',(0.0232702024884716,-0.102677572684301,
-0.125187814961064));
#42687=CARTESIAN_POINT('Ctrl Pts',(0.0988751856278969,-0.0361646676307727,
-0.118838924616419));
#42688=CARTESIAN_POINT('Ctrl Pts',(0.084026776369664,0.0634325420263019,
-0.112490034271774));
#42689=CARTESIAN_POINT('Ctrl Pts',(-0.00769136690761526,0.10500014272577,
-0.106141143927129));
#42690=CARTESIAN_POINT('Ctrl Pts',(-0.0923732327931005,0.050511069528061,
-0.0997922535824832));
#42691=CARTESIAN_POINT('Ctrl Pts',(-0.0925498974318917,-0.0501867179177923,
-0.093443363237838));
#42692=CARTESIAN_POINT('Ctrl Pts',(-0.00805958038587264,-0.104972541267559,
-0.0870944728931927));
#42693=CARTESIAN_POINT('Ctrl Pts',(0.0838036320025109,-0.0637268539308632,
-0.0807455825485475));
#42694=CARTESIAN_POINT('Ctrl Pts',(0.0990016486232777,0.0358174999517078,
-0.0743966922039025));
#42695=CARTESIAN_POINT('Ctrl Pts',(0.0236298435523293,0.102595510207315,
-0.0680478018592568));
#42696=CARTESIAN_POINT('Ctrl Pts',(-0.0733577276587055,0.0755159797753619,
-0.0616989115146119));
#42697=CARTESIAN_POINT('Ctrl Pts',(-0.103238507428393,-0.0206460645117284,
-0.0553500211699664));
#42698=CARTESIAN_POINT('Ctrl Pts',(-0.0386692378469765,-0.0979231005682837,
-0.0490011308253213));
#42699=CARTESIAN_POINT('Ctrl Pts',(0.061266142931286,-0.0856129683647319,
-0.0426522404806759));
#42700=CARTESIAN_POINT('Ctrl Pts',(0.105171683260548,0.00500894404312121,
-0.0363033501360307));
#42701=CARTESIAN_POINT('Ctrl Pts',(0.0528296669834879,0.0910656811754109,
-0.0299544597913853));
#42702=CARTESIAN_POINT('Ctrl Pts',(-0.0477776392088496,0.0937807573036459,
-0.0236055694467402));
#42703=CARTESIAN_POINT('Ctrl Pts',(-0.104800439435505,0.0107655840639825,
-0.0172566791020948));
#42704=CARTESIAN_POINT('Ctrl Pts',(-0.0657048316307863,-0.0822241129237459,
-0.0109077887574495));
#42705=CARTESIAN_POINT('Ctrl Pts',(6.79802070497962E-5,-0.0938765563598085,
-0.00667519519435267));
#42706=CARTESIAN_POINT('Ctrl Pts',(0.028162876328643,-0.0845144524603652,
-0.00455889841280429));
#42707=CARTESIAN_POINT('Ctrl Pts',(0.08682622236805,0.0425119128515047,
-1.149325));
#42708=CARTESIAN_POINT('Ctrl Pts',(0.0726941095669478,0.0713753039881243,
-1.14720870321845));
#42709=CARTESIAN_POINT('Ctrl Pts',(0.0136327653108478,0.113404799406328,
-1.14297610965536));
#42710=CARTESIAN_POINT('Ctrl Pts',(-0.0880700584923845,0.0729041523931668,
-1.13662721931071));
#42711=CARTESIAN_POINT('Ctrl Pts',(-0.108920854282986,-0.0343843203103918,
-1.13027832896607));
#42712=CARTESIAN_POINT('Ctrl Pts',(-0.030270771005262,-0.110169189105151,
-1.12392943862142));
#42713=CARTESIAN_POINT('Ctrl Pts',(0.0761460784861183,-0.0851937976206204,
-1.11758054827678));
#42714=CARTESIAN_POINT('Ctrl Pts',(0.112863563085659,0.01773218456559,-1.11123165793213));
#42715=CARTESIAN_POINT('Ctrl Pts',(0.0463513472942736,0.10442935103042,
-1.10488276758748));
#42716=CARTESIAN_POINT('Ctrl Pts',(-0.0625750604794491,0.0955957161577918,
-1.09853387724284));
#42717=CARTESIAN_POINT('Ctrl Pts',(-0.11425056815612,-0.000693124036769614,
-1.09218498689819));
#42718=CARTESIAN_POINT('Ctrl Pts',(-0.0614099253087358,-0.0963468535198246,
-1.08583609655355));
#42719=CARTESIAN_POINT('Ctrl Pts',(0.0476115885074291,-0.103860701456305,
-1.0794872062089));
#42720=CARTESIAN_POINT('Ctrl Pts',(0.11307603494308,-0.0163599940460347,
-1.07313831586426));
#42721=CARTESIAN_POINT('Ctrl Pts',(0.075096244607004,0.0861070797088801,
-1.06678942551961));
#42722=CARTESIAN_POINT('Ctrl Pts',(-0.0315836320505423,0.109801402711436,
-1.06044053517497));
#42723=CARTESIAN_POINT('Ctrl Pts',(-0.109369918479851,0.0330467168159683,
-1.05409164483032));
#42724=CARTESIAN_POINT('Ctrl Pts',(-0.0871020348394502,-0.0739398793550231,
-1.04774275448568));
#42725=CARTESIAN_POINT('Ctrl Pts',(0.0148489218663328,-0.113284505071712,
-1.04139386414103));
#42726=CARTESIAN_POINT('Ctrl Pts',(0.10321570924649,-0.0489937316063985,
-1.03504497379639));
#42727=CARTESIAN_POINT('Ctrl Pts',(0.0971582899536019,0.0601176840445611,
-1.02869608345174));
#42728=CARTESIAN_POINT('Ctrl Pts',(0.00221812248017289,0.114231996435905,
-1.02234719310709));
#42729=CARTESIAN_POINT('Ctrl Pts',(-0.0947512342030169,0.0638441269533003,
-1.01599830276245));
#42730=CARTESIAN_POINT('Ctrl Pts',(-0.105039881680398,-0.0449498867208618,
-1.0096494124178));
#42731=CARTESIAN_POINT('Ctrl Pts',(-0.0192355153642617,-0.112622661906281,
-1.00330052207316));
#42732=CARTESIAN_POINT('Ctrl Pts',(0.0841659631986869,-0.0772655139629808,
-0.996951631728514));
#42733=CARTESIAN_POINT('Ctrl Pts',(0.110570392166754,0.0287759865909447,
-0.990602741383869));
#42734=CARTESIAN_POINT('Ctrl Pts',(0.0358223638049151,0.108492521739767,
-0.984253851039224));
#42735=CARTESIAN_POINT('Ctrl Pts',(-0.0716968254895517,0.0889574855477255,
-0.977904960694578));
#42736=CARTESIAN_POINT('Ctrl Pts',(-0.113626032440148,-0.0119580004554367,
-0.971556070349933));
#42737=CARTESIAN_POINT('Ctrl Pts',(-0.0516074088528242,-0.101934019705939,
-0.965207180005287));
#42738=CARTESIAN_POINT('Ctrl Pts',(0.0576229150197905,-0.0986583432173273,
-0.958858289660643));
#42739=CARTESIAN_POINT('Ctrl Pts',(0.114138408711896,-0.00512763872200404,
-0.952509399315997));
#42740=CARTESIAN_POINT('Ctrl Pts',(0.0662373377284729,0.0930939531474212,
-0.946160508971352));
#42741=CARTESIAN_POINT('Ctrl Pts',(-0.0422592447626037,0.106150955031313,
-0.939811618626706));
#42742=CARTESIAN_POINT('Ctrl Pts',(-0.112096052568544,0.0220985072022432,
-0.933462728282062));
#42743=CARTESIAN_POINT('Ctrl Pts',(-0.0793846922795672,-0.0821701871341873,
-0.927113837937415));
#42744=CARTESIAN_POINT('Ctrl Pts',(0.0259496960417602,-0.111267615671996,
-0.920764947592771));
#42745=CARTESIAN_POINT('Ctrl Pts',(0.107544677571258,-0.0385747501364792,
-0.914416057248124));
#42746=CARTESIAN_POINT('Ctrl Pts',(0.0907551984479919,0.0694072256804634,
-0.908067166903481));
#42747=CARTESIAN_POINT('Ctrl Pts',(-0.00905932154553617,0.113893800161064,
-0.901718276558834));
#42748=CARTESIAN_POINT('Ctrl Pts',(-0.10058615604626,0.0541875837607848,
-0.895369386214191));
#42749=CARTESIAN_POINT('Ctrl Pts',(-0.100094352942304,-0.0550907390679732,
-0.889020495869543));
#42750=CARTESIAN_POINT('Ctrl Pts',(-0.00803382555549734,-0.113970727245806,
-0.8826716055249));
#42751=CARTESIAN_POINT('Ctrl Pts',(0.0913762388991208,-0.0685875497932755,
-0.876322715180253));
#42752=CARTESIAN_POINT('Ctrl Pts',(0.10719311972448,0.0395411697566919,
-0.86997382483561));
#42753=CARTESIAN_POINT('Ctrl Pts',(0.0249471534806576,0.111496675085882,
-0.863624934490962));
#42754=CARTESIAN_POINT('Ctrl Pts',(-0.0801210694795765,0.08145233727428,
-0.857276044146319));
#42755=CARTESIAN_POINT('Ctrl Pts',(-0.111892608813196,-0.0231065599986507,
-0.850927153801672));
#42756=CARTESIAN_POINT('Ctrl Pts',(-0.0413020952984331,-0.106527019792883,
-0.844578263457028));
#42757=CARTESIAN_POINT('Ctrl Pts',(0.0670725695247095,-0.0924939967746403,
-0.838229373112382));
#42758=CARTESIAN_POINT('Ctrl Pts',(0.114087632679905,0.00615476169231666,
-0.831880482767737));
#42759=CARTESIAN_POINT('Ctrl Pts',(0.0567325822986109,0.0991729959602187,
-0.825531592423091));
#42760=CARTESIAN_POINT('Ctrl Pts',(-0.0525228004555824,0.101465385498195,
-0.819182702078447));
#42761=CARTESIAN_POINT('Ctrl Pts',(-0.113729060635869,0.0109347971575568,
-0.8128338117338));
#42762=CARTESIAN_POINT('Ctrl Pts',(-0.0708932376197477,-0.0895992069260895,
-0.806484921389157));
#42763=CARTESIAN_POINT('Ctrl Pts',(0.0367974262370298,-0.108165699019257,
-0.80013603104451));
#42764=CARTESIAN_POINT('Ctrl Pts',(0.110824918512494,-0.027779605085262,
-0.793787140699865));
#42765=CARTESIAN_POINT('Ctrl Pts',(0.0834671067359925,0.0780199404967516,
-0.78743825035522));
#42766=CARTESIAN_POINT('Ctrl Pts',(-0.0202484241198383,0.112444965839549,
-0.781089360010574));
#42767=CARTESIAN_POINT('Ctrl Pts',(-0.105440209021084,0.0440026288258347,
-0.77474046966593));
#42768=CARTESIAN_POINT('Ctrl Pts',(-0.0941727517736408,-0.0646943725943335,
-0.768391579321284));
#42769=CARTESIAN_POINT('Ctrl Pts',(0.00324620641900389,-0.114207404164001,
-0.762042688976639));
#42770=CARTESIAN_POINT('Ctrl Pts',(0.0976954568128644,-0.0592407523595027,
-0.755693798631993));
#42771=CARTESIAN_POINT('Ctrl Pts',(0.102770550867044,0.0499207661848099,
-0.749344908287349));
#42772=CARTESIAN_POINT('Ctrl Pts',(0.0138286703355967,0.113413565761524,
-0.742996017942703));
#42773=CARTESIAN_POINT('Ctrl Pts',(-0.0877640108048387,0.0731529044498054,
-0.736647127598058));
#42774=CARTESIAN_POINT('Ctrl Pts',(-0.109068061556924,-0.0340297953301104,
-0.730298237253412));
#42775=CARTESIAN_POINT('Ctrl Pts',(-0.0305940233040475,-0.110081218925235,
-0.723949346908768));
#42776=CARTESIAN_POINT('Ctrl Pts',(0.0758681641528745,-0.0854276927586528,
-0.717600456564121));
#42777=CARTESIAN_POINT('Ctrl Pts',(0.112924328183426,0.0173771437905098,
-0.711251566219477));
#42778=CARTESIAN_POINT('Ctrl Pts',(0.046674597642533,0.104284950769043,
-0.704902675874831));
#42779=CARTESIAN_POINT('Ctrl Pts',(-0.0622741787177168,0.0957903736657717,
-0.698553785530186));
#42780=CARTESIAN_POINT('Ctrl Pts',(-0.114253036862592,-0.000335543840976016,
-0.692204895185541));
#42781=CARTESIAN_POINT('Ctrl Pts',(-0.061710465741824,-0.0961544977623059,
-0.685856004840896));
#42782=CARTESIAN_POINT('Ctrl Pts',(0.0472863253901056,-0.104009001788765,
-0.67950711449625));
#42783=CARTESIAN_POINT('Ctrl Pts',(0.113024447429166,-0.0167135665052596,
-0.673158224151605));
#42784=CARTESIAN_POINT('Ctrl Pts',(0.0753650833999685,0.0858718418697883,
-0.666809333806959));
#42785=CARTESIAN_POINT('Ctrl Pts',(-0.0312400736689609,0.10989962156055,
-0.660460443462316));
#42786=CARTESIAN_POINT('Ctrl Pts',(-0.109266059103523,0.0333885811315727,
-0.654111553117668));
#42787=CARTESIAN_POINT('Ctrl Pts',(-0.0873328226098335,-0.0736671372933253,
-0.647762662773025));
#42788=CARTESIAN_POINT('Ctrl Pts',(0.0144945829286659,-0.113330384662359,
-0.641413772428378));
#42789=CARTESIAN_POINT('Ctrl Pts',(0.103061994983266,-0.0493162672154266,
-0.635064882083734));
#42790=CARTESIAN_POINT('Ctrl Pts',(0.0973458123569227,0.0598135589859446,
-0.628715991739088));
#42791=CARTESIAN_POINT('Ctrl Pts',(0.00257533655841932,0.114224501152796,
-0.622367101394443));
#42792=CARTESIAN_POINT('Ctrl Pts',(-0.0945511191362657,0.0641401192084473,
-0.616018211049797));
#42793=CARTESIAN_POINT('Ctrl Pts',(-0.105179934311565,-0.0446211882429091,
-0.609669320705153));
#42794=CARTESIAN_POINT('Ctrl Pts',(-0.0195876129096983,-0.112561958238536,
-0.603320430360507));
#42795=CARTESIAN_POINT('Ctrl Pts',(0.0839239284397834,-0.0775283384139518,
-0.596971540015862));
#42796=CARTESIAN_POINT('Ctrl Pts',(0.11065983921532,0.028430072227023,-0.590622649671217));
#42797=CARTESIAN_POINT('Ctrl Pts',(0.0361614644549543,0.108379968215843,
-0.58427375932657));
#42798=CARTESIAN_POINT('Ctrl Pts',(-0.0714182887349078,0.0891812595569921,
-0.577924868981927));
#42799=CARTESIAN_POINT('Ctrl Pts',(-0.113662871681053,-0.0116026127751691,
-0.57157597863728));
#42800=CARTESIAN_POINT('Ctrl Pts',(-0.051925922680446,-0.101772135556735,
-0.565227088292636));
#42801=CARTESIAN_POINT('Ctrl Pts',(0.057314110732919,-0.09883805811978,
-0.55887819794799));
#42802=CARTESIAN_POINT('Ctrl Pts',(0.114121815558828,-0.00548454515443092,
-0.552529307603345));
#42803=CARTESIAN_POINT('Ctrl Pts',(0.0665281355275057,0.0928863617827071,
-0.546180417258698));
#42804=CARTESIAN_POINT('Ctrl Pts',(-0.041927084841482,0.106282588313841,
-0.539831526914056));
#42805=CARTESIAN_POINT('Ctrl Pts',(-0.11202639841874,0.0224489438352882,
-0.533482636569408));
#42806=CARTESIAN_POINT('Ctrl Pts',(-0.0796412651948913,-0.0819215350207207,
-0.527133746224765));
#42807=CARTESIAN_POINT('Ctrl Pts',(0.0256016151425451,-0.11134822101896,
-0.520784855880118));
#42808=CARTESIAN_POINT('Ctrl Pts',(0.107423521476236,-0.0389108732315119,
-0.514435965535474));
#42809=CARTESIAN_POINT('Ctrl Pts',(0.0909718036703051,0.0691230783383215,
-0.508087075190828));
#42810=CARTESIAN_POINT('Ctrl Pts',(-0.0087031106790096,0.113921573402508,
-0.501738184846182));
#42811=CARTESIAN_POINT('Ctrl Pts',(-0.100416209813545,0.0545018699557744,
-0.495389294501538));
#42812=CARTESIAN_POINT('Ctrl Pts',(-0.100266142249298,-0.0547774564984331,
-0.489040404156892));
#42813=CARTESIAN_POINT('Ctrl Pts',(-0.00839019340757563,-0.113945046739986,
-0.482691513812247));
#42814=CARTESIAN_POINT('Ctrl Pts',(0.0911613063941586,-0.06887296449627,
-0.476342623467602));
#42815=CARTESIAN_POINT('Ctrl Pts',(0.107316247997619,0.0392057640877946,
-0.469993733122956));
#42816=CARTESIAN_POINT('Ctrl Pts',(0.0252957018227751,0.111418115633354,
-0.463644842778311));
#42817=CARTESIAN_POINT('Ctrl Pts',(-0.0798659614846814,0.0817024921169577,
-0.457295952433666));
#42818=CARTESIAN_POINT('Ctrl Pts',(-0.111964320102099,-0.022756538534425,
-0.450947062089021));
#42819=CARTESIAN_POINT('Ctrl Pts',(-0.0416350226572824,-0.106397339770888,
-0.444598171744375));
#42820=CARTESIAN_POINT('Ctrl Pts',(0.0667829960604789,-0.0927032926016133,
-0.43824928139973));
#42821=CARTESIAN_POINT('Ctrl Pts',(0.114106321888124,0.00579795887860732,
-0.431900391055085));
#42822=CARTESIAN_POINT('Ctrl Pts',(0.0570424368415761,0.0989950979653487,
-0.425551500710439));
#42823=CARTESIAN_POINT('Ctrl Pts',(-0.0522052429748849,0.101629137691547,
-0.419202610365795));
#42824=CARTESIAN_POINT('Ctrl Pts',(-0.113694309447372,0.0112903950895989,
-0.412853720021149));
#42825=CARTESIAN_POINT('Ctrl Pts',(-0.071173083947476,-0.0893770728061716,
-0.406504829676504));
#42826=CARTESIAN_POINT('Ctrl Pts',(0.036458992552212,-0.10828024235322,
-0.400155939331858));
#42827=CARTESIAN_POINT('Ctrl Pts',(0.110737504754736,-0.0281260388730614,
-0.393807048987213));
#42828=CARTESIAN_POINT('Ctrl Pts',(0.0837106811157609,0.0777585422261086,
-0.387458158642568));
#42829=CARTESIAN_POINT('Ctrl Pts',(-0.0198966893102775,0.112507736518359,
-0.381109268297923));
#42830=CARTESIAN_POINT('Ctrl Pts',(-0.105302089255079,0.0443321443256423,
-0.374760377953277));
#42831=CARTESIAN_POINT('Ctrl Pts',(-0.0943746023389721,-0.0643995609872857,
-0.368411487608632));
#42832=CARTESIAN_POINT('Ctrl Pts',(0.00288904327994013,-0.114216997206724,
-0.362062597263987));
#42833=CARTESIAN_POINT('Ctrl Pts',(0.0975097225399547,-0.0595459741055193,
-0.355713706919342));
#42834=CARTESIAN_POINT('Ctrl Pts',(0.102926159645516,0.0495991399383105,
-0.349364816574696));
#42835=CARTESIAN_POINT('Ctrl Pts',(0.0141832675079377,0.113369766449404,
-0.343015926230051));
#42836=CARTESIAN_POINT('Ctrl Pts',(-0.0875348192703691,0.0734270007374531,
-0.336667035885406));
#42837=CARTESIAN_POINT('Ctrl Pts',(-0.109173945594853,-0.0336885533267078,
-0.33031814554076));
#42838=CARTESIAN_POINT('Ctrl Pts',(-0.0309381176468522,-0.10998500760769,
-0.323969255196116));
#42839=CARTESIAN_POINT('Ctrl Pts',(0.0756006452955727,-0.0856645285569653,
-0.31762036485147));
#42840=CARTESIAN_POINT('Ctrl Pts',(0.11297811750398,0.0170239239674976,
-0.311271474506825));
#42841=CARTESIAN_POINT('Ctrl Pts',(0.0470004873752844,0.104138480920743,
-0.304922584162179));
#42842=CARTESIAN_POINT('Ctrl Pts',(-0.0619743203475146,0.0959846479363122,
-0.298573693817534));
#42843=CARTESIAN_POINT('Ctrl Pts',(-0.114253527512409,2.17477677095862E-5,
-0.292224803472889));
#42844=CARTESIAN_POINT('Ctrl Pts',(-0.0620108565533915,-0.0959610477824666,
-0.285875913128243));
#42845=CARTESIAN_POINT('Ctrl Pts',(0.0469608391644364,-0.104156366137486,
-0.279527022783599));
#42846=CARTESIAN_POINT('Ctrl Pts',(0.11297162842615,-0.0170669327278882,
-0.273178132438953));
#42847=CARTESIAN_POINT('Ctrl Pts',(0.0756332517154119,0.0856357417025584,
-0.266829242094308));
#42848=CARTESIAN_POINT('Ctrl Pts',(-0.0308962448673541,0.109996777566847,
-0.260480351749662));
#42849=CARTESIAN_POINT('Ctrl Pts',(-0.109161112682653,0.0337301126573813,
-0.254131461405017));
#42850=CARTESIAN_POINT('Ctrl Pts',(-0.0875627660825531,-0.0733936715116903,
-0.247782571060372));
#42851=CARTESIAN_POINT('Ctrl Pts',(0.0141401073880872,-0.113375157706821,
-0.241433680715727));
#42852=CARTESIAN_POINT('Ctrl Pts',(0.102907270134931,-0.049638319626816,
-0.235084790371081));
#42853=CARTESIAN_POINT('Ctrl Pts',(0.0975323842177206,0.0595088485084162,
-0.228735900026436));
#42854=CARTESIAN_POINT('Ctrl Pts',(0.00293252469764535,0.114215889091171,
-0.222387009681791));
#42855=CARTESIAN_POINT('Ctrl Pts',(-0.0943500790294188,0.0644354840841576,
-0.216038119337145));
#42856=CARTESIAN_POINT('Ctrl Pts',(-0.105318958567443,-0.0442920533305308,
-0.2096892289925));
#42857=CARTESIAN_POINT('Ctrl Pts',(-0.0199395187920133,-0.112500153832397,
-0.203340338647855));
#42858=CARTESIAN_POINT('Ctrl Pts',(0.0836810729070069,-0.0777904046735807,
-0.196991448303209));
#42859=CARTESIAN_POINT('Ctrl Pts',(0.110748204119093,0.0280838798274333,
-0.190642557958565));
#42860=CARTESIAN_POINT('Ctrl Pts',(0.036500211457678,0.10826635481745,-0.184293667613919));
#42861=CARTESIAN_POINT('Ctrl Pts',(-0.0711390535560091,0.0894041614363504,
-0.177944777269274));
#42862=CARTESIAN_POINT('Ctrl Pts',(-0.11369859937654,-0.0112471116321533,
-0.171595886924628));
#42863=CARTESIAN_POINT('Ctrl Pts',(-0.0522439287224621,-0.101609256141691,
-0.165246996579984));
#42864=CARTESIAN_POINT('Ctrl Pts',(0.0570047459826288,-0.0990168064706588,
-0.158898106235338));
#42865=CARTESIAN_POINT('Ctrl Pts',(0.114104106321442,-0.00584139792443139,
-0.152549215890693));
#42866=CARTESIAN_POINT('Ctrl Pts',(0.0668182828326907,0.0926778620031539,
-0.146200325546047));
#42867=CARTESIAN_POINT('Ctrl Pts',(-0.0415945151008719,0.106413182328006,
-0.139851435201403));
#42868=CARTESIAN_POINT('Ctrl Pts',(-0.111955648355773,0.0227991607446998,
-0.133502544856757));
#42869=CARTESIAN_POINT('Ctrl Pts',(-0.079897059986415,-0.0816720814146227,
-0.127153654512112));
#42870=CARTESIAN_POINT('Ctrl Pts',(0.0252532852262649,-0.111427738139436,
-0.120804764167466));
#42871=CARTESIAN_POINT('Ctrl Pts',(0.107301312298338,-0.0392466145167992,
-0.114455873822821));
#42872=CARTESIAN_POINT('Ctrl Pts',(0.0911875241033174,0.0688382525769072,
-0.108106983478176));
#42873=CARTESIAN_POINT('Ctrl Pts',(-0.00834682390039813,0.113948237208761,
-0.101758093133531));
#42874=CARTESIAN_POINT('Ctrl Pts',(-0.10024526413777,0.0548156143681033,
-0.0954092027888852));
#42875=CARTESIAN_POINT('Ctrl Pts',(-0.100436984107331,-0.0544636215682244,
-0.0890603124442403));
#42876=CARTESIAN_POINT('Ctrl Pts',(-0.00874641646927006,-0.113918283558929,
-0.0827114220995946));
#42877=CARTESIAN_POINT('Ctrl Pts',(0.0909453634107706,-0.0691576456924166,
-0.0763625317549498));
#42878=CARTESIAN_POINT('Ctrl Pts',(0.10743855244889,0.0388698612665832,
-0.0700136414103045));
#42879=CARTESIAN_POINT('Ctrl Pts',(0.0256435748410253,0.111338682311979,
-0.0636647510656591));
#42880=CARTESIAN_POINT('Ctrl Pts',(-0.0796092608576849,0.0819514388563111,
-0.0573158607210139));
#42881=CARTESIAN_POINT('Ctrl Pts',(-0.112036475647968,-0.0224055186530005,
-0.0509669703763686));
#42882=CARTESIAN_POINT('Ctrl Pts',(-0.0419646237851041,-0.106268090710258,
-0.0446180800317233));
#42883=CARTESIAN_POINT('Ctrl Pts',(0.066487233315796,-0.0929088911131196,
-0.0382691896870782));
#42884=CARTESIAN_POINT('Ctrl Pts',(0.114134396399028,0.00543580541106296,
-0.0319202993424328));
#42885=CARTESIAN_POINT('Ctrl Pts',(0.0573318023082725,0.0988262831913889,
-0.0255714089977875));
#42886=CARTESIAN_POINT('Ctrl Pts',(-0.0518492415773505,0.101772737650102,
-0.0192225186531422));
#42887=CARTESIAN_POINT('Ctrl Pts',(-0.113731515237727,0.0116830253251869,
-0.0128736283084969));
#42888=CARTESIAN_POINT('Ctrl Pts',(-0.0713041863188721,-0.0892312379820752,
-0.00652473796385158));
#42889=CARTESIAN_POINT('Ctrl Pts',(7.37734688490074E-5,-0.101876700685701,
-0.0022921444007548));
#42890=CARTESIAN_POINT('Ctrl Pts',(0.0305629119072589,-0.091716759868353,
-0.000175847619206415));
#42891=CARTESIAN_POINT('Ctrl Pts',(-0.0967093838725941,-8.47898118814713E-5,
-0.0522235916889671));
#42892=CARTESIAN_POINT('Ctrl Pts',(-0.0967676968424891,-0.00643802185033027,
-0.0518047179181009));
#42893=CARTESIAN_POINT('Ctrl Pts',(-0.096195117326514,-0.0127808110712041,
-0.0513858441472348));
#42894=CARTESIAN_POINT('Ctrl Pts',(-0.0949532978724438,-0.0189897877443241,
-0.0509669703763687));
#42895=CARTESIAN_POINT('Ctrl Pts',(-0.0886791916936804,-0.0503597093387527,
-0.0488506735948202));
#42896=CARTESIAN_POINT('Ctrl Pts',(-0.0653219077393917,-0.0783139000245061,
-0.0467343768132717));
#42897=CARTESIAN_POINT('Ctrl Pts',(-0.0355679562454307,-0.0900644621011926,
-0.0446180800317233));
#42898=CARTESIAN_POINT('Ctrl Pts',(-0.00581400475147052,-0.101815024177879,
-0.0425017832501749));
#42899=CARTESIAN_POINT('Ctrl Pts',(0.0303366142821625,-0.0973619576454991,
-0.0403854864686265));
#42900=CARTESIAN_POINT('Ctrl Pts',(0.056353117646184,-0.0787446416252796,
-0.0382691896870782));
#42901=CARTESIAN_POINT('Ctrl Pts',(0.0823696210102062,-0.0601273256050595,
-0.0361528929055297));
#42902=CARTESIAN_POINT('Ctrl Pts',(0.0982520087046172,-0.0273457600969982,
-0.0340365961239812));
#42903=CARTESIAN_POINT('Ctrl Pts',(0.0967261035366966,0.00461010228708682,
-0.0319202993424328));
#42904=CARTESIAN_POINT('Ctrl Pts',(0.095200198368776,0.0365659646711728,
-0.0298040025608842));
#42905=CARTESIAN_POINT('Ctrl Pts',(0.0762660003385246,0.0676961239312805,
-0.0276877057793359));
#42906=CARTESIAN_POINT('Ctrl Pts',(0.0486020606757939,0.0837522793044539,
-0.0255714089977874));
#42907=CARTESIAN_POINT('Ctrl Pts',(0.0209381210130655,0.0998084346776261,
-0.0234551122162391));
#42908=CARTESIAN_POINT('Ctrl Pts',(-0.0154555602821406,0.100790586163864,
-0.0213388154346908));
#42909=CARTESIAN_POINT('Ctrl Pts',(-0.0439661132064728,0.0862667098528324,
-0.0192225186531425));
#42910=CARTESIAN_POINT('Ctrl Pts',(-0.0704497203496431,0.0727754024257818,
-0.0172566791020951));
#42911=CARTESIAN_POINT('Ctrl Pts',(-0.0901312497269368,0.0459044819879136,
-0.0152908395510477));
#42912=CARTESIAN_POINT('Ctrl Pts',(-0.0953948120465076,0.0166363274765985,
-0.0133250000000003));
#42913=CARTESIAN_POINT('',(-0.0601936375465013,0.0430788095790887,-1.149325));
#42914=CARTESIAN_POINT('Ctrl Pts',(-0.0601945574557614,0.0430798164930455,
-1.149325));
#42915=CARTESIAN_POINT('Ctrl Pts',(-0.0593969414063664,0.0446614288629473,
-1.149325));
#42916=CARTESIAN_POINT('Ctrl Pts',(-0.0585400474987182,0.0462093080774674,
-1.149325));
#42917=CARTESIAN_POINT('Ctrl Pts',(-0.057624700283891,0.0477197559654082,
-1.149325));
#42918=CARTESIAN_POINT('Ctrl Pts',(-0.0555316807570405,0.0511735239700963,
-1.149325));
#42919=CARTESIAN_POINT('Ctrl Pts',(-0.0531337632154356,0.0544318108953775,
-1.149325));
#42920=CARTESIAN_POINT('Ctrl Pts',(-0.0504744945711353,0.057482955786154,
-1.149325));
#42921=CARTESIAN_POINT('Ctrl Pts',(-0.0486009492640357,0.0596325912521487,
-1.149325));
#42922=CARTESIAN_POINT('Ctrl Pts',(-0.0465971933153744,0.061678830173069,
-1.149325));
#42923=CARTESIAN_POINT('Ctrl Pts',(-0.0444878921416535,0.0636076850959539,
-1.149325));
#42924=CARTESIAN_POINT('Ctrl Pts',(-0.0415466589643101,0.0662973020004301,
-1.149325));
#42925=CARTESIAN_POINT('Ctrl Pts',(-0.0383961696174096,0.0687641338366335,
-1.149325));
#42926=CARTESIAN_POINT('Ctrl Pts',(-0.0350729886334158,0.0709963287796745,
-1.149325));
#42927=CARTESIAN_POINT('Ctrl Pts',(-0.0327258042152802,0.0725729426366335,
-1.149325));
#42928=CARTESIAN_POINT('Ctrl Pts',(-0.0302911492173328,0.0740325115864712,
-1.149325));
#42929=CARTESIAN_POINT('Ctrl Pts',(-0.0277962837734336,0.0753625431214874,
-1.149325));
#42930=CARTESIAN_POINT('Ctrl Pts',(-0.0218327884651418,0.0785417273289343,
-1.149325));
#42931=CARTESIAN_POINT('Ctrl Pts',(-0.0155102394754001,0.0809963000056631,
-1.149325));
#42932=CARTESIAN_POINT('Ctrl Pts',(-0.0089852668252898,0.0826657982356903,
-1.149325));
#42933=CARTESIAN_POINT('Ctrl Pts',(-0.00663553819203132,0.0832670065479126,
-1.149325));
#42934=CARTESIAN_POINT('Ctrl Pts',(-0.00425676076600993,0.0837664401122449,
-1.149325));
#42935=CARTESIAN_POINT('Ctrl Pts',(-0.00186339920018093,0.0841586454601682,
-1.149325));
#42936=CARTESIAN_POINT('Ctrl Pts',(0.00212334881951441,0.0848119625002976,
-1.149325));
#42937=CARTESIAN_POINT('Ctrl Pts',(0.00613700862087291,0.0851664111597531,
-1.149325));
#42938=CARTESIAN_POINT('Ctrl Pts',(0.0101454841298669,0.0852107399416391,
-1.149325));
#42939=CARTESIAN_POINT('Ctrl Pts',(0.0153704726303765,0.0852685218527613,
-1.149325));
#42940=CARTESIAN_POINT('Ctrl Pts',(0.0205868041004565,0.0848003053162965,
-1.149325));
#42941=CARTESIAN_POINT('Ctrl Pts',(0.0257427285955276,0.0838507664789196,
-1.149325));
#42942=CARTESIAN_POINT('Ctrl Pts',(0.0288674016778731,0.0832753122711186,
-1.149325));
#42943=CARTESIAN_POINT('Ctrl Pts',(0.0319730906513826,0.0825211692425999,
-1.149325));
#42944=CARTESIAN_POINT('Ctrl Pts',(0.0350236518943335,0.0816043220267138,
-1.149325));
#42945=CARTESIAN_POINT('Ctrl Pts',(0.040291699894543,0.0800210084140771,
-1.149325));
#42946=CARTESIAN_POINT('Ctrl Pts',(0.0454099142546439,0.0779519494185946,
-1.149325));
#42947=CARTESIAN_POINT('Ctrl Pts',(0.050321493373422,0.0754465004076252,
-1.149325));
#42948=CARTESIAN_POINT('Ctrl Pts',(0.0539221601041848,0.073609761818822,
-1.149325));
#42949=CARTESIAN_POINT('Ctrl Pts',(0.057411918207577,0.0715380616425189,
-1.149325));
#42950=CARTESIAN_POINT('Ctrl Pts',(0.0607676654134175,0.0692448068755771,
-1.149325));
#42951=CARTESIAN_POINT('Ctrl Pts',(0.0631311994125498,0.0676296120239192,
-1.149325));
#42952=CARTESIAN_POINT('Ctrl Pts',(0.0654216850985366,0.0659085707891866,
-1.149325));
#42953=CARTESIAN_POINT('Ctrl Pts',(0.0676254903620251,0.0640927368991582,
-1.149325));
#42954=CARTESIAN_POINT('Ctrl Pts',(0.0734188261013449,0.0593192954585486,
-1.149325));
#42955=CARTESIAN_POINT('Ctrl Pts',(0.0786285494123232,0.0538847809587341,
-1.149325));
#42956=CARTESIAN_POINT('Ctrl Pts',(0.0831143226909517,0.0478769911187842,
-1.149325));
#42957=CARTESIAN_POINT('Ctrl Pts',(0.0844138435846824,0.0461365446144203,
-1.149325));
#42958=CARTESIAN_POINT('Ctrl Pts',(0.0856524500666806,0.0443476946186774,
-1.149325));
#42959=CARTESIAN_POINT('Ctrl Pts',(0.0868262223680489,0.042511912851507,
-1.149325));
#42960=CARTESIAN_POINT('Ctrl Pts',(-0.0601945574557609,0.0430798164930462,
-1.149325));
#42961=CARTESIAN_POINT('Ctrl Pts',(-0.0689950045553977,0.0306449443926568,
-1.14800758135659));
#42962=CARTESIAN_POINT('Ctrl Pts',(-0.0737382340313444,0.0152576839591632,
-1.14669016271317));
#42963=CARTESIAN_POINT('Ctrl Pts',(-0.0738510899558415,-6.10647340483529E-5,
-1.14537274406976));
#42964=CARTESIAN_POINT('Origin',(-2.39206768658147E-17,-5.43753587379397E-18,
-1.149325));
#42965=CARTESIAN_POINT('Ctrl Pts',(0.086954608065376,-0.0426125957048272,
-1.149325));
#42966=CARTESIAN_POINT('Ctrl Pts',(0.0857330349750578,-0.0445411053039618,
-1.149325));
#42967=CARTESIAN_POINT('Ctrl Pts',(0.0844400486091011,-0.0464202818838494,
-1.149325));
#42968=CARTESIAN_POINT('Ctrl Pts',(0.0830754117572655,-0.0482455415151559,
-1.149325));
#42969=CARTESIAN_POINT('Ctrl Pts',(0.0800390864492769,-0.0523067553133409,
-1.149325));
#42970=CARTESIAN_POINT('Ctrl Pts',(0.0766483379746834,-0.0561016838993785,
-1.149325));
#42971=CARTESIAN_POINT('Ctrl Pts',(0.0729515424226022,-0.059605136564689,
-1.149325));
#42972=CARTESIAN_POINT('Ctrl Pts',(0.070603271984809,-0.0618305921540642,
-1.149325));
#42973=CARTESIAN_POINT('Ctrl Pts',(0.0681306233770263,-0.063938250313155,
-1.149325));
#42974=CARTESIAN_POINT('Ctrl Pts',(0.0655584298678572,-0.0659112849073347,
-1.149325));
#42975=CARTESIAN_POINT('Ctrl Pts',(0.061295013787923,-0.0691815938421431,
-1.149325));
#42976=CARTESIAN_POINT('Ctrl Pts',(0.0567507752997466,-0.0720904225810572,
-1.149325));
#42977=CARTESIAN_POINT('Ctrl Pts',(0.0519830713174729,-0.0746026273715568,
-1.149325));
#42978=CARTESIAN_POINT('Ctrl Pts',(0.0495592178451569,-0.0758798073993565,
-1.149325));
#42979=CARTESIAN_POINT('Ctrl Pts',(0.047077602993811,-0.0770537891045191,
-1.149325));
#42980=CARTESIAN_POINT('Ctrl Pts',(0.0445587027673779,-0.0781143696302628,
-1.149325));
#42981=CARTESIAN_POINT('Ctrl Pts',(0.038135306482972,-0.0808189344784,-1.149325));
#42982=CARTESIAN_POINT('Ctrl Pts',(0.031448698113717,-0.0828009884055702,
-1.149325));
#42983=CARTESIAN_POINT('Ctrl Pts',(0.0246280221596509,-0.0839739399799056,
-1.149325));
#42984=CARTESIAN_POINT('Ctrl Pts',(0.0221514627490004,-0.0843998338765254,
-1.149325));
#42985=CARTESIAN_POINT('Ctrl Pts',(0.0196572765175813,-0.0847185915787331,
-1.149325));
#42986=CARTESIAN_POINT('Ctrl Pts',(0.0171520746182129,-0.0849244113167061,
-1.149325));
#42987=CARTESIAN_POINT('Ctrl Pts',(0.0146062307049426,-0.0851335700784337,
-1.149325));
#42988=CARTESIAN_POINT('Ctrl Pts',(0.0120579190174,-0.0852252699062859,
-1.149325));
#42989=CARTESIAN_POINT('Ctrl Pts',(0.00951710917596823,-0.0851952692846318,
-1.149325));
#42990=CARTESIAN_POINT('Ctrl Pts',(0.00767225013911105,-0.0851734861046915,
-1.149325));
#42991=CARTESIAN_POINT('Ctrl Pts',(0.00583076398118415,-0.0850875694335481,
-1.149325));
#42992=CARTESIAN_POINT('Ctrl Pts',(0.00399523787071753,-0.0849356509029418,
-1.149325));
#42993=CARTESIAN_POINT('Ctrl Pts',(-0.000130301487827045,-0.0845941979136682,
-1.149325));
#42994=CARTESIAN_POINT('Ctrl Pts',(-0.0042260125748701,-0.0839196884632143,
-1.149325));
#42995=CARTESIAN_POINT('Ctrl Pts',(-0.00825975656469361,-0.0829293963495848,
-1.149325));
#42996=CARTESIAN_POINT('Ctrl Pts',(-0.0108453319126542,-0.0822946324967623,
-1.149325));
#42997=CARTESIAN_POINT('Ctrl Pts',(-0.0134073686845953,-0.0815292810894073,
-1.149325));
#42998=CARTESIAN_POINT('Ctrl Pts',(-0.0159300211431115,-0.0806390832814289,
-1.149325));
#42999=CARTESIAN_POINT('Ctrl Pts',(-0.0221589550044849,-0.0784410067090031,
-1.149325));
#43000=CARTESIAN_POINT('Ctrl Pts',(-0.0281034482611466,-0.075502483957626,
-1.149325));
#43001=CARTESIAN_POINT('Ctrl Pts',(-0.0336303034371419,-0.0718981146415137,
-1.149325));
#43002=CARTESIAN_POINT('Ctrl Pts',(-0.0361277442859076,-0.070269394713553,
-1.149325));
#43003=CARTESIAN_POINT('Ctrl Pts',(-0.0385394333564065,-0.0685042094556212,
-1.149325));
#43004=CARTESIAN_POINT('Ctrl Pts',(-0.0408500806194884,-0.0666075686697806,
-1.149325));
#43005=CARTESIAN_POINT('Ctrl Pts',(-0.0424803759150722,-0.0652693788906776,
-1.149325));
#43006=CARTESIAN_POINT('Ctrl Pts',(-0.0440585000802111,-0.063866941402308,
-1.149325));
#43007=CARTESIAN_POINT('Ctrl Pts',(-0.0455732185102893,-0.06240842283285,
-1.149325));
#43008=CARTESIAN_POINT('Ctrl Pts',(-0.0499785755932977,-0.0581665155693797,
-1.149325));
#43009=CARTESIAN_POINT('Ctrl Pts',(-0.053867914455048,-0.053437905398849,
-1.149325));
#43010=CARTESIAN_POINT('Ctrl Pts',(-0.0571076045136135,-0.0482724182734906,
-1.149325));
#43011=CARTESIAN_POINT('Ctrl Pts',(-0.058182525399877,-0.0465585228395456,
-1.149325));
#43012=CARTESIAN_POINT('Ctrl Pts',(-0.0591855280879638,-0.0447964220518841,
-1.149325));
#43013=CARTESIAN_POINT('Ctrl Pts',(-0.0601104350279423,-0.042987737795231,
-1.149325));
#43014=CARTESIAN_POINT('Origin',(0.,0.,-1.149325));
#43015=CARTESIAN_POINT('Origin',(0.,0.,-1.25327725593024));
#43016=CARTESIAN_POINT('Ctrl Pts',(-0.0786356739692314,-0.056235988516294,
-1.16247415238079));
#43017=CARTESIAN_POINT('Ctrl Pts',(-0.0599413062053112,-0.0823766192285753,
-1.16035785559925));
#43018=CARTESIAN_POINT('Ctrl Pts',(0.00523751855363567,-0.11410112217152,
-1.15612526203615));
#43019=CARTESIAN_POINT('Ctrl Pts',(0.0988778236354322,-0.0573979516486903,
-1.1497763716915));
#43020=CARTESIAN_POINT('Ctrl Pts',(0.10176744392733,0.0518596603249867,
-1.14342748134686));
#43021=CARTESIAN_POINT('Ctrl Pts',(0.0117062229254556,0.113650929875517,
-1.13707859100221));
#43022=CARTESIAN_POINT('Ctrl Pts',(-0.0891415772947104,0.071484176152418,
-1.13072970065757));
#43023=CARTESIAN_POINT('Ctrl Pts',(-0.108399781825892,-0.0360846577190267,
-1.12438081031292));
#43024=CARTESIAN_POINT('Ctrl Pts',(-0.0285127216364505,-0.110638879749571,
-1.11803191996828));
#43025=CARTESIAN_POINT('Ctrl Pts',(0.077469779648326,-0.0839798348596053,
-1.11168302962363));
#43026=CARTESIAN_POINT('Ctrl Pts',(0.112575094334631,0.0195069576219953,
-1.10533413927899));
#43027=CARTESIAN_POINT('Ctrl Pts',(0.0446971480117591,0.105147802803276,
-1.09898524893434));
#43028=CARTESIAN_POINT('Ctrl Pts',(-0.0640724843747248,0.0945971764401096,
-1.0926363585897));
#43029=CARTESIAN_POINT('Ctrl Pts',(-0.114226190614228,-0.00249336732137551,
-1.08628746824505));
#43030=CARTESIAN_POINT('Ctrl Pts',(-0.0598834883344679,-0.0973028434580084,
-1.0799385779004));
#43031=CARTESIAN_POINT('Ctrl Pts',(0.0492423141801099,-0.103097375035228,
-1.07358968755576));
#43032=CARTESIAN_POINT('Ctrl Pts',(0.113319933754507,-0.0145759245129412,
-1.06724079721111));
#43033=CARTESIAN_POINT('Ctrl Pts',(0.0737298168519105,0.0872799217159805,
-1.06089190686647));
#43034=CARTESIAN_POINT('Ctrl Pts',(-0.0333101475173397,0.109289999720582,
-1.05454301652182));
#43035=CARTESIAN_POINT('Ctrl Pts',(-0.109877168057254,0.0313189512811141,
-1.04819412617718));
#43036=CARTESIAN_POINT('Ctrl Pts',(-0.0859259193914243,-0.0753034263167131,
-1.04184523583253));
#43037=CARTESIAN_POINT('Ctrl Pts',(0.0166324346020325,-0.11303641711073,
-1.03549634548789));
#43038=CARTESIAN_POINT('Ctrl Pts',(0.103975034167995,-0.047360971234609,
-1.02914745514324));
#43039=CARTESIAN_POINT('Ctrl Pts',(0.0961987702738092,0.0616414313136374,
-1.0227985647986));
#43040=CARTESIAN_POINT('Ctrl Pts',(0.000417554159368378,0.114252768332749,
-1.01644967445395));
#43041=CARTESIAN_POINT('Ctrl Pts',(-0.0957456501507325,0.0623429216779739,
-1.01010078410931));
#43042=CARTESIAN_POINT('Ctrl Pts',(-0.10431842841873,-0.0465997308728082,
-1.00375189376466));
#43043=CARTESIAN_POINT('Ctrl Pts',(-0.017458196332613,-0.11291182754622,
-0.997403003420017));
#43044=CARTESIAN_POINT('Ctrl Pts',(0.0853732140821567,-0.0759294655224641,
-0.991054113075372));
#43045=CARTESIAN_POINT('Ctrl Pts',(0.110103152550627,0.030514999891575,
-0.984705222730726));
#43046=CARTESIAN_POINT('Ctrl Pts',(0.0341080758322783,0.109043608624817,
-0.978356332386081));
#43047=CARTESIAN_POINT('Ctrl Pts',(-0.073089889950516,0.0878164984827856,
-0.972007442041436));
#43048=CARTESIAN_POINT('Ctrl Pts',(-0.113423464450988,-0.0137472590385073,
-0.96565855169679));
#43049=CARTESIAN_POINT('Ctrl Pts',(-0.0499945225011397,-0.102734692966118,
-0.959309661352146));
#43050=CARTESIAN_POINT('Ctrl Pts',(0.0591706124692214,-0.0977379559790979,
-0.952960771007499));
#43051=CARTESIAN_POINT('Ctrl Pts',(0.114205046360993,-0.00332818339188197,
-0.946611880662856));
#43052=CARTESIAN_POINT('Ctrl Pts',(0.0647619538532123,0.09412629150292,
-0.940262990318209));
#43053=CARTESIAN_POINT('Ctrl Pts',(-0.0439269334678215,0.105471768426881,
-0.933914099973564));
#43054=CARTESIAN_POINT('Ctrl Pts',(-0.112430404318708,0.020329131897814,
-0.927565209628919));
#43055=CARTESIAN_POINT('Ctrl Pts',(-0.0780798340429289,-0.0834110840045326,
-0.921216319284272));
#43056=CARTESIAN_POINT('Ctrl Pts',(0.0277000485302825,-0.110844831771279,
-0.91486742893963));
#43057=CARTESIAN_POINT('Ctrl Pts',(0.108139259707659,-0.0368750583574256,
-0.908518538594982));
#43058=CARTESIAN_POINT('Ctrl Pts',(0.0896500721767574,0.0708289063708139,
-0.902169648250338));
#43059=CARTESIAN_POINT('Ctrl Pts',(-0.0108531601007334,0.113736882033979,
-0.895820757905693));
#43060=CARTESIAN_POINT('Ctrl Pts',(-0.101427660180571,0.0525956192974108,
-0.889471867561047));
#43061=CARTESIAN_POINT('Ctrl Pts',(-0.0992136944107583,-0.0566613824430021,
-0.883122977216402));
#43062=CARTESIAN_POINT('Ctrl Pts',(-0.00623665198847288,-0.114083187152876,
-0.876774086871757));
#43063=CARTESIAN_POINT('Ctrl Pts',(0.0924458298476606,-0.0671389452014324,
-0.870425196527112));
#43064=CARTESIAN_POINT('Ctrl Pts',(0.106556640499711,0.0412256204853105,
-0.864076306182466));
#43065=CARTESIAN_POINT('Ctrl Pts',(0.0231868706034319,0.111875995864185,
-0.857727415837821));
#43066=CARTESIAN_POINT('Ctrl Pts',(-0.0813948068466306,0.0801795163204622,
-0.851378525493176));
#43067=CARTESIAN_POINT('Ctrl Pts',(-0.111514555055875,-0.0248671154272822,
-0.845029635148529));
#43068=CARTESIAN_POINT('Ctrl Pts',(-0.039618103097239,-0.10716471119711,
-0.838680744803886));
#43069=CARTESIAN_POINT('Ctrl Pts',(0.0685219435546145,-0.0914254487026546,
-0.832331854459239));
#43070=CARTESIAN_POINT('Ctrl Pts',(0.113976466275917,0.00795201573427383,
-0.825982964114595));
#43071=CARTESIAN_POINT('Ctrl Pts',(0.0551625731639185,0.100054784697779,
-0.819634073769949));
#43072=CARTESIAN_POINT('Ctrl Pts',(-0.0541153701596963,0.100625027361301,
-0.813285183425305));
#43073=CARTESIAN_POINT('Ctrl Pts',(-0.113887269795971,0.00914107200515301,
-0.806936293080658));
#43074=CARTESIAN_POINT('Ctrl Pts',(-0.0694723526865942,-0.0907053561327721,
-0.800587402736014));
#43075=CARTESIAN_POINT('Ctrl Pts',(0.0384975455125421,-0.107572340350544,
-0.794238512391367));
#43076=CARTESIAN_POINT('Ctrl Pts',(0.111248962079288,-0.0260295573390085,
-0.787889622046723));
#43077=CARTESIAN_POINT('Ctrl Pts',(0.0822271493284522,0.0793256915021855,
-0.781540731702078));
#43078=CARTESIAN_POINT('Ctrl Pts',(-0.0220180396078722,0.112111887642701,
-0.775191841357432));
#43079=CARTESIAN_POINT('Ctrl Pts',(-0.106120595729893,0.0423354293815024,
-0.768842951012787));
#43080=CARTESIAN_POINT('Ctrl Pts',(-0.093141475558706,-0.0661704990893252,
-0.762494060668143));
#43081=CARTESIAN_POINT('Ctrl Pts',(0.00504570924375355,-0.114142061647804,
-0.756145170323495));
#43082=CARTESIAN_POINT('Ctrl Pts',(0.0986169577324141,-0.0576937177393419,
-0.749796279978852));
#43083=CARTESIAN_POINT('Ctrl Pts',(0.101971038651006,0.0515342283867572,
-0.743447389634206));
#43084=CARTESIAN_POINT('Ctrl Pts',(0.0120395580109721,0.113617421471727,
-0.73709849928956));
#43085=CARTESIAN_POINT('Ctrl Pts',(-0.0889060002027456,0.0717606615558481,
-0.730749608944917));
#43086=CARTESIAN_POINT('Ctrl Pts',(-0.108518208628496,-0.0357444795044725,
-0.724400718600269));
#43087=CARTESIAN_POINT('Ctrl Pts',(-0.0288553467483356,-0.110549710008741,
-0.718051828255626));
#43088=CARTESIAN_POINT('Ctrl Pts',(0.0772050811564295,-0.0842214038271311,
-0.711702937910979));
#43089=CARTESIAN_POINT('Ctrl Pts',(0.112636441767823,0.019154670575798,
-0.705354047566334));
#43090=CARTESIAN_POINT('Ctrl Pts',(0.0450252732328951,0.105007591103151,
-0.699005157221689));
#43091=CARTESIAN_POINT('Ctrl Pts',(-0.0637760994367215,0.0947970387703165,
-0.692656266877044));
#43092=CARTESIAN_POINT('Ctrl Pts',(-0.114233560651881,-0.00213612728472956,
-0.686307376532398));
#43093=CARTESIAN_POINT('Ctrl Pts',(-0.0601874099079299,-0.0971151126630577,
-0.679958486187754));
#43094=CARTESIAN_POINT('Ctrl Pts',(0.0489196326960759,-0.103250854504282,
-0.673609595843107));
#43095=CARTESIAN_POINT('Ctrl Pts',(0.113273817354663,-0.0149302284271154,
-0.667260705498463));
#43096=CARTESIAN_POINT('Ctrl Pts',(0.0740023863324715,0.0870489301260112,
-0.660911815153817));
#43097=CARTESIAN_POINT('Ctrl Pts',(-0.0329682096391889,0.109393631314487,
-0.654562924809173));
#43098=CARTESIAN_POINT('Ctrl Pts',(-0.109778693578452,0.0316624044442602,
-0.648214034464526));
#43099=CARTESIAN_POINT('Ctrl Pts',(-0.0861609852278712,-0.0750343524230471,
-0.641865144119882));
#43100=CARTESIAN_POINT('Ctrl Pts',(0.0162788671133667,-0.113087876912112,
-0.635516253775236));
#43101=CARTESIAN_POINT('Ctrl Pts',(0.103826419834063,-0.0476858885145751,
-0.629167363430591));
#43102=CARTESIAN_POINT('Ctrl Pts',(0.096391063613419,0.0613402989433316,
-0.622818473085946));
#43103=CARTESIAN_POINT('Ctrl Pts',(0.000774841360944117,0.11425090389073,
-0.616469582741301));
#43104=CARTESIAN_POINT('Ctrl Pts',(-0.0955502244262325,0.062642030866505,
-0.610120692396655));
#43105=CARTESIAN_POINT('Ctrl Pts',(-0.104463644116912,-0.0462732803764618,
-0.603771802052011));
#43106=CARTESIAN_POINT('Ctrl Pts',(-0.0178112067483281,-0.11285668049855,
-0.597422911707364));
#43107=CARTESIAN_POINT('Ctrl Pts',(0.0851353514366683,-0.0761960717802332,
-0.59107402136272));
#43108=CARTESIAN_POINT('Ctrl Pts',(0.110198040119839,0.0301705381577773,
-0.584725131018074));
#43109=CARTESIAN_POINT('Ctrl Pts',(0.0344489081994947,0.108936413300817,
-0.578376240673429));
#43110=CARTESIAN_POINT('Ctrl Pts',(-0.0728149144505367,0.08804463443359,
-0.572027350328784));
#43111=CARTESIAN_POINT('Ctrl Pts',(-0.113465900022296,-0.013392496074814,
-0.565678459984138));
#43112=CARTESIAN_POINT('Ctrl Pts',(-0.0503155480636912,-0.102577848690806,
-0.559329569639494));
#43113=CARTESIAN_POINT('Ctrl Pts',(0.0588646788314206,-0.097922515312145,
-0.552980679294847));
#43114=CARTESIAN_POINT('Ctrl Pts',(0.114194080105829,-0.00368530701123027,
-0.546631788950203));
#43115=CARTESIAN_POINT('Ctrl Pts',(0.0650559871753232,0.0939233088835127,
-0.540282898605557));
#43116=CARTESIAN_POINT('Ctrl Pts',(-0.0435968893318331,0.105608620195377,
-0.533934008260913));
#43117=CARTESIAN_POINT('Ctrl Pts',(-0.112366281691608,0.0206806227610694,
-0.527585117916266));
#43118=CARTESIAN_POINT('Ctrl Pts',(-0.0783402938480742,-0.0831665063519015,
-0.521236227571622));
#43119=CARTESIAN_POINT('Ctrl Pts',(0.0273532811943798,-0.110930912855185,
-0.514887337226976));
#43120=CARTESIAN_POINT('Ctrl Pts',(0.108023415949815,-0.0372130491295291,
-0.508538446882331));
#43121=CARTESIAN_POINT('Ctrl Pts',(0.0898711286561028,0.0705482080074449,
-0.502189556537686));
#43122=CARTESIAN_POINT('Ctrl Pts',(-0.0104974311744136,0.113770265701201,
-0.495840666193041));
#43123=CARTESIAN_POINT('Ctrl Pts',(-0.101262688194809,0.0529125448125908,
-0.489491775848395));
#43124=CARTESIAN_POINT('Ctrl Pts',(-0.0993903997105554,-0.0563508461725251,
-0.48314288550375));
#43125=CARTESIAN_POINT('Ctrl Pts',(-0.00659338031061752,-0.114063126184859,
-0.476793995159105));
#43126=CARTESIAN_POINT('Ctrl Pts',(0.0922354221620667,-0.0674277117924733,
-0.47044510481446));
#43127=CARTESIAN_POINT('Ctrl Pts',(0.106685039467939,0.0408921969660201,
-0.464096214469814));
#43128=CARTESIAN_POINT('Ctrl Pts',(0.0235366137575775,0.111802939280728,
-0.45774732412517));
#43129=CARTESIAN_POINT('Ctrl Pts',(-0.081143672965582,0.080433660594543,
-0.451398433780523));
#43130=CARTESIAN_POINT('Ctrl Pts',(-0.111591773769459,-0.0245182675972318,
-0.445049543435879));
#43131=CARTESIAN_POINT('Ctrl Pts',(-0.0399530328668883,-0.107040294206064,
-0.438700653091233));
#43132=CARTESIAN_POINT('Ctrl Pts',(0.0682357045470802,-0.0916392822099074,
-0.432351762746588));
#43133=CARTESIAN_POINT('Ctrl Pts',(0.114000776367053,0.00759555177013864,
-0.426002872401942));
#43134=CARTESIAN_POINT('Ctrl Pts',(0.0554751928969789,0.0998817920945878,
-0.419653982057298));
#43135=CARTESIAN_POINT('Ctrl Pts',(-0.0538004328442067,0.10079376391801,
-0.413305091712651));
#43136=CARTESIAN_POINT('Ctrl Pts',(-0.113858127137762,0.00949717345661038,
-0.406956201368007));
#43137=CARTESIAN_POINT('Ctrl Pts',(-0.0697556650911323,-0.0904876599690656,
-0.400607311023361));
#43138=CARTESIAN_POINT('Ctrl Pts',(0.0381609590549173,-0.107692203167139,
-0.394258420678717));
#43139=CARTESIAN_POINT('Ctrl Pts',(0.111167018964811,-0.0263773257450609,
-0.387909530334071));
#43140=CARTESIAN_POINT('Ctrl Pts',(0.0824748130913862,0.0790681644185857,
-0.381560639989426));
#43141=CARTESIAN_POINT('Ctrl Pts',(-0.0216673377414524,0.112180193858725,
-0.37521174964478));
#43142=CARTESIAN_POINT('Ctrl Pts',(-0.105987686272075,0.042667080725961,
-0.368862859300135));
#43143=CARTESIAN_POINT('Ctrl Pts',(-0.0933479472818827,-0.0658789052523071,
-0.36251396895549));
#43144=CARTESIAN_POINT('Ctrl Pts',(0.00468874164365965,-0.114157282381732,
-0.356165078610845));
#43145=CARTESIAN_POINT('Ctrl Pts',(0.09843605681153,-0.0580018287503136,
-0.349816188266199));
#43146=CARTESIAN_POINT('Ctrl Pts',(0.102131696927743,0.0512150944707055,
-0.343467297921554));
#43147=CARTESIAN_POINT('Ctrl Pts',(0.0123948014252152,0.113579216041549,
-0.337118407576909));
#43148=CARTESIAN_POINT('Ctrl Pts',(-0.0886811568803896,0.0720383358590353,
-0.330769517232263));
#43149=CARTESIAN_POINT('Ctrl Pts',(-0.108629457483411,-0.0354049486067051,
-0.324420626887619));
#43150=CARTESIAN_POINT('Ctrl Pts',(-0.0292009146492382,-0.11045893355737,
-0.318071736542973));
#43151=CARTESIAN_POINT('Ctrl Pts',(0.0769413280463485,-0.0844624263057108,
-0.311722846198328));
#43152=CARTESIAN_POINT('Ctrl Pts',(0.112695791144682,0.0188023423343459,
-0.305373955853682));
#43153=CARTESIAN_POINT('Ctrl Pts',(0.0453534308576449,0.104866275457958,
-0.299025065509037));
#43154=CARTESIAN_POINT('Ctrl Pts',(-0.0634793400610372,0.094996014676399,
-0.292676175164392));
#43155=CARTESIAN_POINT('Ctrl Pts',(-0.114239682147924,-0.0017788877774734,
-0.286327284819747));
#43156=CARTESIAN_POINT('Ctrl Pts',(-0.0604908121837178,-0.0969264208579767,
-0.279978394475101));
#43157=CARTESIAN_POINT('Ctrl Pts',(0.0485965093481745,-0.103403330208249,
-0.273629504130457));
#43158=CARTESIAN_POINT('Ctrl Pts',(0.113226573953927,-0.0152843831946183,
-0.267280613785811));
#43159=CARTESIAN_POINT('Ctrl Pts',(0.074274242279478,0.0868170856041166,
-0.260931723441166));
#43160=CARTESIAN_POINT('Ctrl Pts',(-0.0326259547108729,0.109496193989502,
-0.25458283309652));
#43161=CARTESIAN_POINT('Ctrl Pts',(-0.109679142718567,0.0320055475114412,
-0.248233942751875));
#43162=CARTESIAN_POINT('Ctrl Pts',(-0.0863952099601143,-0.074764544504249,
-0.24188505240723));
#43163=CARTESIAN_POINT('Ctrl Pts',(0.0159251412139454,-0.113138230922594,
-0.235536162062585));
#43164=CARTESIAN_POINT('Ctrl Pts',(0.103676789737939,-0.0480103393931116,
-0.229187271717939));
#43165=CARTESIAN_POINT('Ctrl Pts',(0.0965824145351879,0.0610385666731131,
-0.222838381373294));
#43166=CARTESIAN_POINT('Ctrl Pts',(0.0011321208704043,0.114247922174953,
-0.216489491028648));
#43167=CARTESIAN_POINT('Ctrl Pts',(-0.0953538642286377,0.0629405274509425,
-0.210140600684003));
#43168=CARTESIAN_POINT('Ctrl Pts',(-0.104607838265844,-0.045946377355595,
-0.203791710339358));
#43169=CARTESIAN_POINT('Ctrl Pts',(-0.0181640429686614,-0.112800429794994,
-0.197442819994713));
#43170=CARTESIAN_POINT('Ctrl Pts',(0.0848966562237705,-0.0764619328946917,
-0.191093929650067));
#43171=CARTESIAN_POINT('Ctrl Pts',(0.11029185002685,0.029825781379531,-0.184745039305422));
#43172=CARTESIAN_POINT('Ctrl Pts',(0.0347894036947918,0.108828152651674,
-0.178396148960777));
#43173=CARTESIAN_POINT('Ctrl Pts',(-0.0725392269022447,0.0882719093800321,
-0.172047258616132));
#43174=CARTESIAN_POINT('Ctrl Pts',(-0.113507225919962,-0.0130376021601832,
-0.165698368271487));
#43175=CARTESIAN_POINT('Ctrl Pts',(-0.0506360816870214,-0.102420001242717,
-0.159349477926841));
#43176=CARTESIAN_POINT('Ctrl Pts',(0.0585581697499888,-0.0981061170983672,
-0.153000587582196));
#43177=CARTESIAN_POINT('Ctrl Pts',(0.114181996713574,-0.00404239446648764,
-0.146651697237551));
#43178=CARTESIAN_POINT('Ctrl Pts',(0.0653493850557507,0.0937194075251059,
-0.140302806892906));
#43179=CARTESIAN_POINT('Ctrl Pts',(-0.0432664202898733,0.105744439634424,
-0.13395391654826));
#43180=CARTESIAN_POINT('Ctrl Pts',(-0.112301057470237,0.0210319105336957,
-0.127605026203615));
#43181=CARTESIAN_POINT('Ctrl Pts',(-0.0785999927227247,-0.0829211137801427,
-0.121256135858969));
#43182=CARTESIAN_POINT('Ctrl Pts',(0.02700625619051,-0.111015912167295,
-0.114907245514325));
#43183=CARTESIAN_POINT('Ctrl Pts',(0.107906497161016,-0.0375506701933854,
-0.108558355169679));
#43184=CARTESIAN_POINT('Ctrl Pts',(0.0900913416102402,0.0702668087494677,
-0.102209464825034));
#43185=CARTESIAN_POINT('Ctrl Pts',(-0.0101416666357262,0.113802557607322,
-0.0958605744803883));
#43186=CARTESIAN_POINT('Ctrl Pts',(-0.101096598775461,0.0532289133730042,
-0.0895116841357433));
#43187=CARTESIAN_POINT('Ctrl Pts',(-0.0995663742066905,-0.0560396839009997,
-0.0831627937910978));
#43188=CARTESIAN_POINT('Ctrl Pts',(-0.00694958676658794,-0.114042091871885,
-0.0768139034464529));
#43189=CARTESIAN_POINT('Ctrl Pts',(0.0920232450043284,-0.0677155494623698,
-0.0704650131018075));
#43190=CARTESIAN_POINT('Ctrl Pts',(0.106814040378024,0.0405578623688256,
-0.0641161227571624));
#43191=CARTESIAN_POINT('Ctrl Pts',(0.0238830063610432,0.111729758858221,
-0.057767232412517));
#43192=CARTESIAN_POINT('Ctrl Pts',(-0.0808858272408635,0.0806851793959811,
-0.0514183420678718));
#43193=CARTESIAN_POINT('Ctrl Pts',(-0.111679127879553,-0.024165691358642,
-0.0450694517232264));
#43194=CARTESIAN_POINT('Ctrl Pts',(-0.0402662619737551,-0.106921455580305,
-0.0387205613785813));
#43195=CARTESIAN_POINT('Ctrl Pts',(0.0679082340930717,-0.0918395816349683,
-0.0323716710339359));
#43196=CARTESIAN_POINT('Ctrl Pts',(0.114102150823536,0.00721443260332955,
-0.0260227806892906));
#43197=CARTESIAN_POINT('Ctrl Pts',(0.0556285462168408,0.0997595234912466,
-0.0196738903446454));
#43198=CARTESIAN_POINT('Ctrl Pts',(-0.0168574189684883,0.100472359437058,
-0.0154412967815485));
#43199=CARTESIAN_POINT('Ctrl Pts',(-0.0452560140322605,0.0854280329804675,
-0.013325));
#43200=CARTESIAN_POINT('Ctrl Pts',(-0.0724605943221351,-0.0518199049426062,
-1.1580911015872));
#43201=CARTESIAN_POINT('Ctrl Pts',(-0.055234252507093,-0.075907771705324,
-1.15597480480565));
#43202=CARTESIAN_POINT('Ctrl Pts',(0.0048262281991512,-0.105141021982032,
-1.15174221124255));
#43203=CARTESIAN_POINT('Ctrl Pts',(0.0911131742662497,-0.0528906217674777,
-1.14539332089791));
#43204=CARTESIAN_POINT('Ctrl Pts',(0.0937758792848175,0.0477872397960602,
-1.13904443055326));
#43205=CARTESIAN_POINT('Ctrl Pts',(0.010786960009752,0.104726182257502,
-1.13269554020861));
#43206=CARTESIAN_POINT('Ctrl Pts',(-0.0821414930851173,0.0658706872743175,
-1.12634664986397));
#43207=CARTESIAN_POINT('Ctrl Pts',(-0.0998873948555119,-0.0332510120693374,
-1.11999775951932));
#43208=CARTESIAN_POINT('Ctrl Pts',(-0.0262736828112808,-0.101950661539774,
-1.11364886917468));
#43209=CARTESIAN_POINT('Ctrl Pts',(0.0713862550159982,-0.0773850904791992,
-1.10729997883003));
#43210=CARTESIAN_POINT('Ctrl Pts',(0.103734829621343,0.0179751208498506,
-1.10095108848539));
#43211=CARTESIAN_POINT('Ctrl Pts',(0.0411871831950449,0.0968907863086817,
-1.09460219814074));
#43212=CARTESIAN_POINT('Ctrl Pts',(-0.0590410187023357,0.0871686765058855,
-1.0882533077961));
#43213=CARTESIAN_POINT('Ctrl Pts',(-0.10525626908595,-0.00229756888763826,
-1.08190441745145));
#43214=CARTESIAN_POINT('Ctrl Pts',(-0.055180974941425,-0.0896618736803812,
-1.07555552710681));
#43215=CARTESIAN_POINT('Ctrl Pts',(0.0453754278584056,-0.0950013739441941,
-1.06920663676216));
#43216=CARTESIAN_POINT('Ctrl Pts',(0.104421178504928,-0.013431310494212,
-1.06285774641752));
#43217=CARTESIAN_POINT('Ctrl Pts',(0.0679399829451714,0.0804260290616174,
-1.05650885607287));
#43218=CARTESIAN_POINT('Ctrl Pts',(-0.0306943778088397,0.100707705974746,
-1.05015996572823));
#43219=CARTESIAN_POINT('Ctrl Pts',(-0.101248765324717,0.0288595456594365,
-1.04381107538358));
#43220=CARTESIAN_POINT('Ctrl Pts',(-0.0791783534431802,-0.0693900204573446,
-1.03746218503894));
#43221=CARTESIAN_POINT('Ctrl Pts',(0.0153263275489798,-0.104159925774821,
-1.03111329469429));
#43222=CARTESIAN_POINT('Ctrl Pts',(0.0958101125123582,-0.0436418224720267,
-1.02476440434965));
#43223=CARTESIAN_POINT('Ctrl Pts',(0.0886445008384644,0.0568008706786289,
-1.018415514005));
#43224=CARTESIAN_POINT('Ctrl Pts',(0.000384764586127094,0.105280759717015,
-1.01206662366036));
#43225=CARTESIAN_POINT('Ctrl Pts',(-0.0882269632024242,0.0574472746088744,
-1.00571773331571));
#43226=CARTESIAN_POINT('Ctrl Pts',(-0.0961265407978823,-0.042940360574977,
-0.999368842971065));
#43227=CARTESIAN_POINT('Ctrl Pts',(-0.0160872440992713,-0.104045119943892,
-0.993019952626418));
#43228=CARTESIAN_POINT('Ctrl Pts',(0.0786690508178819,-0.069966898235941,
-0.986671062281774));
#43229=CARTESIAN_POINT('Ctrl Pts',(0.101457003772623,0.028118726733982,
-0.980322171937128));
#43230=CARTESIAN_POINT('Ctrl Pts',(0.0314296466379681,0.100480663408266,
-0.973973281592484));
#43231=CARTESIAN_POINT('Ctrl Pts',(-0.0673503080399109,0.0809204696820091,
-0.967624391247837));
#43232=CARTESIAN_POINT('Ctrl Pts',(-0.104516579172577,-0.0126677182244316,
-0.961275500903192));
#43233=CARTESIAN_POINT('Ctrl Pts',(-0.0460685669801909,-0.0946671724685623,
-0.954926610558547));
#43234=CARTESIAN_POINT('Ctrl Pts',(0.0545240795876188,-0.0900628178102374,
-0.948577720213902));
#43235=CARTESIAN_POINT('Ctrl Pts',(0.105236785242567,-0.00306682876124731,
-0.942228829869257));
#43236=CARTESIAN_POINT('Ctrl Pts',(0.0596763457194078,0.0867347690859587,
-0.935879939524611));
#43237=CARTESIAN_POINT('Ctrl Pts',(-0.0404774518378589,0.097189311652734,
-0.929531049179967));
#43238=CARTESIAN_POINT('Ctrl Pts',(-0.103601501781483,0.0187327316599986,
-0.923182158835321));
#43239=CARTESIAN_POINT('Ctrl Pts',(-0.0719484032341107,-0.0768610023281135,
-0.916833268490676));
#43240=CARTESIAN_POINT('Ctrl Pts',(0.0255248270656589,-0.102140440620203,
-0.91048437814603));
#43241=CARTESIAN_POINT('Ctrl Pts',(0.0996473309434417,-0.0339793443531499,
-0.904135487801385));
#43242=CARTESIAN_POINT('Ctrl Pts',(0.0826100570269412,0.0652668743301431,
-0.89778659745674));
#43243=CARTESIAN_POINT('Ctrl Pts',(-0.0100008862578078,0.104805384789522,
-0.891437707112095));
#43244=CARTESIAN_POINT('Ctrl Pts',(-0.0934627779786483,0.0484654055934257,
-0.885088816767449));
#43245=CARTESIAN_POINT('Ctrl Pts',(-0.0914226698776842,-0.0522118936570709,
-0.878739926422805));
#43246=CARTESIAN_POINT('Ctrl Pts',(-0.00574690197024275,-0.105124495359387,
-0.872391036078158));
#43247=CARTESIAN_POINT('Ctrl Pts',(0.0851862702414863,-0.0618666773729265,
-0.866042145733514));
#43248=CARTESIAN_POINT('Ctrl Pts',(0.0981889912026475,0.0379882667863077,
-0.859693255388868));
#43249=CARTESIAN_POINT('Ctrl Pts',(0.0213660586803464,0.103090629755033,
-0.853344365044224));
#43250=CARTESIAN_POINT('Ctrl Pts',(-0.0750030588044541,0.0738832022640935,
-0.846995474699577));
#43251=CARTESIAN_POINT('Ctrl Pts',(-0.102757572066831,-0.0229143577206821,
-0.840646584354933));
#43252=CARTESIAN_POINT('Ctrl Pts',(-0.0365069840625374,-0.0987493114987594,
-0.834297694010287));
#43253=CARTESIAN_POINT('Ctrl Pts',(0.0631410720281716,-0.0842460172943181,
-0.827948803665642));
#43254=CARTESIAN_POINT('Ctrl Pts',(0.105026155028839,0.00732756212390092,
-0.821599913320996));
#43255=CARTESIAN_POINT('Ctrl Pts',(0.0508307824430911,0.0921977112679295,
-0.815251022976352));
#43256=CARTESIAN_POINT('Ctrl Pts',(-0.0498658138959695,0.0927231740791579,
-0.808902132631705));
#43257=CARTESIAN_POINT('Ctrl Pts',(-0.104943962944481,0.00842324452504938,
-0.802553242287061));
#43258=CARTESIAN_POINT('Ctrl Pts',(-0.0640168477044826,-0.0835824719471878,
-0.796204351942415));
#43259=CARTESIAN_POINT('Ctrl Pts',(0.0354744213023932,-0.0991249304669698,
-0.789855461597771));
#43260=CARTESIAN_POINT('Ctrl Pts',(0.102512835499318,-0.0239855157274384,
-0.783506571253125));
#43261=CARTESIAN_POINT('Ctrl Pts',(0.0757700393346405,0.0730964263562066,
-0.777157680908479));
#43262=CARTESIAN_POINT('Ctrl Pts',(-0.0202890133098994,0.103307997491637,
-0.770808790563835));
#43263=CARTESIAN_POINT('Ctrl Pts',(-0.0977871880314241,0.0390109249278746,
-0.764459900219188));
#43264=CARTESIAN_POINT('Ctrl Pts',(-0.0858272884856976,-0.0609742811192895,
-0.758111009874544));
#43265=CARTESIAN_POINT('Ctrl Pts',(0.00464948123573095,-0.105178746574866,
-0.751762119529899));
#43266=CARTESIAN_POINT('Ctrl Pts',(0.0908727935660286,-0.0531631620234097,
-0.745413229185254));
#43267=CARTESIAN_POINT('Ctrl Pts',(0.0939634861804381,0.0474873632837188,
-0.739064338840607));
#43268=CARTESIAN_POINT('Ctrl Pts',(0.0110941190532975,0.104695305192032,
-0.732715448495963));
#43269=CARTESIAN_POINT('Ctrl Pts',(-0.0819244153234499,0.0661254609113028,
-0.726366558151318));
#43270=CARTESIAN_POINT('Ctrl Pts',(-0.0999965218721342,-0.0329375472720281,
-0.720017667806672));
#43271=CARTESIAN_POINT('Ctrl Pts',(-0.0265894023566692,-0.101868494094771,
-0.713668777462027));
#43272=CARTESIAN_POINT('Ctrl Pts',(0.0711423426913388,-0.0776076895881424,
-0.707319887117382));
#43273=CARTESIAN_POINT('Ctrl Pts',(0.103791359580901,0.0176504980997559,
-0.700970996772737));
#43274=CARTESIAN_POINT('Ctrl Pts',(0.0414895414929455,0.0967615851127215,
-0.69462210642809));
#43275=CARTESIAN_POINT('Ctrl Pts',(-0.0587679081957195,0.087352844104361,
-0.688273216083447));
#43276=CARTESIAN_POINT('Ctrl Pts',(-0.1052630603714,-0.00196838209410804,
-0.681924325738799));
#43277=CARTESIAN_POINT('Ctrl Pts',(-0.0554610302487527,-0.0894888849554417,
-0.675575435394156));
#43278=CARTESIAN_POINT('Ctrl Pts',(0.0450780858133816,-0.0951428010215314,
-0.66922654504951));
#43279=CARTESIAN_POINT('Ctrl Pts',(0.104378683520503,-0.0137577917322536,
-0.662877654704865));
#43280=CARTESIAN_POINT('Ctrl Pts',(0.0681911481677555,0.0802131767129601,
-0.65652876436022));
#43281=CARTESIAN_POINT('Ctrl Pts',(-0.0303792915302921,0.100803199616574,
-0.650179874015574));
#43282=CARTESIAN_POINT('Ctrl Pts',(-0.101158023821536,0.0291760282311139,
-0.643830983670929));
#43283=CARTESIAN_POINT('Ctrl Pts',(-0.0793949600970565,-0.0691420763212106,
-0.637482093326283));
#43284=CARTESIAN_POINT('Ctrl Pts',(0.0150005249066355,-0.104207344555683,
-0.631133202981639));
#43285=CARTESIAN_POINT('Ctrl Pts',(0.0956731685222073,-0.0439412247410412,
-0.624784312636993));
#43286=CARTESIAN_POINT('Ctrl Pts',(0.0888216938218651,0.056523385544712,
-0.618435422292349));
#43287=CARTESIAN_POINT('Ctrl Pts',(0.000713994840833118,0.105279041685364,
-0.612086531947701));
#43288=CARTESIAN_POINT('Ctrl Pts',(-0.0880468838131556,0.0577228954368544,
-0.605737641603059));
#43289=CARTESIAN_POINT('Ctrl Pts',(-0.0962603530393757,-0.0426395454895582,
-0.599388751258411));
#43290=CARTESIAN_POINT('Ctrl Pts',(-0.0164125334143298,-0.103994303467761,
-0.593039860913768));
#43291=CARTESIAN_POINT('Ctrl Pts',(0.0784498669819821,-0.0702125685139818,
-0.586690970569121));
#43292=CARTESIAN_POINT('Ctrl Pts',(0.101544440038021,0.0278013147923997,
-0.580342080224476));
#43293=CARTESIAN_POINT('Ctrl Pts',(0.0317437142188269,0.100381885887917,
-0.573993189879831));
#43294=CARTESIAN_POINT('Ctrl Pts',(-0.0670969257371112,0.0811306906383144,
-0.567644299535187));
#43295=CARTESIAN_POINT('Ctrl Pts',(-0.104555682375514,-0.0123408139849797,
-0.56129540919054));
#43296=CARTESIAN_POINT('Ctrl Pts',(-0.0463643831394596,-0.0945226448155085,
-0.554946518845896));
#43297=CARTESIAN_POINT('Ctrl Pts',(0.0542421702187635,-0.0902328841209236,
-0.54859762850125));
#43298=CARTESIAN_POINT('Ctrl Pts',(0.105226680142342,-0.00339590827946428,
-0.542248738156605));
#43299=CARTESIAN_POINT('Ctrl Pts',(0.0599472892771499,0.0865477262274584,
-0.53589984781196));
#43300=CARTESIAN_POINT('Ctrl Pts',(-0.040173325313101,0.0973154167648122,
-0.529550957467314));
#43301=CARTESIAN_POINT('Ctrl Pts',(-0.103542414557649,0.0190566207495772,
-0.523202067122669));
#43302=CARTESIAN_POINT('Ctrl Pts',(-0.0721884097263963,-0.0766356307992258,
-0.516853176778024));
#43303=CARTESIAN_POINT('Ctrl Pts',(0.0252052905756322,-0.102219761953447,
-0.510504286433378));
#43304=CARTESIAN_POINT('Ctrl Pts',(0.0995405841309819,-0.0342907934828616,
-0.504155396088733));
#43305=CARTESIAN_POINT('Ctrl Pts',(0.0828137544464914,0.0650082185673283,
-0.497806505744088));
#43306=CARTESIAN_POINT('Ctrl Pts',(-0.00967309191056538,0.104836146913701,
-0.491457615399442));
#43307=CARTESIAN_POINT('Ctrl Pts',(-0.0933107608656584,0.0487574436726666,
-0.485108725054797));
#43308=CARTESIAN_POINT('Ctrl Pts',(-0.0915854989143904,-0.0519257430897579,
-0.478759834710152));
#43309=CARTESIAN_POINT('Ctrl Pts',(-0.00607561723304139,-0.105106009733311,
-0.472410944365507));
#43310=CARTESIAN_POINT('Ctrl Pts',(0.0849923853902668,-0.0621327677839452,
-0.466062054020862));
#43311=CARTESIAN_POINT('Ctrl Pts',(0.098307307293533,0.0376810262534904,
-0.459713163676216));
#43312=CARTESIAN_POINT('Ctrl Pts',(0.0216883373044148,0.103023310138003,
-0.453364273331571));
#43313=CARTESIAN_POINT('Ctrl Pts',(-0.0747716458927733,0.0741173891695262,
-0.447015382986926));
#43314=CARTESIAN_POINT('Ctrl Pts',(-0.102828726971427,-0.0225929041129553,
-0.44066649264228));
#43315=CARTESIAN_POINT('Ctrl Pts',(-0.0368156125633175,-0.0986346646894945,
-0.434317602297635));
#43316=CARTESIAN_POINT('Ctrl Pts',(0.062877310715307,-0.0844430589452562,
-0.42796871195299));
#43317=CARTESIAN_POINT('Ctrl Pts',(0.105048556104111,0.00699909045968183,
-0.421619821608345));
#43318=CARTESIAN_POINT('Ctrl Pts',(0.0511188528634354,0.0920383033782552,
-0.4152709312637));
#43319=CARTESIAN_POINT('Ctrl Pts',(-0.049575607887644,0.0928786601399474,
-0.408922040919054));
#43320=CARTESIAN_POINT('Ctrl Pts',(-0.104917108792576,0.00875138214388225,
-0.402573150574409));
#43321=CARTESIAN_POINT('Ctrl Pts',(-0.0642779122337915,-0.083381870965374,
-0.396224260229764));
#43322=CARTESIAN_POINT('Ctrl Pts',(0.0351642662095556,-0.0992353807306885,
-0.389875369885118));
#43323=CARTESIAN_POINT('Ctrl Pts',(0.102437327190227,-0.0243059746758653,
-0.383526479540474));
#43324=CARTESIAN_POINT('Ctrl Pts',(0.0759982546286465,0.0728591222855505,
-0.377177589195827));
#43325=CARTESIAN_POINT('Ctrl Pts',(-0.0199658512590393,0.103370939776724,
-0.370828698851183));
#43326=CARTESIAN_POINT('Ctrl Pts',(-0.0976647156493817,0.0393165324506968,
-0.364479808506537));
#43327=CARTESIAN_POINT('Ctrl Pts',(-0.0860175464566275,-0.0607055854794545,
-0.358130918161892));
#43328=CARTESIAN_POINT('Ctrl Pts',(0.00432054548493318,-0.105192772059367,
-0.351782027817247));
#43329=CARTESIAN_POINT('Ctrl Pts',(0.0907060983807646,-0.0534470777813002,
-0.345433137472601));
#43330=CARTESIAN_POINT('Ctrl Pts',(0.0941115283301076,0.0471932902242764,
-0.339084247127957));
#43331=CARTESIAN_POINT('Ctrl Pts',(0.0114214660146163,0.104660099946915,
-0.332735356783311));
#43332=CARTESIAN_POINT('Ctrl Pts',(-0.0817172284330107,0.0663813300864664,
-0.326386466438666));
#43333=CARTESIAN_POINT('Ctrl Pts',(-0.100099034608884,-0.0326246789591988,
-0.32003757609402));
#43334=CARTESIAN_POINT('Ctrl Pts',(-0.0269078336005834,-0.101784846110532,
-0.313688685749375));
#43335=CARTESIAN_POINT('Ctrl Pts',(0.0708993015098229,-0.0778297851226668,
-0.30733979540473));
#43336=CARTESIAN_POINT('Ctrl Pts',(0.103846048386919,0.0173258373893755,
-0.300990905060084));
#43337=CARTESIAN_POINT('Ctrl Pts',(0.0417919296498781,0.0966313666619745,
-0.294642014715439));
#43338=CARTESIAN_POINT('Ctrl Pts',(-0.0584944526551572,0.0875361948875711,
-0.288293124370794));
#43339=CARTESIAN_POINT('Ctrl Pts',(-0.105268701160358,-0.00163919578839571,
-0.281944234026149));
#43340=CARTESIAN_POINT('Ctrl Pts',(-0.0557406070376653,-0.0893150106862998,
-0.275595343681503));
#43341=CARTESIAN_POINT('Ctrl Pts',(0.0447803366030493,-0.0952833031571579,
-0.269246453336859));
#43342=CARTESIAN_POINT('Ctrl Pts',(0.104335150035986,-0.0140841355357712,
-0.262897562992213));
#43343=CARTESIAN_POINT('Ctrl Pts',(0.0684416558889433,0.0799995384111712,
-0.256548672647568));
#43344=CARTESIAN_POINT('Ctrl Pts',(-0.0300639130988035,0.100897708279267,
-0.250199782302922));
#43345=CARTESIAN_POINT('Ctrl Pts',(-0.101066290463019,0.0294922250579535,
-0.243850891958277));
#43346=CARTESIAN_POINT('Ctrl Pts',(-0.0796107916967184,-0.0688934558012595,
-0.237502001613632));
#43347=CARTESIAN_POINT('Ctrl Pts',(0.0146745762931698,-0.104253744380875,
-0.231153111268987));
#43348=CARTESIAN_POINT('Ctrl Pts',(0.0955352885353473,-0.0442401972340638,
-0.224804220924341));
#43349=CARTESIAN_POINT('Ctrl Pts',(0.0889980183933423,0.0562453476196506,
-0.218455330579696));
#43350=CARTESIAN_POINT('Ctrl Pts',(0.00104321800746791,0.105276294116908,
-0.212106440235051));
#43351=CARTESIAN_POINT('Ctrl Pts',(-0.0878659433328274,0.0579979517671395,
-0.205757549890405));
#43352=CARTESIAN_POINT('Ctrl Pts',(-0.0963932239515455,-0.0423383134153348,
-0.19940865954576));
#43353=CARTESIAN_POINT('Ctrl Pts',(-0.0167376622131716,-0.103942470003317,
-0.193059769201115));
#43354=CARTESIAN_POINT('Ctrl Pts',(0.078229915958288,-0.0704575521631122,
-0.18671087885647));
#43355=CARTESIAN_POINT('Ctrl Pts',(0.101630883267566,0.0274836309755344,
-0.180361988511825));
#43356=CARTESIAN_POINT('Ctrl Pts',(0.0320574713815479,0.100282126699974,
-0.174013098167179));
#43357=CARTESIAN_POINT('Ctrl Pts',(-0.0668428873015247,0.0813401182029611,
-0.167664207822534));
#43358=CARTESIAN_POINT('Ctrl Pts',(-0.104593763044944,-0.012013789077868,
-0.161315317477889));
#43359=CARTESIAN_POINT('Ctrl Pts',(-0.046659745990369,-0.0943771927665409,
-0.154966427133243));
#43360=CARTESIAN_POINT('Ctrl Pts',(0.0539597305945496,-0.0904020680787478,
-0.148617536788598));
#43361=CARTESIAN_POINT('Ctrl Pts',(0.105215545631247,-0.00372495447347343,
-0.142268646443953));
#43362=CARTESIAN_POINT('Ctrl Pts',(0.0602176472929908,0.0863598367764309,
-0.135919756099308));
#43363=CARTESIAN_POINT('Ctrl Pts',(-0.0398688072492659,0.0974405706139124,
-0.129570865754662));
#43364=CARTESIAN_POINT('Ctrl Pts',(-0.103482312245223,0.0193803226967692,
-0.123221975410017));
#43365=CARTESIAN_POINT('Ctrl Pts',(-0.0724277150423184,-0.0764095083449458,
-0.116873085065372));
#43366=CARTESIAN_POINT('Ctrl Pts',(0.0248855166517145,-0.102298086463958,
-0.110524194720727));
#43367=CARTESIAN_POINT('Ctrl Pts',(0.0994328467072885,-0.0346019019366694,
-0.104175304376081));
#43368=CARTESIAN_POINT('Ctrl Pts',(0.0830166745809391,0.0647489169495561,
-0.0978264140314359));
#43369=CARTESIAN_POINT('Ctrl Pts',(-0.00934526474751318,0.104865903010281,
-0.0914775236867907));
#43370=CARTESIAN_POINT('Ctrl Pts',(-0.0931577140685862,0.0490489685335253,
-0.0851286333421453));
#43371=CARTESIAN_POINT('Ctrl Pts',(-0.0917476545357751,-0.0516390156798273,
-0.0787797429975));
#43372=CARTESIAN_POINT('Ctrl Pts',(-0.00640385161062303,-0.105086627196832,
-0.0724308526528549));
#43373=CARTESIAN_POINT('Ctrl Pts',(0.0847968700195037,-0.0623980022198728,
-0.0660819623082098));
#43374=CARTESIAN_POINT('Ctrl Pts',(0.0984261780571572,0.0373729461876333,
-0.0597330719635643));
#43375=CARTESIAN_POINT('Ctrl Pts',(0.0220075284888858,0.102955876406722,
-0.0533841816189193));
#43376=CARTESIAN_POINT('Ctrl Pts',(-0.0745340482031569,0.0743491567746786,
-0.0470352912742738));
#43377=CARTESIAN_POINT('Ctrl Pts',(-0.102909221363023,-0.0222680148800854,
-0.0406864009296286));
#43378=CARTESIAN_POINT('Ctrl Pts',(-0.037104244504737,-0.0985251581892469,
-0.0343375105849833));
#43379=CARTESIAN_POINT('Ctrl Pts',(0.0625755557671689,-0.0846276293145263,
-0.027988620240338));
#43380=CARTESIAN_POINT('Ctrl Pts',(0.105141969856357,0.00664789970947171,
-0.0216397298956927));
#43381=CARTESIAN_POINT('Ctrl Pts',(0.051260163697788,0.0919256362487216,
-0.0152908395510475));
#43382=CARTESIAN_POINT('Ctrl Pts',(-0.0155336444076485,0.0925824948178739,
-0.0110582459879506));
#43383=CARTESIAN_POINT('Ctrl Pts',(-0.0417021627450095,0.0787195649134732,
-0.00894194920640216));
#43384=CARTESIAN_POINT('Ctrl Pts',(-0.0662855146750388,-0.0474038213689184,
-1.1537080507936));
#43385=CARTESIAN_POINT('Ctrl Pts',(-0.0505271988088748,-0.0694389241820727,
-1.15159175401205));
#43386=CARTESIAN_POINT('Ctrl Pts',(0.00441493784466667,-0.0961809217925434,
-1.14735916044895));
#43387=CARTESIAN_POINT('Ctrl Pts',(0.0833485248970674,-0.0483832918862652,
-1.14101027010431));
#43388=CARTESIAN_POINT('Ctrl Pts',(0.0857843146423046,0.043714819267134,
-1.13466137975966));
#43389=CARTESIAN_POINT('Ctrl Pts',(0.00986769709404836,0.0958014346394865,
-1.12831248941502));
#43390=CARTESIAN_POINT('Ctrl Pts',(-0.0751414088755243,0.0602571983962171,
-1.12196359907037));
#43391=CARTESIAN_POINT('Ctrl Pts',(-0.0913750078851314,-0.0304173664196481,
-1.11561470872573));
#43392=CARTESIAN_POINT('Ctrl Pts',(-0.024034643986111,-0.0932624433299762,
-1.10926581838108));
#43393=CARTESIAN_POINT('Ctrl Pts',(0.0653027303836705,-0.070790346098793,
-1.10291692803644));
#43394=CARTESIAN_POINT('Ctrl Pts',(0.0948945649080561,0.016443284077706,
-1.09656803769179));
#43395=CARTESIAN_POINT('Ctrl Pts',(0.0376772183783308,0.0886337698140873,
-1.09021914734715));
#43396=CARTESIAN_POINT('Ctrl Pts',(-0.0540095530299468,0.0797401765716616,
-1.0838702570025));
#43397=CARTESIAN_POINT('Ctrl Pts',(-0.0962863475576708,-0.00210177045390104,
-1.07752136665785));
#43398=CARTESIAN_POINT('Ctrl Pts',(-0.0504784615483822,-0.0820209039027542,
-1.07117247631321));
#43399=CARTESIAN_POINT('Ctrl Pts',(0.0415085415367013,-0.0869053728531599,
-1.06482358596856));
#43400=CARTESIAN_POINT('Ctrl Pts',(0.0955224232553502,-0.0122866964754829,
-1.05847469562392));
#43401=CARTESIAN_POINT('Ctrl Pts',(0.0621501490384322,0.0735721364072543,
-1.05212580527927));
#43402=CARTESIAN_POINT('Ctrl Pts',(-0.0280786081003397,0.0921254122289098,
-1.04577691493463));
#43403=CARTESIAN_POINT('Ctrl Pts',(-0.0926203625921804,0.0264001400377588,
-1.03942802458998));
#43404=CARTESIAN_POINT('Ctrl Pts',(-0.0724307874949361,-0.0634766145979759,
-1.03307913424534));
#43405=CARTESIAN_POINT('Ctrl Pts',(0.0140202204959272,-0.0952834344389127,
-1.02673024390069));
#43406=CARTESIAN_POINT('Ctrl Pts',(0.0876451908567207,-0.0399226737094445,
-1.02038135355605));
#43407=CARTESIAN_POINT('Ctrl Pts',(0.0810902314031199,0.0519603100436204,
-1.0140324632114));
#43408=CARTESIAN_POINT('Ctrl Pts',(0.000351975012885768,0.0963087511012804,
-1.00768357286676));
#43409=CARTESIAN_POINT('Ctrl Pts',(-0.0807082762541159,0.0525516275397749,
-1.00133468252211));
#43410=CARTESIAN_POINT('Ctrl Pts',(-0.0879346531770343,-0.0392809902771458,
-0.994985792177466));
#43411=CARTESIAN_POINT('Ctrl Pts',(-0.0147162918659295,-0.0951784123415638,
-0.988636901832821));
#43412=CARTESIAN_POINT('Ctrl Pts',(0.071964887553607,-0.0640043309494178,
-0.982288011488176));
#43413=CARTESIAN_POINT('Ctrl Pts',(0.0928108549946201,0.0257224535763889,
-0.975939121143531));
#43414=CARTESIAN_POINT('Ctrl Pts',(0.0287512174436577,0.0919177181917147,
-0.969590230798886));
#43415=CARTESIAN_POINT('Ctrl Pts',(-0.0616107261293058,0.0740244408812324,
-0.963241340454239));
#43416=CARTESIAN_POINT('Ctrl Pts',(-0.0956096938941654,-0.0115881774103558,
-0.956892450109595));
#43417=CARTESIAN_POINT('Ctrl Pts',(-0.0421426114592421,-0.0865996519710071,
-0.950543559764949));
#43418=CARTESIAN_POINT('Ctrl Pts',(0.0498775467060162,-0.0823876796413767,
-0.944194669420304));
#43419=CARTESIAN_POINT('Ctrl Pts',(0.0962685241241404,-0.00280547413061279,
-0.937845779075659));
#43420=CARTESIAN_POINT('Ctrl Pts',(0.0545907375856034,0.0793432466689976,
-0.931496888731014));
#43421=CARTESIAN_POINT('Ctrl Pts',(-0.0370279702078962,0.0889068548785865,
-0.925147998386368));
#43422=CARTESIAN_POINT('Ctrl Pts',(-0.0947725992442585,0.0171363314221833,
-0.918799108041723));
#43423=CARTESIAN_POINT('Ctrl Pts',(-0.0658169724252926,-0.0703109206516945,
-0.912450217697078));
#43424=CARTESIAN_POINT('Ctrl Pts',(0.0233496056010352,-0.0934360494691271,
-0.906101327352432));
#43425=CARTESIAN_POINT('Ctrl Pts',(0.0911554021792248,-0.0310836303488742,
-0.899752437007787));
#43426=CARTESIAN_POINT('Ctrl Pts',(0.0755700418771249,0.0597048422894724,
-0.893403546663142));
#43427=CARTESIAN_POINT('Ctrl Pts',(-0.00914861241488205,0.0958738875450639,
-0.887054656318497));
#43428=CARTESIAN_POINT('Ctrl Pts',(-0.0854978957767257,0.0443351918894408,
-0.880705765973851));
#43429=CARTESIAN_POINT('Ctrl Pts',(-0.0836316453446097,-0.0477624048711401,
-0.874356875629207));
#43430=CARTESIAN_POINT('Ctrl Pts',(-0.00525715195201284,-0.0961658035658973,
-0.86800798528456));
#43431=CARTESIAN_POINT('Ctrl Pts',(0.0779267106353122,-0.056594409544421,
-0.861659094939916));
#43432=CARTESIAN_POINT('Ctrl Pts',(0.0898213419055841,0.0347509130873053,
-0.85531020459527));
#43433=CARTESIAN_POINT('Ctrl Pts',(0.019545246757261,0.0943052636458809,
-0.848961314250626));
#43434=CARTESIAN_POINT('Ctrl Pts',(-0.0686113107622776,0.0675868882077251,
-0.84261242390598));
#43435=CARTESIAN_POINT('Ctrl Pts',(-0.0940005890777867,-0.0209616000140822,
-0.836263533561334));
#43436=CARTESIAN_POINT('Ctrl Pts',(-0.0333958650278359,-0.0903339118004081,
-0.82991464321669));
#43437=CARTESIAN_POINT('Ctrl Pts',(0.0577602005017288,-0.0770665858859817,
-0.823565752872044));
#43438=CARTESIAN_POINT('Ctrl Pts',(0.09607584378176,0.00670310851352802,
-0.817216862527399));
#43439=CARTESIAN_POINT('Ctrl Pts',(0.0464989917222637,0.0843406378380802,
-0.810867972182753));
#43440=CARTESIAN_POINT('Ctrl Pts',(-0.0456162576322428,0.084821320797015,
-0.804519081838108));
#43441=CARTESIAN_POINT('Ctrl Pts',(-0.0960006560929914,0.00770541704494582,
-0.798170191493463));
#43442=CARTESIAN_POINT('Ctrl Pts',(-0.058561342722371,-0.0764595877616036,
-0.791821301148817));
#43443=CARTESIAN_POINT('Ctrl Pts',(0.0324512970922443,-0.0906775205833958,
-0.785472410804173));
#43444=CARTESIAN_POINT('Ctrl Pts',(0.0937767089193475,-0.0219414741158684,
-0.779123520459527));
#43445=CARTESIAN_POINT('Ctrl Pts',(0.0693129293408286,0.0668671612102279,
-0.772774630114882));
#43446=CARTESIAN_POINT('Ctrl Pts',(-0.0185599870119265,0.0945041073405723,
-0.766425739770236));
#43447=CARTESIAN_POINT('Ctrl Pts',(-0.0894537803329552,0.0356864204742467,
-0.760076849425591));
#43448=CARTESIAN_POINT('Ctrl Pts',(-0.0785131014126889,-0.0557780631492537,
-0.753727959080947));
#43449=CARTESIAN_POINT('Ctrl Pts',(0.0042532532277082,-0.0962154315019286,
-0.747379068736299));
#43450=CARTESIAN_POINT('Ctrl Pts',(0.0831286293996434,-0.0486326063074775,
-0.741030178391657));
#43451=CARTESIAN_POINT('Ctrl Pts',(0.08595593370987,0.0434404981806807,
-0.734681288047009));
#43452=CARTESIAN_POINT('Ctrl Pts',(0.0101486800956229,0.0957731889123362,
-0.728332397702366));
#43453=CARTESIAN_POINT('Ctrl Pts',(-0.0749428304441543,0.0604902602667578,
-0.721983507357719));
#43454=CARTESIAN_POINT('Ctrl Pts',(-0.0914748351157721,-0.0301306150395839,
-0.715634617013074));
#43455=CARTESIAN_POINT('Ctrl Pts',(-0.0243234579650029,-0.0931872781808012,
-0.70928572666843));
#43456=CARTESIAN_POINT('Ctrl Pts',(0.0650796042262482,-0.0709939753491537,
-0.702936836323783));
#43457=CARTESIAN_POINT('Ctrl Pts',(0.0949462773939787,0.0161463256237138,
-0.696587945979139));
#43458=CARTESIAN_POINT('Ctrl Pts',(0.0379538097529958,0.0885155791222918,
-0.690239055634493));
#43459=CARTESIAN_POINT('Ctrl Pts',(-0.0537597169547176,0.0799086494384053,
-0.683890165289848));
#43460=CARTESIAN_POINT('Ctrl Pts',(-0.0962925600909185,-0.00180063690348633,
-0.677541274945203));
#43461=CARTESIAN_POINT('Ctrl Pts',(-0.0507346505895757,-0.0818626572478259,
-0.671192384600557));
#43462=CARTESIAN_POINT('Ctrl Pts',(0.0412365389306873,-0.0870347475387801,
-0.664843494255913));
#43463=CARTESIAN_POINT('Ctrl Pts',(0.0954835496863418,-0.0125853550373922,
-0.658494603911266));
#43464=CARTESIAN_POINT('Ctrl Pts',(0.0623799100030393,0.0733774232999093,
-0.652145713566622));
#43465=CARTESIAN_POINT('Ctrl Pts',(-0.0277903734213952,0.0922127679186605,
-0.645796823221977));
#43466=CARTESIAN_POINT('Ctrl Pts',(-0.0925373540646213,0.0266896520179679,
-0.639447932877331));
#43467=CARTESIAN_POINT('Ctrl Pts',(-0.0726289349662417,-0.0632498002193741,
-0.633099042532686));
#43468=CARTESIAN_POINT('Ctrl Pts',(0.0137221826999042,-0.0953268121992537,
-0.626750152188041));
#43469=CARTESIAN_POINT('Ctrl Pts',(0.0875199172103516,-0.0401965609675073,
-0.620401261843396));
#43470=CARTESIAN_POINT('Ctrl Pts',(0.0812523240303111,0.0517064721460925,
-0.61405237149875));
#43471=CARTESIAN_POINT('Ctrl Pts',(0.000653148320722093,0.0963071794799973,
-0.607703481154105));
#43472=CARTESIAN_POINT('Ctrl Pts',(-0.0805435432000787,0.0528037600072041,
-0.60135459080946));
#43473=CARTESIAN_POINT('Ctrl Pts',(-0.0880570619618391,-0.0390058106026548,
-0.595005700464814));
#43474=CARTESIAN_POINT('Ctrl Pts',(-0.0150138600803315,-0.0951319264369724,
-0.588656810120169));
#43475=CARTESIAN_POINT('Ctrl Pts',(0.0717643825272961,-0.0642290652477304,
-0.582307919775524));
#43476=CARTESIAN_POINT('Ctrl Pts',(0.0928908399562031,0.025432091427022,
-0.575959029430878));
#43477=CARTESIAN_POINT('Ctrl Pts',(0.029038520238159,0.0918273584750176,
-0.569610139086234));
#43478=CARTESIAN_POINT('Ctrl Pts',(-0.0613789370236857,0.0742167468430388,
-0.563261248741587));
#43479=CARTESIAN_POINT('Ctrl Pts',(-0.095645464728733,-0.0112891318951454,
-0.556912358396944));
#43480=CARTESIAN_POINT('Ctrl Pts',(-0.0424132182152278,-0.0864674409402106,
-0.550563468052297));
#43481=CARTESIAN_POINT('Ctrl Pts',(0.0496196616061063,-0.0825432529297025,
-0.544214577707653));
#43482=CARTESIAN_POINT('Ctrl Pts',(0.0962592801788553,-0.00310650954769815,
-0.537865687363006));
#43483=CARTESIAN_POINT('Ctrl Pts',(0.0548385913789765,0.0791721435714039,
-0.531516797018362));
#43484=CARTESIAN_POINT('Ctrl Pts',(-0.0367497612943688,0.0890222133342473,
-0.525167906673716));
#43485=CARTESIAN_POINT('Ctrl Pts',(-0.0947185474236903,0.0174326187380849,
-0.518819016329072));
#43486=CARTESIAN_POINT('Ctrl Pts',(-0.0660365256047182,-0.0701047552465502,
-0.512470125984425));
#43487=CARTESIAN_POINT('Ctrl Pts',(0.0230572999568844,-0.0935086110517078,
-0.506121235639781));
#43488=CARTESIAN_POINT('Ctrl Pts',(0.0910577523121486,-0.0313685378361942,
-0.499772345295134));
#43489=CARTESIAN_POINT('Ctrl Pts',(0.0757563802368799,0.0594682291272118,
-0.493423454950491));
#43490=CARTESIAN_POINT('Ctrl Pts',(-0.00884875264671714,0.0959020281262003,
-0.487074564605844));
#43491=CARTESIAN_POINT('Ctrl Pts',(-0.0853588335365077,0.0446023425327426,
-0.4807256742612));
#43492=CARTESIAN_POINT('Ctrl Pts',(-0.0837805981182255,-0.0475006400069908,
-0.474376783916553));
#43493=CARTESIAN_POINT('Ctrl Pts',(-0.0055578541554653,-0.0961488932817632,
-0.468027893571909));
#43494=CARTESIAN_POINT('Ctrl Pts',(0.0777493486184669,-0.0568378237754173,
-0.461679003227264));
#43495=CARTESIAN_POINT('Ctrl Pts',(0.0899295751191266,0.0344698555409609,
-0.455330112882618));
#43496=CARTESIAN_POINT('Ctrl Pts',(0.019840060851252,0.0942436809952789,
-0.448981222537974));
#43497=CARTESIAN_POINT('Ctrl Pts',(-0.0683996188199645,0.0678011177445095,
-0.442632332193327));
#43498=CARTESIAN_POINT('Ctrl Pts',(-0.0940656801733943,-0.0206675406286791,
-0.436283441848683));
#43499=CARTESIAN_POINT('Ctrl Pts',(-0.0336781922597468,-0.0902290351729243,
-0.429934551504037));
#43500=CARTESIAN_POINT('Ctrl Pts',(0.0575189168835339,-0.0772468356806051,
-0.423585661159392));
#43501=CARTESIAN_POINT('Ctrl Pts',(0.0960963358411698,0.00640262914922511,
-0.417236770814747));
#43502=CARTESIAN_POINT('Ctrl Pts',(0.0467625128298921,0.0841948146619225,
-0.410887880470101));
#43503=CARTESIAN_POINT('Ctrl Pts',(-0.0453507829310814,0.084963556361885,
-0.404538990125456));
#43504=CARTESIAN_POINT('Ctrl Pts',(-0.0959760904473898,0.00800559083115412,
-0.398190099780811));
#43505=CARTESIAN_POINT('Ctrl Pts',(-0.0588001593764506,-0.0762760819616825,
-0.391841209436166));
#43506=CARTESIAN_POINT('Ctrl Pts',(0.0321675733641939,-0.0907785582942382,
-0.38549231909152));
#43507=CARTESIAN_POINT('Ctrl Pts',(0.0937076354156433,-0.0222346236066698,
-0.379143428746875));
#43508=CARTESIAN_POINT('Ctrl Pts',(0.0695216961659067,0.0666500801525155,
-0.37279453840223));
#43509=CARTESIAN_POINT('Ctrl Pts',(-0.0182643647766261,0.0945616856947227,
-0.366445648057585));
#43510=CARTESIAN_POINT('Ctrl Pts',(-0.0893417450266884,0.0359659841754329,
-0.360096757712939));
#43511=CARTESIAN_POINT('Ctrl Pts',(-0.078687145631372,-0.0555322657066021,
-0.353747867368294));
#43512=CARTESIAN_POINT('Ctrl Pts',(0.00395234932620661,-0.0962282617370018,
-0.347398977023649));
#43513=CARTESIAN_POINT('Ctrl Pts',(0.0829761399499992,-0.0488923268122867,
-0.341050086679003));
#43514=CARTESIAN_POINT('Ctrl Pts',(0.0860913597324722,0.0431714859778473,
-0.334701196334359));
#43515=CARTESIAN_POINT('Ctrl Pts',(0.0104481306040173,0.0957409838522809,
-0.328352305989713));
#43516=CARTESIAN_POINT('Ctrl Pts',(-0.0747532999856318,0.0607243243138976,
-0.322003415645068));
#43517=CARTESIAN_POINT('Ctrl Pts',(-0.0915686117343578,-0.0298444093116925,
-0.315654525300423));
#43518=CARTESIAN_POINT('Ctrl Pts',(-0.0246147525519286,-0.0931107586636937,
-0.309305634955777));
#43519=CARTESIAN_POINT('Ctrl Pts',(0.0648572749732974,-0.0711971439396228,
-0.302956744611133));
#43520=CARTESIAN_POINT('Ctrl Pts',(0.0949963056291566,0.0158493324444051,
-0.296607854266486));
#43521=CARTESIAN_POINT('Ctrl Pts',(0.0382304284421113,0.088396457865991,
-0.290258963921842));
#43522=CARTESIAN_POINT('Ctrl Pts',(-0.053509565249277,0.0800763750987432,
-0.283910073577196));
#43523=CARTESIAN_POINT('Ctrl Pts',(-0.0962977201727911,-0.00149950379931796,
-0.277561183232552));
#43524=CARTESIAN_POINT('Ctrl Pts',(-0.0509904018916127,-0.0817036005146229,
-0.271212292887905));
#43525=CARTESIAN_POINT('Ctrl Pts',(0.040964163857924,-0.0871632761060666,
-0.264863402543261));
#43526=CARTESIAN_POINT('Ctrl Pts',(0.0954437261180456,-0.0128838878769242,
-0.258514512198614));
#43527=CARTESIAN_POINT('Ctrl Pts',(0.0626090694984084,0.073181991218226,
-0.25216562185397));
#43528=CARTESIAN_POINT('Ctrl Pts',(-0.0275018714867341,0.0922992225690327,
-0.245816731509324));
#43529=CARTESIAN_POINT('Ctrl Pts',(-0.09245343820747,0.0269789026044658,
-0.239467841164679));
#43530=CARTESIAN_POINT('Ctrl Pts',(-0.0728263734333226,-0.0630223670982701,
-0.233118950820034));
#43531=CARTESIAN_POINT('Ctrl Pts',(0.0134240113723944,-0.0953692578391558,
-0.226770060475389));
#43532=CARTESIAN_POINT('Ctrl Pts',(0.0873937873327554,-0.040470055075016,
-0.220421170130743));
#43533=CARTESIAN_POINT('Ctrl Pts',(0.0814136222514969,0.0514521285661883,
-0.214072279786098));
#43534=CARTESIAN_POINT('Ctrl Pts',(0.00095431514453144,0.0963046660588629,
-0.207723389441453));
#43535=CARTESIAN_POINT('Ctrl Pts',(-0.080378022437017,0.0530553760833366,
-0.201374499096808));
#43536=CARTESIAN_POINT('Ctrl Pts',(-0.0881786096372469,-0.0387302494750746,
-0.195025608752162));
#43537=CARTESIAN_POINT('Ctrl Pts',(-0.0153112814576817,-0.0950845102116404,
-0.188676718407517));
#43538=CARTESIAN_POINT('Ctrl Pts',(0.0715631756928054,-0.0644531714315326,
-0.182327828062872));
#43539=CARTESIAN_POINT('Ctrl Pts',(0.0929699165082818,0.0251414805715377,
-0.175978937718227));
#43540=CARTESIAN_POINT('Ctrl Pts',(0.0293255390683039,0.0917361007482732,
-0.169630047373581));
#43541=CARTESIAN_POINT('Ctrl Pts',(-0.0611465477008044,0.07440832702589,
-0.163281157028936));
#43542=CARTESIAN_POINT('Ctrl Pts',(-0.0956803001699257,-0.0109899759955527,
-0.156932266684291));
#43543=CARTESIAN_POINT('Ctrl Pts',(-0.0426834102937165,-0.0863343842903646,
-0.150583376339646));
#43544=CARTESIAN_POINT('Ctrl Pts',(0.0493612914391104,-0.0826980190591283,
-0.144234485995));
#43545=CARTESIAN_POINT('Ctrl Pts',(0.0962490945489212,-0.00340751448045925,
-0.137885595650355));
#43546=CARTESIAN_POINT('Ctrl Pts',(0.0550859095302308,0.079000266027756,
-0.13153670530571));
#43547=CARTESIAN_POINT('Ctrl Pts',(-0.0364711942086585,0.0891367015934007,
-0.125187814961065));
#43548=CARTESIAN_POINT('Ctrl Pts',(-0.0946635670202091,0.0177287348598427,
-0.118838924616419));
#43549=CARTESIAN_POINT('Ctrl Pts',(-0.0662554373619121,-0.069897902909749,
-0.112490034271774));
#43550=CARTESIAN_POINT('Ctrl Pts',(0.0227647771129189,-0.0935802607606224,
-0.106141143927129));
#43551=CARTESIAN_POINT('Ctrl Pts',(0.0909591962535613,-0.0316531336799535,
-0.0997922535824833));
#43552=CARTESIAN_POINT('Ctrl Pts',(0.0759420075516381,0.0592310251496444,
-0.0934433632378381));
#43553=CARTESIAN_POINT('Ctrl Pts',(-0.00854886285930021,0.0959292484132404,
-0.0870944728931927));
#43554=CARTESIAN_POINT('Ctrl Pts',(-0.0852188293617118,0.0448690236940463,
-0.0807455825485475));
#43555=CARTESIAN_POINT('Ctrl Pts',(-0.0839289348648598,-0.0472383474586548,
-0.0743966922039022));
#43556=CARTESIAN_POINT('Ctrl Pts',(-0.00585811645465809,-0.096131162521779,
-0.068047801859257));
#43557=CARTESIAN_POINT('Ctrl Pts',(0.0775704950346791,-0.0570804549773756,
-0.0616989115146119));
#43558=CARTESIAN_POINT('Ctrl Pts',(0.0900383157362904,0.0341880300064409,
-0.0553500211699665));
#43559=CARTESIAN_POINT('Ctrl Pts',(0.0201320506167284,0.0941819939552226,
-0.0490011308253214));
#43560=CARTESIAN_POINT('Ctrl Pts',(-0.0681822691654502,0.0680131341533761,
-0.042652240480676));
#43561=CARTESIAN_POINT('Ctrl Pts',(-0.0941393148464921,-0.0203703384015287,
-0.0363033501360307));
#43562=CARTESIAN_POINT('Ctrl Pts',(-0.0339422270357189,-0.0901288607981892,
-0.0299544597913855));
#43563=CARTESIAN_POINT('Ctrl Pts',(0.0572428774412662,-0.0774156769940841,
-0.0236055694467402));
#43564=CARTESIAN_POINT('Ctrl Pts',(0.0961817888891786,0.00608136681561371,
-0.0172566791020948));
#43565=CARTESIAN_POINT('Ctrl Pts',(0.0468917811787354,0.0840917490061967,
-0.0109077887574496));
#43566=CARTESIAN_POINT('Ctrl Pts',(-0.0142098698468084,0.0846926301986895,
-0.00667519519435273));
#43567=CARTESIAN_POINT('Ctrl Pts',(-0.0381483114577586,0.0720110968464789,
-0.00455889841280429));
#43568=CARTESIAN_POINT('Ctrl Pts',(-0.0601104350279426,-0.0429877377952305,
-1.149325));
#43569=CARTESIAN_POINT('Ctrl Pts',(-0.0458201451106566,-0.0629700766588213,
-1.14720870321845));
#43570=CARTESIAN_POINT('Ctrl Pts',(0.00400364749018219,-0.0872208216030551,
-1.14297610965536));
#43571=CARTESIAN_POINT('Ctrl Pts',(0.075583875527885,-0.0438759620050528,
-1.13662721931071));
#43572=CARTESIAN_POINT('Ctrl Pts',(0.0777927499997916,0.0396423987382078,
-1.13027832896607));
#43573=CARTESIAN_POINT('Ctrl Pts',(0.00894843417834478,0.0868766870214709,
-1.12392943862142));
#43574=CARTESIAN_POINT('Ctrl Pts',(-0.0681413246659313,0.0546437095181167,
-1.11758054827678));
#43575=CARTESIAN_POINT('Ctrl Pts',(-0.0828626209147509,-0.0275837207699589,
-1.11123165793213));
#43576=CARTESIAN_POINT('Ctrl Pts',(-0.0217956051609413,-0.0845742251201784,
-1.10488276758748));
#43577=CARTESIAN_POINT('Ctrl Pts',(0.0592192057513427,-0.0641956017183869,
-1.09853387724284));
#43578=CARTESIAN_POINT('Ctrl Pts',(0.0860543001947688,0.0149114473055614,
-1.09218498689819));
#43579=CARTESIAN_POINT('Ctrl Pts',(0.0341672535616166,0.0803767533194929,
-1.08583609655355));
#43580=CARTESIAN_POINT('Ctrl Pts',(-0.0489780873575578,0.0723116766374376,
-1.0794872062089));
#43581=CARTESIAN_POINT('Ctrl Pts',(-0.0873164260293921,-0.00190597202016384,
-1.07313831586426));
#43582=CARTESIAN_POINT('Ctrl Pts',(-0.0457759481553394,-0.074379934125127,
-1.06678942551961));
#43583=CARTESIAN_POINT('Ctrl Pts',(0.037641655214997,-0.0788093717621258,
-1.06044053517497));
#43584=CARTESIAN_POINT('Ctrl Pts',(0.0866236680057719,-0.0111420824567537,
-1.05409164483032));
#43585=CARTESIAN_POINT('Ctrl Pts',(0.0563603151316931,0.0667182437528911,
-1.04774275448568));
#43586=CARTESIAN_POINT('Ctrl Pts',(-0.0254628383918398,0.0835431184830735,
-1.04139386414103));
#43587=CARTESIAN_POINT('Ctrl Pts',(-0.0839919598596433,0.0239407344160811,
-1.03504497379639));
#43588=CARTESIAN_POINT('Ctrl Pts',(-0.0656832215466922,-0.0575632087386073,
-1.02869608345174));
#43589=CARTESIAN_POINT('Ctrl Pts',(0.0127141134428745,-0.0864069431030045,
-1.0223471931071));
#43590=CARTESIAN_POINT('Ctrl Pts',(0.0794802692010834,-0.0362035249468621,
-1.01599830276245));
#43591=CARTESIAN_POINT('Ctrl Pts',(0.0735359619677752,0.0471197494086118,
-1.0096494124178));
#43592=CARTESIAN_POINT('Ctrl Pts',(0.000319185439644519,0.0873367424855461,
-1.00330052207316));
#43593=CARTESIAN_POINT('Ctrl Pts',(-0.0731895893058077,0.0476559804706753,
-0.996951631728512));
#43594=CARTESIAN_POINT('Ctrl Pts',(-0.0797427655561862,-0.0356216199793146,
-0.990602741383869));
#43595=CARTESIAN_POINT('Ctrl Pts',(-0.0133453396325877,-0.0863117047392357,
-0.984253851039223));
#43596=CARTESIAN_POINT('Ctrl Pts',(0.0652607242893321,-0.0580417636628946,
-0.977904960694579));
#43597=CARTESIAN_POINT('Ctrl Pts',(0.0841647062166166,0.0233261804187959,
-0.971556070349931));
#43598=CARTESIAN_POINT('Ctrl Pts',(0.0260727882493475,0.0833547729751633,
-0.965207180005289));
#43599=CARTESIAN_POINT('Ctrl Pts',(-0.0558711442187008,0.0671284120804557,
-0.958858289660641));
#43600=CARTESIAN_POINT('Ctrl Pts',(-0.0867028086157542,-0.0105086365962801,
-0.952509399315998));
#43601=CARTESIAN_POINT('Ctrl Pts',(-0.0382166559382933,-0.0785321314734518,
-0.946160508971351));
#43602=CARTESIAN_POINT('Ctrl Pts',(0.0452310138244137,-0.0747125414725162,
-0.939811618626707));
#43603=CARTESIAN_POINT('Ctrl Pts',(0.087300263005714,-0.00254411949997818,
-0.933462728282061));
#43604=CARTESIAN_POINT('Ctrl Pts',(0.0495051294517987,0.0719517242520363,
-0.927113837937416));
#43605=CARTESIAN_POINT('Ctrl Pts',(-0.0335784885779334,0.0806243981044391,
-0.920764947592771));
#43606=CARTESIAN_POINT('Ctrl Pts',(-0.0859436967070338,0.0155399311843679,
-0.914416057248125));
#43607=CARTESIAN_POINT('Ctrl Pts',(-0.0596855416164745,-0.0637608389752754,
-0.908067166903481));
#43608=CARTESIAN_POINT('Ctrl Pts',(0.0211743841364114,-0.0847316583180511,
-0.901718276558834));
#43609=CARTESIAN_POINT('Ctrl Pts',(0.0826634734150078,-0.0281879163445984,
-0.89536938621419));
#43610=CARTESIAN_POINT('Ctrl Pts',(0.0685300267273087,0.0541428102488016,
-0.889020495869544));
#43611=CARTESIAN_POINT('Ctrl Pts',(-0.00829633857195642,0.0869423903006062,
-0.882671605524899));
#43612=CARTESIAN_POINT('Ctrl Pts',(-0.0775330135748029,0.0402049781854557,
-0.876322715180253));
#43613=CARTESIAN_POINT('Ctrl Pts',(-0.0758406208115356,-0.043312916085209,
-0.86997382483561));
#43614=CARTESIAN_POINT('Ctrl Pts',(-0.00476740193378281,-0.087207111772408,
-0.863624934490961));
#43615=CARTESIAN_POINT('Ctrl Pts',(0.0706671510291381,-0.0513221417159152,
-0.857276044146319));
#43616=CARTESIAN_POINT('Ctrl Pts',(0.0814536926085207,0.0315135593883026,
-0.850927153801671));
#43617=CARTESIAN_POINT('Ctrl Pts',(0.0177244348341756,0.0855198975367287,
-0.844578263457028));
#43618=CARTESIAN_POINT('Ctrl Pts',(-0.0622195627201011,0.0612905741513564,
-0.838229373112381));
#43619=CARTESIAN_POINT('Ctrl Pts',(-0.0852436060887428,-0.0190088423074822,
-0.831880482767737));
#43620=CARTESIAN_POINT('Ctrl Pts',(-0.0302847459931343,-0.081918512102057,
-0.825531592423091));
#43621=CARTESIAN_POINT('Ctrl Pts',(0.0523793289752858,-0.0698871544776452,
-0.819182702078447));
#43622=CARTESIAN_POINT('Ctrl Pts',(0.0871255325346814,0.00607865490315511,
-0.812833811733801));
#43623=CARTESIAN_POINT('Ctrl Pts',(0.0421672010014363,0.0764835644082308,
-0.806484921389155));
#43624=CARTESIAN_POINT('Ctrl Pts',(-0.041366701368516,0.0769194675148722,
-0.800136031044511));
#43625=CARTESIAN_POINT('Ctrl Pts',(-0.0870573492415018,0.0069875895648422,
-0.793787140699864));
#43626=CARTESIAN_POINT('Ctrl Pts',(-0.0531058377402594,-0.0693367035760193,
-0.787438250355221));
#43627=CARTESIAN_POINT('Ctrl Pts',(0.0294281728820954,-0.0822301106998219,
-0.781089360010573));
#43628=CARTESIAN_POINT('Ctrl Pts',(0.0850405823393773,-0.0198974325042983,
-0.77474046966593));
#43629=CARTESIAN_POINT('Ctrl Pts',(0.0628558193470167,0.0606378960642491,
-0.768391579321283));
#43630=CARTESIAN_POINT('Ctrl Pts',(-0.0168309607139535,0.0857002171895078,
-0.762042688976639));
#43631=CARTESIAN_POINT('Ctrl Pts',(-0.0811203726344865,0.0323619160206188,
-0.755693798631993));
#43632=CARTESIAN_POINT('Ctrl Pts',(-0.0711989143396801,-0.0505818451792178,
-0.749344908287349));
#43633=CARTESIAN_POINT('Ctrl Pts',(0.00385702521968538,-0.0872521164289911,
-0.742996017942701));
#43634=CARTESIAN_POINT('Ctrl Pts',(0.0753844652332581,-0.0441020505915453,
-0.736647127598059));
#43635=CARTESIAN_POINT('Ctrl Pts',(0.0779483812393019,0.0393936330776424,
-0.730298237253411));
#43636=CARTESIAN_POINT('Ctrl Pts',(0.00920324113794826,0.086851072632641,
-0.723949346908768));
#43637=CARTESIAN_POINT('Ctrl Pts',(-0.0679612455648586,0.0548550596222128,
-0.717600456564122));
#43638=CARTESIAN_POINT('Ctrl Pts',(-0.0829531483594101,-0.0273236828071396,
-0.711251566219477));
#43639=CARTESIAN_POINT('Ctrl Pts',(-0.0220575135733365,-0.0845060622668312,
-0.704902675874831));
#43640=CARTESIAN_POINT('Ctrl Pts',(0.0590168657611575,-0.064380261110165,
-0.698553785530186));
#43641=CARTESIAN_POINT('Ctrl Pts',(0.0861011952070565,0.0146421531476717,
-0.692204895185541));
#43642=CARTESIAN_POINT('Ctrl Pts',(0.0344180780130461,0.080269573131862,
-0.685856004840895));
#43643=CARTESIAN_POINT('Ctrl Pts',(-0.0487515257137156,0.0724644547724496,
-0.679507114496251));
#43644=CARTESIAN_POINT('Ctrl Pts',(-0.0873220598104371,-0.00163289171286479,
-0.673158224151604));
#43645=CARTESIAN_POINT('Ctrl Pts',(-0.0460082709303986,-0.0742364295402099,
-0.66680933380696));
#43646=CARTESIAN_POINT('Ctrl Pts',(0.037394992047993,-0.0789266940560291,
-0.660460443462315));
#43647=CARTESIAN_POINT('Ctrl Pts',(0.0865884158521809,-0.0114129183425305,
-0.654111553117668));
#43648=CARTESIAN_POINT('Ctrl Pts',(0.0565686718383231,0.0665416698868583,
-0.647762662773025));
#43649=CARTESIAN_POINT('Ctrl Pts',(-0.0252014553124982,0.0836223362207471,
-0.641413772428377));
#43650=CARTESIAN_POINT('Ctrl Pts',(-0.0839166843077061,0.0242032758048216,
-0.635064882083734));
#43651=CARTESIAN_POINT('Ctrl Pts',(-0.0658629098354269,-0.0573575241175375,
-0.628715991739088));
#43652=CARTESIAN_POINT('Ctrl Pts',(0.0124438404931729,-0.0864462798428249,
-0.622367101394442));
#43653=CARTESIAN_POINT('Ctrl Pts',(0.0793666658984961,-0.0364518971939734,
-0.616018211049798));
#43654=CARTESIAN_POINT('Ctrl Pts',(0.073682954238757,0.0468895587474729,
-0.609669320705152));
#43655=CARTESIAN_POINT('Ctrl Pts',(0.000592301800611145,0.087335317274631,
-0.603320430360507));
#43656=CARTESIAN_POINT('Ctrl Pts',(-0.0730402025870019,0.0478846245775535,
-0.596971540015862));
#43657=CARTESIAN_POINT('Ctrl Pts',(-0.0798537708843025,-0.0353720757157512,
-0.590622649671216));
#43658=CARTESIAN_POINT('Ctrl Pts',(-0.0136151867463331,-0.0862695494061835,
-0.584273759326571));
#43659=CARTESIAN_POINT('Ctrl Pts',(0.06507889807261,-0.058245561981479,
-0.577924868981926));
#43660=CARTESIAN_POINT('Ctrl Pts',(0.0842372398743852,0.0230628680616442,
-0.57157597863728));
#43661=CARTESIAN_POINT('Ctrl Pts',(0.0263333262574912,0.083272831062118,
-0.565227088292636));
#43662=CARTESIAN_POINT('Ctrl Pts',(-0.0556609483102603,0.0673028030477632,
-0.55887819794799));
#43663=CARTESIAN_POINT('Ctrl Pts',(-0.0867352470819517,-0.010237449805311,
-0.552529307603345));
#43664=CARTESIAN_POINT('Ctrl Pts',(-0.0384620532909962,-0.0784122370649128,
-0.5461804172587));
#43665=CARTESIAN_POINT('Ctrl Pts',(0.0449971529934493,-0.0748536217384812,
-0.539831526914054));
#43666=CARTESIAN_POINT('Ctrl Pts',(0.0872918802153685,-0.00281711081593204,
-0.533482636569409));
#43667=CARTESIAN_POINT('Ctrl Pts',(0.0497298934808031,0.0717965609153495,
-0.527133746224764));
#43668=CARTESIAN_POINT('Ctrl Pts',(-0.0333261972756367,0.0807290099036824,
-0.520784855880119));
#43669=CARTESIAN_POINT('Ctrl Pts',(-0.0858946802897314,0.0158086167265926,
-0.514435965535473));
#43670=CARTESIAN_POINT('Ctrl Pts',(-0.0598846414830402,-0.0635738796938743,
-0.508087075190828));
#43671=CARTESIAN_POINT('Ctrl Pts',(0.0209093093381367,-0.0847974601499693,
-0.501738184846182));
#43672=CARTESIAN_POINT('Ctrl Pts',(0.0825749204933152,-0.0284462821895266,
-0.495389294501537));
#43673=CARTESIAN_POINT('Ctrl Pts',(0.0686990060272686,0.0539282396870952,
-0.489040404156892));
#43674=CARTESIAN_POINT('Ctrl Pts',(-0.00802441338286892,0.0869679093386998,
-0.482691513812247));
#43675=CARTESIAN_POINT('Ctrl Pts',(-0.0774069062073571,0.0404472413928185,
-0.476342623467602));
#43676=CARTESIAN_POINT('Ctrl Pts',(-0.0759756973220605,-0.0430755369242237,
-0.469993733122956));
#43677=CARTESIAN_POINT('Ctrl Pts',(-0.0050400910778892,-0.0871917768302152,
-0.463644842778311));
#43678=CARTESIAN_POINT('Ctrl Pts',(0.070506311846667,-0.0515428797668893,
-0.457295952433666));
#43679=CARTESIAN_POINT('Ctrl Pts',(0.0815518429447203,0.0312586848284312,
-0.45094706208902));
#43680=CARTESIAN_POINT('Ctrl Pts',(0.0179917843980893,0.0854640518525547,
-0.444598171744375));
#43681=CARTESIAN_POINT('Ctrl Pts',(-0.0620275917471557,0.0614848463194927,
-0.43824928139973));
#43682=CARTESIAN_POINT('Ctrl Pts',(-0.0853026333753618,-0.0187421771444026,
-0.431900391055085));
#43683=CARTESIAN_POINT('Ctrl Pts',(-0.0305407719561762,-0.0818234056563543,
-0.425551500710439));
#43684=CARTESIAN_POINT('Ctrl Pts',(0.0521605230517608,-0.0700506124159539,
-0.419202610365794));
#43685=CARTESIAN_POINT('Ctrl Pts',(0.0871441155782282,0.00580616783876835,
-0.412853720021149));
#43686=CARTESIAN_POINT('Ctrl Pts',(0.0424061727963488,0.0763513259455898,
-0.406504829676504));
#43687=CARTESIAN_POINT('Ctrl Pts',(-0.0411259579745188,0.0770484525838227,
-0.400155939331858));
#43688=CARTESIAN_POINT('Ctrl Pts',(-0.0870350721022039,0.00725979951842593,
-0.393807048987213));
#43689=CARTESIAN_POINT('Ctrl Pts',(-0.0533224065191096,-0.0691702929579908,
-0.387458158642567));
#43690=CARTESIAN_POINT('Ctrl Pts',(0.0291708805188321,-0.082321735857788,
-0.381109268297923));
#43691=CARTESIAN_POINT('Ctrl Pts',(0.0849779436410596,-0.0201632725374741,
-0.374760377953277));
#43692=CARTESIAN_POINT('Ctrl Pts',(0.0630451377031669,0.0604410380194803,
-0.368411487608632));
#43693=CARTESIAN_POINT('Ctrl Pts',(-0.0165628782942129,0.0857524316127216,
-0.362062597263987));
#43694=CARTESIAN_POINT('Ctrl Pts',(-0.0810187744039951,0.0326154359001687,
-0.355713706919342));
#43695=CARTESIAN_POINT('Ctrl Pts',(-0.0713567448061166,-0.0503589459337495,
-0.349364816574696));
#43696=CARTESIAN_POINT('Ctrl Pts',(0.00358415316748011,-0.0872637514146367,
-0.343015926230051));
#43697=CARTESIAN_POINT('Ctrl Pts',(0.0752461815192336,-0.0443375758432733,
-0.336667035885405));
#43698=CARTESIAN_POINT('Ctrl Pts',(0.0780711911348368,0.0391496817314182,
-0.330318145540761));
#43699=CARTESIAN_POINT('Ctrl Pts',(0.00947479519341831,0.0868218677576465,
-0.323969255196115));
#43700=CARTESIAN_POINT('Ctrl Pts',(-0.0677893715382528,0.0550673185413288,
-0.31762036485147));
#43701=CARTESIAN_POINT('Ctrl Pts',(-0.0830381888598311,-0.0270641396641863,
-0.311271474506825));
#43702=CARTESIAN_POINT('Ctrl Pts',(-0.0223216715032739,-0.0844366712168558,
-0.304922584162179));
#43703=CARTESIAN_POINT('Ctrl Pts',(0.0588152484367718,-0.0645645027565787,
-0.298573693817534));
#43704=CARTESIAN_POINT('Ctrl Pts',(0.0861465628713941,0.0143728274994348,
-0.292224803472889));
#43705=CARTESIAN_POINT('Ctrl Pts',(0.0346689272343444,0.0801615490700074,
-0.285875913128243));
#43706=CARTESIAN_POINT('Ctrl Pts',(-0.0485246778433969,0.0726165553099154,
-0.279527022783598));
#43707=CARTESIAN_POINT('Ctrl Pts',(-0.0873267391852247,-0.00135981181024029,
-0.273178132438953));
#43708=CARTESIAN_POINT('Ctrl Pts',(-0.04624019674556,-0.074092190342946,
-0.266829242094308));
#43709=CARTESIAN_POINT('Ctrl Pts',(0.0371479911127987,-0.0790432490549754,
-0.260480351749662));
#43710=CARTESIAN_POINT('Ctrl Pts',(0.0865523022001051,-0.0116836402180771,
-0.254131461405018));
#43711=CARTESIAN_POINT('Ctrl Pts',(0.0567764831078735,0.0663644440252806,
-0.247782571060372));
#43712=CARTESIAN_POINT('Ctrl Pts',(-0.0249398298746646,0.083700736858798,
-0.241433680715727));
#43713=CARTESIAN_POINT('Ctrl Pts',(-0.0838405859519216,0.0244655801509781,
-0.235084790371081));
#43714=CARTESIAN_POINT('Ctrl Pts',(-0.0660419551699266,-0.0571512783952807,
-0.228735900026436));
#43715=CARTESIAN_POINT('Ctrl Pts',(0.0121734464516189,-0.0864847712974369,
-0.222387009681791));
#43716=CARTESIAN_POINT('Ctrl Pts',(0.0792522861301636,-0.0366999129159682,
-0.216038119337145));
#43717=CARTESIAN_POINT('Ctrl Pts',(0.0738292261096514,0.046658909512726,
-0.2096892289925));
#43718=CARTESIAN_POINT('Ctrl Pts',(0.000865412281594935,0.0873330380008177,
-0.203340338647855));
#43719=CARTESIAN_POINT('Ctrl Pts',(-0.0728901015412066,0.0481128003995335,
-0.19699144830321));
#43720=CARTESIAN_POINT('Ctrl Pts',(-0.0799639953229482,-0.0351221855348143,
-0.190642557958564));
#43721=CARTESIAN_POINT('Ctrl Pts',(-0.0138849007021918,-0.0862265504199637,
-0.184293667613919));
#43722=CARTESIAN_POINT('Ctrl Pts',(0.0648964354273228,-0.058448790699953,
-0.177944777269274));
#43723=CARTESIAN_POINT('Ctrl Pts',(0.0843089497489975,0.0227993301675411,
-0.171595886924629));
#43724=CARTESIAN_POINT('Ctrl Pts',(0.0265936067550599,0.0831900747965725,
-0.165246996579983));
#43725=CARTESIAN_POINT('Ctrl Pts',(-0.0554502081000843,0.0674765358488189,
-0.158898106235338));
#43726=CARTESIAN_POINT('Ctrl Pts',(-0.0867668372949077,-0.00996616291323742,
-0.152549215890693));
#43727=CARTESIAN_POINT('Ctrl Pts',(-0.0387070745970641,-0.0782915758141884,
-0.146200325546048));
#43728=CARTESIAN_POINT('Ctrl Pts',(0.0447628522836712,-0.0749939700395087,
-0.139851435201402));
#43729=CARTESIAN_POINT('Ctrl Pts',(0.087282643466595,-0.00309007448744508,
-0.133502544856757));
#43730=CARTESIAN_POINT('Ctrl Pts',(0.0499541717674709,0.071640695279081,
-0.127153654512112));
#43731=CARTESIAN_POINT('Ctrl Pts',(-0.0330735811680512,0.0808328325728891,
-0.120804764167467));
#43732=CARTESIAN_POINT('Ctrl Pts',(-0.085844821795195,0.0160771470229162,
-0.114455873822821));
#43733=CARTESIAN_POINT('Ctrl Pts',(-0.0600831596815059,-0.0633862974745522,
-0.108106983478176));
#43734=CARTESIAN_POINT('Ctrl Pts',(0.0206440375741234,-0.0848624350572862,
-0.101758093133531));
#43735=CARTESIAN_POINT('Ctrl Pts',(0.082485545799834,-0.0287043654232375,
-0.0954092027888854));
#43736=CARTESIAN_POINT('Ctrl Pts',(0.0688673405223371,0.0537131333497329,
-0.0890603124442403));
#43737=CARTESIAN_POINT('Ctrl Pts',(-0.00775246097108719,0.0869925938161997,
-0.0827114220995948));
#43738=CARTESIAN_POINT('Ctrl Pts',(-0.0772799446548373,0.0406890788545673,
-0.0763625317549497));
#43739=CARTESIAN_POINT('Ctrl Pts',(-0.0761102151939444,-0.0428376792374824,
-0.0700136414103042));
#43740=CARTESIAN_POINT('Ctrl Pts',(-0.00531238129869321,-0.0871756978467261,
-0.0636647510656592));
#43741=CARTESIAN_POINT('Ctrl Pts',(0.0703441200498545,-0.0517629077348786,
-0.057315860721014));
#43742=CARTESIAN_POINT('Ctrl Pts',(0.0816504534154235,0.0310031138252487,
-0.0509669703763687));
#43743=CARTESIAN_POINT('Ctrl Pts',(0.018256572744571,0.0854081115037233,
-0.0446180800317234));
#43744=CARTESIAN_POINT('Ctrl Pts',(-0.0618304901277434,0.0616771115320737,
-0.0382691896870782));
#43745=CARTESIAN_POINT('Ctrl Pts',(-0.0853694083299616,-0.0184726619229722,
-0.0319202993424328));
#43746=CARTESIAN_POINT('Ctrl Pts',(-0.0307802095667008,-0.0817325634071313,
-0.0255714089977876));
#43747=CARTESIAN_POINT('Ctrl Pts',(0.0519101991153633,-0.070203724673642,
-0.0192225186531423));
#43748=CARTESIAN_POINT('Ctrl Pts',(0.087221607922,0.0055148339217558,-0.012873628308497));
#43749=CARTESIAN_POINT('Ctrl Pts',(0.0425233986596825,0.0762578617636718,
-0.00652473796385174));
#43750=CARTESIAN_POINT('Ctrl Pts',(-0.0128860952859686,0.0768027655795051,
-0.00229214440075486));
#43751=CARTESIAN_POINT('Ctrl Pts',(-0.0345944601705076,0.0653026287794846,
-0.000175847619206415));
#43752=CARTESIAN_POINT('Ctrl Pts',(-0.0452560140322605,0.0854280329804675,
-0.013325));
#43753=CARTESIAN_POINT('Ctrl Pts',(-0.0168574189684875,0.100472359437059,
-0.0154412967815485));
#43754=CARTESIAN_POINT('Ctrl Pts',(0.0193855636241788,0.100115941464152,
-0.0175575935630971));
#43755=CARTESIAN_POINT('Ctrl Pts',(0.0472526556882942,0.084513550663045,
-0.0196738903446456));
#43756=CARTESIAN_POINT('Ctrl Pts',(0.0751197477524064,0.0689111598619393,
-0.0217901871261938));
#43757=CARTESIAN_POINT('Ctrl Pts',(0.0946109492879698,0.0380627962326364,
-0.0239064839077421));
#43758=CARTESIAN_POINT('Ctrl Pts',(0.0966575639340093,0.0061296120449364,
-0.0260227806892903));
#43759=CARTESIAN_POINT('Ctrl Pts',(0.0987041785800492,-0.0258035721427672,
-0.0281390774708388));
#43760=CARTESIAN_POINT('Ctrl Pts',(0.0833062063365607,-0.0588215768888681,
-0.0302553742523873));
#43761=CARTESIAN_POINT('Ctrl Pts',(0.0575781375370112,-0.0778442249194746,
-0.0323716710339359));
#43762=CARTESIAN_POINT('Ctrl Pts',(0.0318500687374624,-0.0968668729500805,
-0.0344879678154843));
#43763=CARTESIAN_POINT('Ctrl Pts',(-0.00420809661814683,-0.101894164265193,
-0.0366042645970328));
#43764=CARTESIAN_POINT('Ctrl Pts',(-0.0341393236135845,-0.0906151825524714,
-0.0387205613785813));
#43765=CARTESIAN_POINT('Ctrl Pts',(-0.0640705506090213,-0.0793362008397503,
-0.0408368581601297));
#43766=CARTESIAN_POINT('Ctrl Pts',(-0.0878748392442869,-0.0517509460991965,
-0.042953154941678));
#43767=CARTESIAN_POINT('Ctrl Pts',(-0.0946447667888051,-0.0204831736031495,
-0.0450694517232264));
#43768=CARTESIAN_POINT('Ctrl Pts',(-0.0960917122047474,-0.0138002719350931,
-0.0455217705858284));
#43769=CARTESIAN_POINT('Ctrl Pts',(-0.0967605098021332,-0.00694914892060837,
-0.0459740894484305));
#43770=CARTESIAN_POINT('Ctrl Pts',(-0.0966970977580488,-8.58596968723868E-5,
-0.0464264083110326));
#43771=CARTESIAN_POINT('Origin',(0.194007127343405,-0.0342086910003853,
0.04));
#43772=CARTESIAN_POINT('',(0.18738691397118,-0.0314029373205391,0.04));
#43773=CARTESIAN_POINT('',(0.186826537413779,-0.0345809907026646,0.04));
#43774=CARTESIAN_POINT('Origin',(0.,0.,0.04));
#43775=CARTESIAN_POINT('',(0.181204626554246,-0.0319512646907152,0.04));
#43776=CARTESIAN_POINT('',(0.208025165376232,-0.02957246303897,0.04));
#43777=CARTESIAN_POINT('',(0.181204626554246,-0.0319512646907152,0.04));
#43778=CARTESIAN_POINT('Origin',(0.181204626554246,-0.0319512646907152,
0.04));
#43779=CARTESIAN_POINT('',(0.186826537413779,-0.0345809907026646,0.185));
#43780=CARTESIAN_POINT('',(0.186826537413779,-0.0345809907026646,0.0925));
#43781=CARTESIAN_POINT('',(0.181204626554246,-0.0319512646907152,0.191));
#43782=CARTESIAN_POINT('',(0.181204626554246,-0.0319512646907152,0.04));
#43783=CARTESIAN_POINT('Ctrl Pts',(0.186826537413779,-0.0345809907026646,
0.185));
#43784=CARTESIAN_POINT('Ctrl Pts',(0.183970486442383,-0.033245033637782,
0.188051499118437));
#43785=CARTESIAN_POINT('Ctrl Pts',(0.181204626554246,-0.0319512646907152,
0.191));
#43786=CARTESIAN_POINT('Origin',(0.208025165376232,-0.02957246303897,0.04));
#43787=CARTESIAN_POINT('',(0.18738691397118,-0.0314029373205391,0.185));
#43788=CARTESIAN_POINT('',(0.18738691397118,-0.0314029373205391,0.0925));
#43789=CARTESIAN_POINT('Ctrl Pts',(0.181204626554246,-0.0319512646907152,
0.191));
#43790=CARTESIAN_POINT('Ctrl Pts',(0.18424617972193,-0.0316814993535168,
0.188051499118469));
#43791=CARTESIAN_POINT('Ctrl Pts',(0.18738691397118,-0.0314029373205392,
0.185));
#43792=CARTESIAN_POINT('Origin',(0.185119446294824,-0.0673779682351569,
0.04));
#43793=CARTESIAN_POINT('',(0.179087022852749,-0.0634652522703487,0.04));
#43794=CARTESIAN_POINT('',(0.17798329649608,-0.0664977155125527,0.04));
#43795=CARTESIAN_POINT('Origin',(0.,0.,0.04));
#43796=CARTESIAN_POINT('',(0.172903442224607,-0.0629317063719232,0.04));
#43797=CARTESIAN_POINT('',(0.19972959136832,-0.0652463817528892,0.04));
#43798=CARTESIAN_POINT('',(0.172903442224607,-0.0629317063719232,0.04));
#43799=CARTESIAN_POINT('Origin',(0.172903442224607,-0.0629317063719232,
0.04));
#43800=CARTESIAN_POINT('',(0.17798329649608,-0.0664977155125527,0.185));
#43801=CARTESIAN_POINT('',(0.17798329649608,-0.0664977155125527,0.0925));
#43802=CARTESIAN_POINT('',(0.172903442224607,-0.0629317063719232,0.191));
#43803=CARTESIAN_POINT('',(0.172903442224607,-0.0629317063719232,0.04));
#43804=CARTESIAN_POINT('Ctrl Pts',(0.17798329649608,-0.0664977155125527,
0.185));
#43805=CARTESIAN_POINT('Ctrl Pts',(0.17540262186618,-0.0646861065908373,
0.188051499118472));
#43806=CARTESIAN_POINT('Ctrl Pts',(0.172903442224607,-0.0629317063719232,
0.191));
#43807=CARTESIAN_POINT('Origin',(0.19972959136832,-0.0652463817528892,0.04));
#43808=CARTESIAN_POINT('',(0.179087022852749,-0.0634652522703487,0.185));
#43809=CARTESIAN_POINT('',(0.179087022852749,-0.0634652522703487,0.0925));
#43810=CARTESIAN_POINT('Ctrl Pts',(0.172903442224607,-0.0629317063719232,
0.191));
#43811=CARTESIAN_POINT('Ctrl Pts',(0.17594563162456,-0.063194199541203,
0.188051499118452));
#43812=CARTESIAN_POINT('Ctrl Pts',(0.179087022852749,-0.0634652522703487,
0.185));
#43813=CARTESIAN_POINT('Origin',(0.170607004545534,-0.0985000000000001,
0.04));
#43814=CARTESIAN_POINT('',(0.165345663167344,-0.0935992076448907,0.04));
#43815=CARTESIAN_POINT('',(0.163732123178242,-0.0963939408860593,0.04));
#43816=CARTESIAN_POINT('Origin',(0.,0.,0.04));
#43817=CARTESIAN_POINT('',(0.159348674296337,-0.0920000000000001,0.04));
#43818=CARTESIAN_POINT('',(0.185365334794732,-0.098937822173509,0.04));
#43819=CARTESIAN_POINT('',(0.159348674296337,-0.0920000000000001,0.04));
#43820=CARTESIAN_POINT('Origin',(0.159348674296337,-0.0920000000000001,
0.04));
#43821=CARTESIAN_POINT('',(0.163732123178242,-0.0963939408860593,0.185));
#43822=CARTESIAN_POINT('',(0.163732123178242,-0.0963939408860593,0.0925));
#43823=CARTESIAN_POINT('',(0.159348674296337,-0.0920000000000001,0.191));
#43824=CARTESIAN_POINT('',(0.159348674296337,-0.0920000000000001,0.04));
#43825=CARTESIAN_POINT('Ctrl Pts',(0.163732123178242,-0.0963939408860593,
0.185));
#43826=CARTESIAN_POINT('Ctrl Pts',(0.161505237382642,-0.0941617249279212,
0.188051499118436));
#43827=CARTESIAN_POINT('Ctrl Pts',(0.159348674296337,-0.0920000000000001,
0.191));
#43828=CARTESIAN_POINT('Origin',(0.185365334794732,-0.098937822173509,0.04));
#43829=CARTESIAN_POINT('',(0.165345663167344,-0.0935992076448907,0.185));
#43830=CARTESIAN_POINT('',(0.165345663167344,-0.0935992076448907,0.0925));
#43831=CARTESIAN_POINT('Ctrl Pts',(0.159348674296337,-0.0920000000000001,
0.191));
#43832=CARTESIAN_POINT('Ctrl Pts',(0.162299064543036,-0.0927867759536363,
0.188051499118462));
#43833=CARTESIAN_POINT('Ctrl Pts',(0.165345663167344,-0.0935992076448907,
0.185));
#43834=CARTESIAN_POINT('Origin',(0.150910755294439,-0.126629159108248,0.04));
#43835=CARTESIAN_POINT('',(0.146580359175541,-0.120889198458627,0.04));
#43836=CARTESIAN_POINT('',(0.144506032150084,-0.123361285143431,0.04));
#43837=CARTESIAN_POINT('Origin',(0.,0.,0.04));
#43838=CARTESIAN_POINT('',(0.140952177533892,-0.118272920182323,0.04));
#43839=CARTESIAN_POINT('',(0.165368846322791,-0.129623086932341,0.04));
#43840=CARTESIAN_POINT('',(0.140952177533892,-0.118272920182323,0.04));
#43841=CARTESIAN_POINT('Origin',(0.140952177533892,-0.118272920182323,0.04));
#43842=CARTESIAN_POINT('',(0.144506032150084,-0.123361285143431,0.185));
#43843=CARTESIAN_POINT('',(0.144506032150084,-0.123361285143431,0.0925));
#43844=CARTESIAN_POINT('',(0.140952177533892,-0.118272920182323,0.191));
#43845=CARTESIAN_POINT('',(0.140952177533892,-0.118272920182323,0.04));
#43846=CARTESIAN_POINT('Ctrl Pts',(0.144506032150084,-0.123361285143431,
0.185));
#43847=CARTESIAN_POINT('Ctrl Pts',(0.1427005979868,-0.120776286901188,0.188051499118426));
#43848=CARTESIAN_POINT('Ctrl Pts',(0.140952177533892,-0.118272920182323,
0.191));
#43849=CARTESIAN_POINT('Origin',(0.165368846322791,-0.129623086932341,0.04));
#43850=CARTESIAN_POINT('',(0.146580359175541,-0.120889198458627,0.185));
#43851=CARTESIAN_POINT('',(0.146580359175541,-0.120889198458627,0.0925));
#43852=CARTESIAN_POINT('Ctrl Pts',(0.140952177533892,-0.118272920182323,
0.191));
#43853=CARTESIAN_POINT('Ctrl Pts',(0.143721122512686,-0.1195600731311,0.188051499118447));
#43854=CARTESIAN_POINT('Ctrl Pts',(0.146580359175541,-0.120889198458627,
0.185));
#43855=CARTESIAN_POINT('Origin',(0.126629159108248,-0.150910755294439,0.04));
#43856=CARTESIAN_POINT('',(0.123361285143431,-0.144506032150084,0.04));
#43857=CARTESIAN_POINT('',(0.120889198458627,-0.146580359175541,0.04));
#43858=CARTESIAN_POINT('Origin',(0.,0.,0.04));
#43859=CARTESIAN_POINT('',(0.118272920182323,-0.140952177533892,0.04));
#43860=CARTESIAN_POINT('',(0.140347709136006,-0.15636981978718,0.04));
#43861=CARTESIAN_POINT('',(0.118272920182323,-0.140952177533892,0.04));
#43862=CARTESIAN_POINT('Origin',(0.118272920182323,-0.140952177533892,0.04));
#43863=CARTESIAN_POINT('',(0.120889198458627,-0.146580359175541,0.185));
#43864=CARTESIAN_POINT('',(0.120889198458627,-0.146580359175541,0.0925));
#43865=CARTESIAN_POINT('',(0.118272920182323,-0.140952177533892,0.191));
#43866=CARTESIAN_POINT('',(0.118272920182323,-0.140952177533892,0.04));
#43867=CARTESIAN_POINT('Ctrl Pts',(0.120889198458627,-0.146580359175541,
0.185));
#43868=CARTESIAN_POINT('Ctrl Pts',(0.119560073131107,-0.143721122512702,
0.18805149911843));
#43869=CARTESIAN_POINT('Ctrl Pts',(0.118272920182323,-0.140952177533892,
0.191));
#43870=CARTESIAN_POINT('Origin',(0.140347709136006,-0.15636981978718,0.04));
#43871=CARTESIAN_POINT('',(0.123361285143431,-0.144506032150084,0.185));
#43872=CARTESIAN_POINT('',(0.123361285143431,-0.144506032150084,0.0925));
#43873=CARTESIAN_POINT('Ctrl Pts',(0.118272920182323,-0.140952177533892,
0.191));
#43874=CARTESIAN_POINT('Ctrl Pts',(0.120776286901169,-0.142700597986787,
0.188051499118449));
#43875=CARTESIAN_POINT('Ctrl Pts',(0.123361285143431,-0.144506032150084,
0.185));
#43876=CARTESIAN_POINT('Origin',(0.0985,-0.170607004545534,0.04));
#43877=CARTESIAN_POINT('',(0.0963939408860592,-0.163732123178242,0.04));
#43878=CARTESIAN_POINT('',(0.0935992076448907,-0.165345663167344,0.04));
#43879=CARTESIAN_POINT('Origin',(0.,0.,0.04));
#43880=CARTESIAN_POINT('',(0.092,-0.159348674296337,0.04));
#43881=CARTESIAN_POINT('',(0.111062177826491,-0.178365334794732,0.04));
#43882=CARTESIAN_POINT('',(0.092,-0.159348674296337,0.04));
#43883=CARTESIAN_POINT('Origin',(0.092,-0.159348674296337,0.04));
#43884=CARTESIAN_POINT('',(0.0935992076448907,-0.165345663167344,0.185));
#43885=CARTESIAN_POINT('',(0.0935992076448907,-0.165345663167344,0.0925));
#43886=CARTESIAN_POINT('',(0.092,-0.159348674296337,0.191));
#43887=CARTESIAN_POINT('',(0.092,-0.159348674296337,0.04));
#43888=CARTESIAN_POINT('Ctrl Pts',(0.0935992076448907,-0.165345663167344,
0.185));
#43889=CARTESIAN_POINT('Ctrl Pts',(0.0927867759536364,-0.162299064543037,
0.188051499118462));
#43890=CARTESIAN_POINT('Ctrl Pts',(0.092,-0.159348674296337,0.191));
#43891=CARTESIAN_POINT('Origin',(0.111062177826491,-0.178365334794732,0.04));
#43892=CARTESIAN_POINT('',(0.0963939408860592,-0.163732123178242,0.185));
#43893=CARTESIAN_POINT('',(0.0963939408860592,-0.163732123178242,0.0925));
#43894=CARTESIAN_POINT('Ctrl Pts',(0.092,-0.159348674296337,0.191));
#43895=CARTESIAN_POINT('Ctrl Pts',(0.0941617249279249,-0.161505237382646,
0.18805149911843));
#43896=CARTESIAN_POINT('Ctrl Pts',(0.0963939408860592,-0.163732123178242,
0.185));
#43897=CARTESIAN_POINT('Origin',(0.0673779682351567,-0.185119446294824,
0.04));
#43898=CARTESIAN_POINT('',(0.0664977155125524,-0.17798329649608,0.04));
#43899=CARTESIAN_POINT('',(0.0634652522703484,-0.179087022852749,0.04));
#43900=CARTESIAN_POINT('Origin',(0.,0.,0.04));
#43901=CARTESIAN_POINT('',(0.062931706371923,-0.172903442224607,0.04));
#43902=CARTESIAN_POINT('',(0.0784020784438917,-0.194941309361761,0.04));
#43903=CARTESIAN_POINT('',(0.062931706371923,-0.172903442224607,0.04));
#43904=CARTESIAN_POINT('Origin',(0.062931706371923,-0.172903442224607,0.04));
#43905=CARTESIAN_POINT('',(0.0634652522703484,-0.179087022852749,0.185));
#43906=CARTESIAN_POINT('',(0.0634652522703484,-0.179087022852749,0.0925));
#43907=CARTESIAN_POINT('',(0.062931706371923,-0.172903442224607,0.191));
#43908=CARTESIAN_POINT('',(0.062931706371923,-0.172903442224607,0.04));
#43909=CARTESIAN_POINT('Ctrl Pts',(0.0634652522703485,-0.179087022852749,
0.185));
#43910=CARTESIAN_POINT('Ctrl Pts',(0.0631941995412026,-0.175945631624558,
0.188051499118454));
#43911=CARTESIAN_POINT('Ctrl Pts',(0.062931706371923,-0.172903442224607,
0.191));
#43912=CARTESIAN_POINT('Origin',(0.0784020784438917,-0.194941309361761,
0.04));
#43913=CARTESIAN_POINT('',(0.0664977155125524,-0.17798329649608,0.185));
#43914=CARTESIAN_POINT('',(0.0664977155125524,-0.17798329649608,0.0925));
#43915=CARTESIAN_POINT('Ctrl Pts',(0.062931706371923,-0.172903442224607,
0.191));
#43916=CARTESIAN_POINT('Ctrl Pts',(0.0646861065908383,-0.175402621866182,
0.18805149911847));
#43917=CARTESIAN_POINT('Ctrl Pts',(0.0664977155125524,-0.17798329649608,
0.185));
#43918=CARTESIAN_POINT('Origin',(0.0342086910003852,-0.194007127343405,
0.04));
#43919=CARTESIAN_POINT('',(0.0345809907026645,-0.186826537413779,0.04));
#43920=CARTESIAN_POINT('',(0.031402937320539,-0.18738691397118,0.04));
#43921=CARTESIAN_POINT('Origin',(0.,0.,0.04));
#43922=CARTESIAN_POINT('',(0.0319512646907151,-0.181204626554246,0.04));
#43923=CARTESIAN_POINT('',(0.0433597715811408,-0.205594090888895,0.04));
#43924=CARTESIAN_POINT('',(0.0319512646907151,-0.181204626554246,0.04));
#43925=CARTESIAN_POINT('Origin',(0.0319512646907151,-0.181204626554246,
0.04));
#43926=CARTESIAN_POINT('',(0.031402937320539,-0.18738691397118,0.185));
#43927=CARTESIAN_POINT('',(0.031402937320539,-0.18738691397118,0.0925));
#43928=CARTESIAN_POINT('',(0.0319512646907151,-0.181204626554246,0.191));
#43929=CARTESIAN_POINT('',(0.0319512646907151,-0.181204626554246,0.04));
#43930=CARTESIAN_POINT('Ctrl Pts',(0.031402937320539,-0.18738691397118,
0.185));
#43931=CARTESIAN_POINT('Ctrl Pts',(0.0316814993535159,-0.184246179721939,
0.18805149911846));
#43932=CARTESIAN_POINT('Ctrl Pts',(0.0319512646907151,-0.181204626554246,
0.191));
#43933=CARTESIAN_POINT('Origin',(0.0433597715811408,-0.205594090888895,
0.04));
#43934=CARTESIAN_POINT('',(0.0345809907026646,-0.186826537413779,0.185));
#43935=CARTESIAN_POINT('',(0.0345809907026646,-0.186826537413779,0.0925));
#43936=CARTESIAN_POINT('Ctrl Pts',(0.0319512646907151,-0.181204626554246,
0.191));
#43937=CARTESIAN_POINT('Ctrl Pts',(0.0332450336377804,-0.18397048644238,
0.188051499118441));
#43938=CARTESIAN_POINT('Ctrl Pts',(0.0345809907026645,-0.186826537413779,
0.185));
#43939=CARTESIAN_POINT('Origin',(-4.16333634234434E-17,-0.197,0.04));
#43940=CARTESIAN_POINT('',(0.00161353998910185,-0.18999314853095,0.04));
#43941=CARTESIAN_POINT('',(-0.00161353998910192,-0.18999314853095,0.04));
#43942=CARTESIAN_POINT('Origin',(0.,0.,0.04));
#43943=CARTESIAN_POINT('',(-3.46944695195361E-17,-0.184,0.04));
#43944=CARTESIAN_POINT('',(0.00699999999999997,-0.21,0.04));
#43945=CARTESIAN_POINT('',(-3.46944695195361E-17,-0.184,0.04));
#43946=CARTESIAN_POINT('Origin',(-3.46944695195361E-17,-0.184,0.04));
#43947=CARTESIAN_POINT('',(-0.00161353998910191,-0.18999314853095,0.185));
#43948=CARTESIAN_POINT('',(-0.00161353998910191,-0.18999314853095,0.0925));
#43949=CARTESIAN_POINT('',(-3.46944695195361E-17,-0.184,0.191));
#43950=CARTESIAN_POINT('',(-3.46944695195361E-17,-0.184,0.04));
#43951=CARTESIAN_POINT('Ctrl Pts',(-0.0016135399891019,-0.18999314853095,
0.185));
#43952=CARTESIAN_POINT('Ctrl Pts',(-0.000793827160417415,-0.18694850088155,
0.18805149911845));
#43953=CARTESIAN_POINT('Ctrl Pts',(-3.46944695195361E-17,-0.184,0.191));
#43954=CARTESIAN_POINT('Origin',(0.00699999999999997,-0.21,0.04));
#43955=CARTESIAN_POINT('',(0.00161353998910184,-0.18999314853095,0.185));
#43956=CARTESIAN_POINT('',(0.00161353998910184,-0.18999314853095,0.0925));
#43957=CARTESIAN_POINT('Ctrl Pts',(-3.46944695195361E-17,-0.184,0.191));
#43958=CARTESIAN_POINT('Ctrl Pts',(0.000793827160417323,-0.18694850088155,
0.18805149911845));
#43959=CARTESIAN_POINT('Ctrl Pts',(0.00161353998910184,-0.18999314853095,
0.185));
#43960=CARTESIAN_POINT('Origin',(-0.0342086910003853,-0.194007127343405,
0.04));
#43961=CARTESIAN_POINT('',(-0.0314029373205391,-0.18738691397118,0.04));
#43962=CARTESIAN_POINT('',(-0.0345809907026646,-0.186826537413779,0.04));
#43963=CARTESIAN_POINT('Origin',(0.,0.,0.04));
#43964=CARTESIAN_POINT('',(-0.0319512646907152,-0.181204626554246,0.04));
#43965=CARTESIAN_POINT('',(-0.0295724630389699,-0.208025165376232,0.04));
#43966=CARTESIAN_POINT('',(-0.0319512646907152,-0.181204626554246,0.04));
#43967=CARTESIAN_POINT('Origin',(-0.0319512646907152,-0.181204626554246,
0.04));
#43968=CARTESIAN_POINT('',(-0.0345809907026646,-0.186826537413779,0.185));
#43969=CARTESIAN_POINT('',(-0.0345809907026646,-0.186826537413779,0.0925));
#43970=CARTESIAN_POINT('',(-0.0319512646907152,-0.181204626554246,0.191));
#43971=CARTESIAN_POINT('',(-0.0319512646907152,-0.181204626554246,0.04));
#43972=CARTESIAN_POINT('Ctrl Pts',(-0.0345809907026646,-0.186826537413779,
0.185));
#43973=CARTESIAN_POINT('Ctrl Pts',(-0.033245033637776,-0.18397048644237,
0.188051499118451));
#43974=CARTESIAN_POINT('Ctrl Pts',(-0.0319512646907152,-0.181204626554246,
0.191));
#43975=CARTESIAN_POINT('Origin',(-0.0295724630389699,-0.208025165376232,
0.04));
#43976=CARTESIAN_POINT('',(-0.0314029373205391,-0.18738691397118,0.185));
#43977=CARTESIAN_POINT('',(-0.0314029373205391,-0.18738691397118,0.0925));
#43978=CARTESIAN_POINT('Ctrl Pts',(-0.0319512646907152,-0.181204626554246,
0.191));
#43979=CARTESIAN_POINT('Ctrl Pts',(-0.0316814993535157,-0.184246179721942,
0.188051499118457));
#43980=CARTESIAN_POINT('Ctrl Pts',(-0.0314029373205391,-0.18738691397118,
0.185));
#43981=CARTESIAN_POINT('Origin',(-0.0673779682351569,-0.185119446294824,
0.04));
#43982=CARTESIAN_POINT('',(-0.0634652522703487,-0.179087022852749,0.04));
#43983=CARTESIAN_POINT('',(-0.0664977155125527,-0.17798329649608,0.04));
#43984=CARTESIAN_POINT('Origin',(0.,0.,0.04));
#43985=CARTESIAN_POINT('',(-0.0629317063719232,-0.172903442224607,0.04));
#43986=CARTESIAN_POINT('',(-0.0652463817528892,-0.19972959136832,0.04));
#43987=CARTESIAN_POINT('',(-0.0629317063719232,-0.172903442224607,0.04));
#43988=CARTESIAN_POINT('Origin',(-0.0629317063719232,-0.172903442224607,
0.04));
#43989=CARTESIAN_POINT('',(-0.0664977155125527,-0.17798329649608,0.185));
#43990=CARTESIAN_POINT('',(-0.0664977155125527,-0.17798329649608,0.0925));
#43991=CARTESIAN_POINT('',(-0.0629317063719232,-0.172903442224607,0.191));
#43992=CARTESIAN_POINT('',(-0.0629317063719232,-0.172903442224607,0.04));
#43993=CARTESIAN_POINT('Ctrl Pts',(-0.0664977155125527,-0.17798329649608,
0.185));
#43994=CARTESIAN_POINT('Ctrl Pts',(-0.0646861065908368,-0.175402621866179,
0.188051499118473));
#43995=CARTESIAN_POINT('Ctrl Pts',(-0.0629317063719232,-0.172903442224607,
0.191));
#43996=CARTESIAN_POINT('Origin',(-0.0652463817528892,-0.19972959136832,
0.04));
#43997=CARTESIAN_POINT('',(-0.0634652522703487,-0.179087022852749,0.185));
#43998=CARTESIAN_POINT('',(-0.0634652522703487,-0.179087022852749,0.0925));
#43999=CARTESIAN_POINT('Ctrl Pts',(-0.0629317063719232,-0.172903442224607,
0.191));
#44000=CARTESIAN_POINT('Ctrl Pts',(-0.0631941995412029,-0.175945631624558,
0.188051499118454));
#44001=CARTESIAN_POINT('Ctrl Pts',(-0.0634652522703487,-0.179087022852749,
0.185));
#44002=CARTESIAN_POINT('Origin',(-0.0985000000000001,-0.170607004545534,
0.04));
#44003=CARTESIAN_POINT('',(-0.0935992076448907,-0.165345663167344,0.04));
#44004=CARTESIAN_POINT('',(-0.0963939408860593,-0.163732123178242,0.04));
#44005=CARTESIAN_POINT('Origin',(0.,0.,0.04));
#44006=CARTESIAN_POINT('',(-0.0920000000000001,-0.159348674296337,0.04));
#44007=CARTESIAN_POINT('',(-0.098937822173509,-0.185365334794732,0.04));
#44008=CARTESIAN_POINT('',(-0.0920000000000001,-0.159348674296337,0.04));
#44009=CARTESIAN_POINT('Origin',(-0.0920000000000001,-0.159348674296337,
0.04));
#44010=CARTESIAN_POINT('',(-0.0963939408860593,-0.163732123178242,0.185));
#44011=CARTESIAN_POINT('',(-0.0963939408860593,-0.163732123178242,0.0925));
#44012=CARTESIAN_POINT('',(-0.0920000000000001,-0.159348674296337,0.191));
#44013=CARTESIAN_POINT('',(-0.0920000000000001,-0.159348674296337,0.04));
#44014=CARTESIAN_POINT('Ctrl Pts',(-0.0963939408860593,-0.163732123178242,
0.185));
#44015=CARTESIAN_POINT('Ctrl Pts',(-0.0941617249279212,-0.161505237382642,
0.188051499118436));
#44016=CARTESIAN_POINT('Ctrl Pts',(-0.0920000000000001,-0.159348674296337,
0.191));
#44017=CARTESIAN_POINT('Origin',(-0.098937822173509,-0.185365334794732,
0.04));
#44018=CARTESIAN_POINT('',(-0.0935992076448907,-0.165345663167344,0.185));
#44019=CARTESIAN_POINT('',(-0.0935992076448907,-0.165345663167344,0.0925));
#44020=CARTESIAN_POINT('Ctrl Pts',(-0.0920000000000001,-0.159348674296337,
0.191));
#44021=CARTESIAN_POINT('Ctrl Pts',(-0.0927867759536363,-0.162299064543036,
0.188051499118462));
#44022=CARTESIAN_POINT('Ctrl Pts',(-0.0935992076448907,-0.165345663167344,
0.185));
#44023=CARTESIAN_POINT('Origin',(-0.126629159108248,-0.150910755294439,
0.04));
#44024=CARTESIAN_POINT('',(-0.120889198458627,-0.146580359175541,0.04));
#44025=CARTESIAN_POINT('',(-0.123361285143431,-0.144506032150084,0.04));
#44026=CARTESIAN_POINT('Origin',(0.,0.,0.04));
#44027=CARTESIAN_POINT('',(-0.118272920182323,-0.140952177533892,0.04));
#44028=CARTESIAN_POINT('',(-0.12962308693234,-0.165368846322791,0.04));
#44029=CARTESIAN_POINT('',(-0.118272920182323,-0.140952177533892,0.04));
#44030=CARTESIAN_POINT('Origin',(-0.118272920182323,-0.140952177533892,
0.04));
#44031=CARTESIAN_POINT('',(-0.123361285143431,-0.144506032150084,0.185));
#44032=CARTESIAN_POINT('',(-0.123361285143431,-0.144506032150084,0.0925));
#44033=CARTESIAN_POINT('',(-0.118272920182323,-0.140952177533892,0.191));
#44034=CARTESIAN_POINT('',(-0.118272920182323,-0.140952177533892,0.04));
#44035=CARTESIAN_POINT('Ctrl Pts',(-0.123361285143431,-0.144506032150084,
0.185));
#44036=CARTESIAN_POINT('Ctrl Pts',(-0.120776286901195,-0.142700597986805,
0.188051499118418));
#44037=CARTESIAN_POINT('Ctrl Pts',(-0.118272920182323,-0.140952177533892,
0.191));
#44038=CARTESIAN_POINT('Origin',(-0.12962308693234,-0.165368846322791,0.04));
#44039=CARTESIAN_POINT('',(-0.120889198458627,-0.146580359175541,0.185));
#44040=CARTESIAN_POINT('',(-0.120889198458627,-0.146580359175541,0.0925));
#44041=CARTESIAN_POINT('Ctrl Pts',(-0.118272920182323,-0.140952177533892,
0.191));
#44042=CARTESIAN_POINT('Ctrl Pts',(-0.119560073131103,-0.143721122512692,
0.188051499118441));
#44043=CARTESIAN_POINT('Ctrl Pts',(-0.120889198458627,-0.146580359175541,
0.185));
#44044=CARTESIAN_POINT('Origin',(-0.150910755294439,-0.126629159108248,
0.04));
#44045=CARTESIAN_POINT('',(-0.144506032150084,-0.123361285143431,0.04));
#44046=CARTESIAN_POINT('',(-0.146580359175541,-0.120889198458627,0.04));
#44047=CARTESIAN_POINT('Origin',(0.,0.,0.04));
#44048=CARTESIAN_POINT('',(-0.140952177533892,-0.118272920182323,0.04));
#44049=CARTESIAN_POINT('',(-0.15636981978718,-0.140347709136006,0.04));
#44050=CARTESIAN_POINT('',(-0.140952177533892,-0.118272920182323,0.04));
#44051=CARTESIAN_POINT('Origin',(-0.140952177533892,-0.118272920182323,
0.04));
#44052=CARTESIAN_POINT('',(-0.146580359175541,-0.120889198458627,0.185));
#44053=CARTESIAN_POINT('',(-0.146580359175541,-0.120889198458627,0.0925));
#44054=CARTESIAN_POINT('',(-0.140952177533892,-0.118272920182323,0.191));
#44055=CARTESIAN_POINT('',(-0.140952177533892,-0.118272920182323,0.04));
#44056=CARTESIAN_POINT('Ctrl Pts',(-0.146580359175541,-0.120889198458627,
0.185));
#44057=CARTESIAN_POINT('Ctrl Pts',(-0.14372112251267,-0.119560073131093,
0.188051499118464));
#44058=CARTESIAN_POINT('Ctrl Pts',(-0.140952177533892,-0.118272920182323,
0.191));
#44059=CARTESIAN_POINT('Origin',(-0.15636981978718,-0.140347709136006,0.04));
#44060=CARTESIAN_POINT('',(-0.144506032150084,-0.123361285143431,0.185));
#44061=CARTESIAN_POINT('',(-0.144506032150084,-0.123361285143431,0.0925));
#44062=CARTESIAN_POINT('Ctrl Pts',(-0.140952177533892,-0.118272920182323,
0.191));
#44063=CARTESIAN_POINT('Ctrl Pts',(-0.142700597986788,-0.120776286901171,
0.188051499118446));
#44064=CARTESIAN_POINT('Ctrl Pts',(-0.144506032150084,-0.123361285143431,
0.185));
#44065=CARTESIAN_POINT('Origin',(-0.170607004545534,-0.0985,0.04));
#44066=CARTESIAN_POINT('',(-0.163732123178242,-0.0963939408860592,0.04));
#44067=CARTESIAN_POINT('',(-0.165345663167344,-0.0935992076448906,0.04));
#44068=CARTESIAN_POINT('Origin',(0.,0.,0.04));
#44069=CARTESIAN_POINT('',(-0.159348674296337,-0.092,0.04));
#44070=CARTESIAN_POINT('',(-0.178365334794732,-0.111062177826491,0.04));
#44071=CARTESIAN_POINT('',(-0.159348674296337,-0.092,0.04));
#44072=CARTESIAN_POINT('Origin',(-0.159348674296337,-0.092,0.04));
#44073=CARTESIAN_POINT('',(-0.165345663167344,-0.0935992076448906,0.185));
#44074=CARTESIAN_POINT('',(-0.165345663167344,-0.0935992076448906,0.0925));
#44075=CARTESIAN_POINT('',(-0.159348674296337,-0.0919999999999999,0.191));
#44076=CARTESIAN_POINT('',(-0.159348674296337,-0.092,0.04));
#44077=CARTESIAN_POINT('Ctrl Pts',(-0.165345663167344,-0.0935992076448906,
0.185));
#44078=CARTESIAN_POINT('Ctrl Pts',(-0.16229906454304,-0.0927867759536372,
0.188051499118458));
#44079=CARTESIAN_POINT('Ctrl Pts',(-0.159348674296337,-0.0919999999999999,
0.191));
#44080=CARTESIAN_POINT('Origin',(-0.178365334794732,-0.111062177826491,
0.04));
#44081=CARTESIAN_POINT('',(-0.163732123178242,-0.0963939408860592,0.185));
#44082=CARTESIAN_POINT('',(-0.163732123178242,-0.0963939408860592,0.0925));
#44083=CARTESIAN_POINT('Ctrl Pts',(-0.159348674296337,-0.0919999999999999,
0.191));
#44084=CARTESIAN_POINT('Ctrl Pts',(-0.161505237382618,-0.0941617249278968,
0.188051499118469));
#44085=CARTESIAN_POINT('Ctrl Pts',(-0.163732123178242,-0.0963939408860592,
0.185));
#44086=CARTESIAN_POINT('Origin',(-0.185119446294824,-0.0673779682351567,
0.04));
#44087=CARTESIAN_POINT('',(-0.17798329649608,-0.0664977155125525,0.04));
#44088=CARTESIAN_POINT('',(-0.179087022852749,-0.0634652522703485,0.04));
#44089=CARTESIAN_POINT('Origin',(0.,0.,0.04));
#44090=CARTESIAN_POINT('',(-0.172903442224607,-0.062931706371923,0.04));
#44091=CARTESIAN_POINT('',(-0.194941309361761,-0.0784020784438918,0.04));
#44092=CARTESIAN_POINT('',(-0.172903442224607,-0.062931706371923,0.04));
#44093=CARTESIAN_POINT('Origin',(-0.172903442224607,-0.062931706371923,
0.04));
#44094=CARTESIAN_POINT('',(-0.179087022852749,-0.0634652522703485,0.185));
#44095=CARTESIAN_POINT('',(-0.179087022852749,-0.0634652522703485,0.0925));
#44096=CARTESIAN_POINT('',(-0.172903442224607,-0.062931706371923,0.191));
#44097=CARTESIAN_POINT('',(-0.172903442224607,-0.062931706371923,0.04));
#44098=CARTESIAN_POINT('Ctrl Pts',(-0.179087022852749,-0.0634652522703485,
0.185));
#44099=CARTESIAN_POINT('Ctrl Pts',(-0.175945631624537,-0.0631941995412009,
0.188051499118474));
#44100=CARTESIAN_POINT('Ctrl Pts',(-0.172903442224607,-0.062931706371923,
0.191));
#44101=CARTESIAN_POINT('Origin',(-0.194941309361761,-0.0784020784438918,
0.04));
#44102=CARTESIAN_POINT('',(-0.17798329649608,-0.0664977155125525,0.185));
#44103=CARTESIAN_POINT('',(-0.17798329649608,-0.0664977155125525,0.0925));
#44104=CARTESIAN_POINT('Ctrl Pts',(-0.172903442224607,-0.062931706371923,
0.191));
#44105=CARTESIAN_POINT('Ctrl Pts',(-0.175402621866193,-0.0646861065908464,
0.188051499118456));
#44106=CARTESIAN_POINT('Ctrl Pts',(-0.17798329649608,-0.0664977155125525,
0.185));
#44107=CARTESIAN_POINT('Origin',(-0.194007127343405,-0.0342086910003852,
0.04));
#44108=CARTESIAN_POINT('',(-0.186826537413779,-0.0345809907026646,0.04));
#44109=CARTESIAN_POINT('',(-0.18738691397118,-0.031402937320539,0.04));
#44110=CARTESIAN_POINT('Origin',(0.,0.,0.04));
#44111=CARTESIAN_POINT('',(-0.181204626554246,-0.0319512646907151,0.04));
#44112=CARTESIAN_POINT('',(-0.205594090888895,-0.0433597715811408,0.04));
#44113=CARTESIAN_POINT('',(-0.181204626554246,-0.0319512646907151,0.04));
#44114=CARTESIAN_POINT('Origin',(-0.181204626554246,-0.0319512646907151,
0.04));
#44115=CARTESIAN_POINT('',(-0.18738691397118,-0.031402937320539,0.185));
#44116=CARTESIAN_POINT('',(-0.18738691397118,-0.031402937320539,0.0925));
#44117=CARTESIAN_POINT('',(-0.181204626554246,-0.0319512646907151,0.191));
#44118=CARTESIAN_POINT('',(-0.181204626554246,-0.0319512646907151,0.04));
#44119=CARTESIAN_POINT('Ctrl Pts',(-0.18738691397118,-0.031402937320539,
0.185));
#44120=CARTESIAN_POINT('Ctrl Pts',(-0.184246179721915,-0.031681499353518,
0.188051499118483));
#44121=CARTESIAN_POINT('Ctrl Pts',(-0.181204626554246,-0.0319512646907151,
0.191));
#44122=CARTESIAN_POINT('Origin',(-0.205594090888895,-0.0433597715811408,
0.04));
#44123=CARTESIAN_POINT('',(-0.186826537413779,-0.0345809907026646,0.185));
#44124=CARTESIAN_POINT('',(-0.186826537413779,-0.0345809907026646,0.0925));
#44125=CARTESIAN_POINT('Ctrl Pts',(-0.181204626554246,-0.0319512646907151,
0.191));
#44126=CARTESIAN_POINT('Ctrl Pts',(-0.183970486442384,-0.0332450336377824,
0.188051499118436));
#44127=CARTESIAN_POINT('Ctrl Pts',(-0.186826537413779,-0.0345809907026646,
0.185));
#44128=CARTESIAN_POINT('Origin',(-0.197,2.08166817117217E-17,0.04));
#44129=CARTESIAN_POINT('',(-0.18999314853095,-0.00161353998910186,0.04));
#44130=CARTESIAN_POINT('',(-0.19,-2.32682891837997E-17,0.04));
#44131=CARTESIAN_POINT('Origin',(0.,0.,0.04));
#44132=CARTESIAN_POINT('',(-0.184,2.08166817117217E-17,0.04));
#44133=CARTESIAN_POINT('',(-0.21,-0.00699999999999998,0.04));
#44134=CARTESIAN_POINT('',(-0.18999314853095,0.0016135399891019,0.04));
#44135=CARTESIAN_POINT('',(-0.184,2.08166817117217E-17,0.04));
#44136=CARTESIAN_POINT('Origin',(0.,0.,0.04));
#44137=CARTESIAN_POINT('Origin',(-0.184,2.08166817117217E-17,0.04));
#44138=CARTESIAN_POINT('',(-0.18999314853095,0.00161353998910189,0.185));
#44139=CARTESIAN_POINT('',(-0.18999314853095,0.00161353998910189,0.0925));
#44140=CARTESIAN_POINT('',(-0.184,2.08166817117217E-17,0.191));
#44141=CARTESIAN_POINT('',(-0.184,2.08166817117217E-17,0.04));
#44142=CARTESIAN_POINT('Ctrl Pts',(-0.18999314853095,0.00161353998910189,
0.185));
#44143=CARTESIAN_POINT('Ctrl Pts',(-0.186948500881544,0.000793827160415821,
0.188051499118456));
#44144=CARTESIAN_POINT('Ctrl Pts',(-0.184,2.08166817117217E-17,0.191));
#44145=CARTESIAN_POINT('Origin',(-0.21,-0.00699999999999998,0.04));
#44146=CARTESIAN_POINT('',(-0.18999314853095,-0.00161353998910186,0.185));
#44147=CARTESIAN_POINT('',(-0.18999314853095,-0.00161353998910186,0.0925));
#44148=CARTESIAN_POINT('Ctrl Pts',(-0.184,2.08166817117217E-17,0.191));
#44149=CARTESIAN_POINT('Ctrl Pts',(-0.186948500881545,-0.000793827160416021,
0.188051499118455));
#44150=CARTESIAN_POINT('Ctrl Pts',(-0.18999314853095,-0.00161353998910185,
0.185));
#44151=CARTESIAN_POINT('Origin',(-0.194007127343405,0.0342086910003854,
0.04));
#44152=CARTESIAN_POINT('',(-0.18738691397118,0.0314029373205392,0.04));
#44153=CARTESIAN_POINT('',(-0.186826537413779,0.0345809907026647,0.04));
#44154=CARTESIAN_POINT('Origin',(0.,0.,0.04));
#44155=CARTESIAN_POINT('',(-0.181204626554246,0.0319512646907152,0.04));
#44156=CARTESIAN_POINT('',(-0.208025165376232,0.02957246303897,0.04));
#44157=CARTESIAN_POINT('',(-0.181204626554246,0.0319512646907152,0.04));
#44158=CARTESIAN_POINT('Origin',(-0.181204626554246,0.0319512646907152,
0.04));
#44159=CARTESIAN_POINT('',(-0.186826537413779,0.0345809907026647,0.185));
#44160=CARTESIAN_POINT('',(-0.186826537413779,0.0345809907026647,0.0925));
#44161=CARTESIAN_POINT('',(-0.181204626554246,0.0319512646907153,0.191));
#44162=CARTESIAN_POINT('',(-0.181204626554246,0.0319512646907152,0.04));
#44163=CARTESIAN_POINT('Ctrl Pts',(-0.186826537413779,0.0345809907026647,
0.185));
#44164=CARTESIAN_POINT('Ctrl Pts',(-0.183970486442384,0.0332450336377824,
0.188051499118436));
#44165=CARTESIAN_POINT('Ctrl Pts',(-0.181204626554246,0.0319512646907153,
0.191));
#44166=CARTESIAN_POINT('Origin',(-0.208025165376232,0.02957246303897,0.04));
#44167=CARTESIAN_POINT('',(-0.18738691397118,0.0314029373205392,0.185));
#44168=CARTESIAN_POINT('',(-0.18738691397118,0.0314029373205392,0.0925));
#44169=CARTESIAN_POINT('Ctrl Pts',(-0.181204626554246,0.0319512646907153,
0.191));
#44170=CARTESIAN_POINT('Ctrl Pts',(-0.184246179721934,0.0316814993535164,
0.188051499118464));
#44171=CARTESIAN_POINT('Ctrl Pts',(-0.18738691397118,0.0314029373205392,
0.185));
#44172=CARTESIAN_POINT('Origin',(-0.185119446294824,0.0673779682351568,
0.04));
#44173=CARTESIAN_POINT('',(-0.179087022852749,0.0634652522703486,0.04));
#44174=CARTESIAN_POINT('',(-0.17798329649608,0.0664977155125526,0.04));
#44175=CARTESIAN_POINT('Origin',(0.,0.,0.04));
#44176=CARTESIAN_POINT('',(-0.172903442224607,0.0629317063719231,0.04));
#44177=CARTESIAN_POINT('',(-0.199729591368321,0.0652463817528891,0.04));
#44178=CARTESIAN_POINT('',(-0.172903442224607,0.0629317063719231,0.04));
#44179=CARTESIAN_POINT('Origin',(-0.172903442224607,0.0629317063719231,
0.04));
#44180=CARTESIAN_POINT('',(-0.17798329649608,0.0664977155125526,0.185));
#44181=CARTESIAN_POINT('',(-0.17798329649608,0.0664977155125526,0.0925));
#44182=CARTESIAN_POINT('',(-0.172903442224607,0.0629317063719231,0.191));
#44183=CARTESIAN_POINT('',(-0.172903442224607,0.0629317063719231,0.04));
#44184=CARTESIAN_POINT('Ctrl Pts',(-0.17798329649608,0.0664977155125526,
0.185));
#44185=CARTESIAN_POINT('Ctrl Pts',(-0.175402621866187,0.0646861065908417,
0.188051499118464));
#44186=CARTESIAN_POINT('Ctrl Pts',(-0.172903442224607,0.0629317063719231,
0.191));
#44187=CARTESIAN_POINT('Origin',(-0.199729591368321,0.0652463817528891,
0.04));
#44188=CARTESIAN_POINT('',(-0.179087022852749,0.0634652522703485,0.185));
#44189=CARTESIAN_POINT('',(-0.179087022852749,0.0634652522703485,0.0925));
#44190=CARTESIAN_POINT('Ctrl Pts',(-0.172903442224607,0.0629317063719231,
0.191));
#44191=CARTESIAN_POINT('Ctrl Pts',(-0.175945631624522,0.0631941995411996,
0.188051499118489));
#44192=CARTESIAN_POINT('Ctrl Pts',(-0.179087022852749,0.0634652522703486,
0.185));
#44193=CARTESIAN_POINT('Origin',(-0.170607004545534,0.0985,0.04));
#44194=CARTESIAN_POINT('',(-0.165345663167344,0.0935992076448906,0.04));
#44195=CARTESIAN_POINT('',(-0.163732123178242,0.0963939408860592,0.04));
#44196=CARTESIAN_POINT('Origin',(0.,0.,0.04));
#44197=CARTESIAN_POINT('',(-0.159348674296337,0.092,0.04));
#44198=CARTESIAN_POINT('',(-0.185365334794732,0.098937822173509,0.04));
#44199=CARTESIAN_POINT('',(-0.159348674296337,0.092,0.04));
#44200=CARTESIAN_POINT('Origin',(-0.159348674296337,0.092,0.04));
#44201=CARTESIAN_POINT('',(-0.163732123178242,0.0963939408860592,0.185));
#44202=CARTESIAN_POINT('',(-0.163732123178242,0.0963939408860592,0.0925));
#44203=CARTESIAN_POINT('',(-0.159348674296337,0.092,0.191));
#44204=CARTESIAN_POINT('',(-0.159348674296337,0.092,0.04));
#44205=CARTESIAN_POINT('Ctrl Pts',(-0.163732123178242,0.0963939408860592,
0.185));
#44206=CARTESIAN_POINT('Ctrl Pts',(-0.161505237382624,0.0941617249279029,
0.18805149911846));
#44207=CARTESIAN_POINT('Ctrl Pts',(-0.159348674296337,0.092,0.191));
#44208=CARTESIAN_POINT('Origin',(-0.185365334794732,0.098937822173509,0.04));
#44209=CARTESIAN_POINT('',(-0.165345663167344,0.0935992076448906,0.185));
#44210=CARTESIAN_POINT('',(-0.165345663167344,0.0935992076448906,0.0925));
#44211=CARTESIAN_POINT('Ctrl Pts',(-0.159348674296337,0.092,0.191));
#44212=CARTESIAN_POINT('Ctrl Pts',(-0.162299064543065,0.0927867759536439,
0.188051499118434));
#44213=CARTESIAN_POINT('Ctrl Pts',(-0.165345663167344,0.0935992076448907,
0.185));
#44214=CARTESIAN_POINT('Origin',(-0.150910755294439,0.126629159108248,0.04));
#44215=CARTESIAN_POINT('',(-0.146580359175541,0.120889198458627,0.04));
#44216=CARTESIAN_POINT('',(-0.144506032150084,0.123361285143431,0.04));
#44217=CARTESIAN_POINT('Origin',(0.,0.,0.04));
#44218=CARTESIAN_POINT('',(-0.140952177533892,0.118272920182323,0.04));
#44219=CARTESIAN_POINT('',(-0.165368846322791,0.12962308693234,0.04));
#44220=CARTESIAN_POINT('',(-0.140952177533892,0.118272920182323,0.04));
#44221=CARTESIAN_POINT('Origin',(-0.140952177533892,0.118272920182323,0.04));
#44222=CARTESIAN_POINT('',(-0.144506032150084,0.123361285143431,0.185));
#44223=CARTESIAN_POINT('',(-0.144506032150084,0.123361285143431,0.0925));
#44224=CARTESIAN_POINT('',(-0.140952177533892,0.118272920182323,0.191));
#44225=CARTESIAN_POINT('',(-0.140952177533892,0.118272920182323,0.04));
#44226=CARTESIAN_POINT('Ctrl Pts',(-0.144506032150084,0.123361285143431,
0.185));
#44227=CARTESIAN_POINT('Ctrl Pts',(-0.142700597986805,0.120776286901195,
0.188051499118418));
#44228=CARTESIAN_POINT('Ctrl Pts',(-0.140952177533892,0.118272920182323,
0.191));
#44229=CARTESIAN_POINT('Origin',(-0.165368846322791,0.12962308693234,0.04));
#44230=CARTESIAN_POINT('',(-0.146580359175541,0.120889198458627,0.185));
#44231=CARTESIAN_POINT('',(-0.146580359175541,0.120889198458627,0.0925));
#44232=CARTESIAN_POINT('Ctrl Pts',(-0.140952177533892,0.118272920182323,
0.191));
#44233=CARTESIAN_POINT('Ctrl Pts',(-0.143721122512692,0.119560073131103,
0.188051499118441));
#44234=CARTESIAN_POINT('Ctrl Pts',(-0.146580359175541,0.120889198458627,
0.185));
#44235=CARTESIAN_POINT('Origin',(-0.126629159108248,0.150910755294439,0.04));
#44236=CARTESIAN_POINT('',(-0.123361285143431,0.144506032150084,0.04));
#44237=CARTESIAN_POINT('',(-0.120889198458627,0.146580359175541,0.04));
#44238=CARTESIAN_POINT('Origin',(0.,0.,0.04));
#44239=CARTESIAN_POINT('',(-0.118272920182323,0.140952177533892,0.04));
#44240=CARTESIAN_POINT('',(-0.140347709136006,0.15636981978718,0.04));
#44241=CARTESIAN_POINT('',(-0.118272920182323,0.140952177533892,0.04));
#44242=CARTESIAN_POINT('Origin',(-0.118272920182323,0.140952177533892,0.04));
#44243=CARTESIAN_POINT('',(-0.120889198458627,0.146580359175541,0.185));
#44244=CARTESIAN_POINT('',(-0.120889198458627,0.146580359175541,0.0925));
#44245=CARTESIAN_POINT('',(-0.118272920182323,0.140952177533892,0.191));
#44246=CARTESIAN_POINT('',(-0.118272920182323,0.140952177533892,0.04));
#44247=CARTESIAN_POINT('Ctrl Pts',(-0.120889198458627,0.146580359175541,
0.185));
#44248=CARTESIAN_POINT('Ctrl Pts',(-0.1195600731311,0.143721122512687,0.188051499118446));
#44249=CARTESIAN_POINT('Ctrl Pts',(-0.118272920182323,0.140952177533892,
0.191));
#44250=CARTESIAN_POINT('Origin',(-0.140347709136006,0.15636981978718,0.04));
#44251=CARTESIAN_POINT('',(-0.123361285143431,0.144506032150084,0.185));
#44252=CARTESIAN_POINT('',(-0.123361285143431,0.144506032150084,0.0925));
#44253=CARTESIAN_POINT('Ctrl Pts',(-0.118272920182323,0.140952177533892,
0.191));
#44254=CARTESIAN_POINT('Ctrl Pts',(-0.120776286901187,0.142700597986799,
0.188051499118427));
#44255=CARTESIAN_POINT('Ctrl Pts',(-0.123361285143431,0.144506032150084,
0.185));
#44256=CARTESIAN_POINT('Origin',(-0.0985,0.170607004545534,0.04));
#44257=CARTESIAN_POINT('',(-0.0963939408860591,0.163732123178242,0.04));
#44258=CARTESIAN_POINT('',(-0.0935992076448906,0.165345663167344,0.04));
#44259=CARTESIAN_POINT('Origin',(0.,0.,0.04));
#44260=CARTESIAN_POINT('',(-0.092,0.159348674296337,0.04));
#44261=CARTESIAN_POINT('',(-0.111062177826491,0.178365334794732,0.04));
#44262=CARTESIAN_POINT('',(-0.092,0.159348674296337,0.04));
#44263=CARTESIAN_POINT('Origin',(-0.092,0.159348674296337,0.04));
#44264=CARTESIAN_POINT('',(-0.0935992076448906,0.165345663167344,0.185));
#44265=CARTESIAN_POINT('',(-0.0935992076448906,0.165345663167344,0.0925));
#44266=CARTESIAN_POINT('',(-0.092,0.159348674296337,0.191));
#44267=CARTESIAN_POINT('',(-0.092,0.159348674296337,0.04));
#44268=CARTESIAN_POINT('Ctrl Pts',(-0.0935992076448906,0.165345663167344,
0.185));
#44269=CARTESIAN_POINT('Ctrl Pts',(-0.0927867759536353,0.162299064543033,
0.188051499118466));
#44270=CARTESIAN_POINT('Ctrl Pts',(-0.092,0.159348674296337,0.191));
#44271=CARTESIAN_POINT('Origin',(-0.111062177826491,0.178365334794732,0.04));
#44272=CARTESIAN_POINT('',(-0.0963939408860592,0.163732123178242,0.185));
#44273=CARTESIAN_POINT('',(-0.0963939408860592,0.163732123178242,0.0925));
#44274=CARTESIAN_POINT('Ctrl Pts',(-0.092,0.159348674296337,0.191));
#44275=CARTESIAN_POINT('Ctrl Pts',(-0.0941617249279073,0.161505237382628,
0.188051499118454));
#44276=CARTESIAN_POINT('Ctrl Pts',(-0.0963939408860592,0.163732123178242,
0.185));
#44277=CARTESIAN_POINT('Origin',(-0.0673779682351567,0.185119446294824,
0.04));
#44278=CARTESIAN_POINT('',(-0.0664977155125525,0.17798329649608,0.04));
#44279=CARTESIAN_POINT('',(-0.0634652522703485,0.179087022852749,0.04));
#44280=CARTESIAN_POINT('Origin',(0.,0.,0.04));
#44281=CARTESIAN_POINT('',(-0.062931706371923,0.172903442224607,0.04));
#44282=CARTESIAN_POINT('',(-0.0784020784438918,0.194941309361761,0.04));
#44283=CARTESIAN_POINT('',(-0.062931706371923,0.172903442224607,0.04));
#44284=CARTESIAN_POINT('Origin',(-0.062931706371923,0.172903442224607,0.04));
#44285=CARTESIAN_POINT('',(-0.0634652522703485,0.179087022852749,0.185));
#44286=CARTESIAN_POINT('',(-0.0634652522703485,0.179087022852749,0.0925));
#44287=CARTESIAN_POINT('',(-0.062931706371923,0.172903442224607,0.191));
#44288=CARTESIAN_POINT('',(-0.062931706371923,0.172903442224607,0.04));
#44289=CARTESIAN_POINT('Ctrl Pts',(-0.0634652522703485,0.179087022852749,
0.185));
#44290=CARTESIAN_POINT('Ctrl Pts',(-0.0631941995412009,0.175945631624537,
0.188051499118474));
#44291=CARTESIAN_POINT('Ctrl Pts',(-0.062931706371923,0.172903442224607,
0.191));
#44292=CARTESIAN_POINT('Origin',(-0.0784020784438918,0.194941309361761,
0.04));
#44293=CARTESIAN_POINT('',(-0.0664977155125525,0.17798329649608,0.185));
#44294=CARTESIAN_POINT('',(-0.0664977155125525,0.17798329649608,0.0925));
#44295=CARTESIAN_POINT('Ctrl Pts',(-0.062931706371923,0.172903442224607,
0.191));
#44296=CARTESIAN_POINT('Ctrl Pts',(-0.0646861065908464,0.175402621866193,
0.188051499118456));
#44297=CARTESIAN_POINT('Ctrl Pts',(-0.0664977155125525,0.17798329649608,
0.185));
#44298=CARTESIAN_POINT('Origin',(-0.0342086910003853,0.194007127343405,
0.04));
#44299=CARTESIAN_POINT('',(-0.0345809907026646,0.186826537413779,0.04));
#44300=CARTESIAN_POINT('',(-0.0314029373205391,0.18738691397118,0.04));
#44301=CARTESIAN_POINT('Origin',(0.,0.,0.04));
#44302=CARTESIAN_POINT('',(-0.0319512646907152,0.181204626554246,0.04));
#44303=CARTESIAN_POINT('',(-0.0433597715811408,0.205594090888895,0.04));
#44304=CARTESIAN_POINT('',(-0.0319512646907152,0.181204626554246,0.04));
#44305=CARTESIAN_POINT('Origin',(-0.0319512646907152,0.181204626554246,
0.04));
#44306=CARTESIAN_POINT('',(-0.0314029373205391,0.18738691397118,0.185));
#44307=CARTESIAN_POINT('',(-0.0314029373205391,0.18738691397118,0.0925));
#44308=CARTESIAN_POINT('',(-0.0319512646907152,0.181204626554246,0.191));
#44309=CARTESIAN_POINT('',(-0.0319512646907152,0.181204626554246,0.04));
#44310=CARTESIAN_POINT('Ctrl Pts',(-0.0314029373205391,0.18738691397118,
0.185));
#44311=CARTESIAN_POINT('Ctrl Pts',(-0.031681499353516,0.184246179721939,
0.18805149911846));
#44312=CARTESIAN_POINT('Ctrl Pts',(-0.0319512646907152,0.181204626554246,
0.191));
#44313=CARTESIAN_POINT('Origin',(-0.0433597715811408,0.205594090888895,
0.04));
#44314=CARTESIAN_POINT('',(-0.0345809907026646,0.186826537413779,0.185));
#44315=CARTESIAN_POINT('',(-0.0345809907026646,0.186826537413779,0.0925));
#44316=CARTESIAN_POINT('Ctrl Pts',(-0.0319512646907152,0.181204626554246,
0.191));
#44317=CARTESIAN_POINT('Ctrl Pts',(-0.033245033637777,0.183970486442373,
0.188051499118448));
#44318=CARTESIAN_POINT('Ctrl Pts',(-0.0345809907026646,0.186826537413779,
0.185));
#44319=CARTESIAN_POINT('Origin',(1.38777878078145E-17,0.197,0.04));
#44320=CARTESIAN_POINT('',(-0.00161353998910187,0.18999314853095,0.04));
#44321=CARTESIAN_POINT('',(0.00161353998910189,0.18999314853095,0.04));
#44322=CARTESIAN_POINT('Origin',(0.,0.,0.04));
#44323=CARTESIAN_POINT('',(6.93889390390723E-18,0.184,0.04));
#44324=CARTESIAN_POINT('',(-0.00699999999999999,0.21,0.04));
#44325=CARTESIAN_POINT('',(6.93889390390723E-18,0.184,0.04));
#44326=CARTESIAN_POINT('Origin',(6.93889390390723E-18,0.184,0.04));
#44327=CARTESIAN_POINT('',(0.00161353998910188,0.18999314853095,0.185));
#44328=CARTESIAN_POINT('',(0.00161353998910188,0.18999314853095,0.0925));
#44329=CARTESIAN_POINT('',(6.93889390390723E-18,0.184,0.191));
#44330=CARTESIAN_POINT('',(6.93889390390723E-18,0.184,0.04));
#44331=CARTESIAN_POINT('Ctrl Pts',(0.00161353998910188,0.18999314853095,
0.185));
#44332=CARTESIAN_POINT('Ctrl Pts',(0.000793827160417808,0.186948500881552,
0.188051499118448));
#44333=CARTESIAN_POINT('Ctrl Pts',(6.93889390390723E-18,0.184,0.191));
#44334=CARTESIAN_POINT('Origin',(-0.00699999999999999,0.21,0.04));
#44335=CARTESIAN_POINT('',(-0.00161353998910187,0.18999314853095,0.185));
#44336=CARTESIAN_POINT('',(-0.00161353998910187,0.18999314853095,0.0925));
#44337=CARTESIAN_POINT('Ctrl Pts',(6.93889390390723E-18,0.184,0.191));
#44338=CARTESIAN_POINT('Ctrl Pts',(-0.000793827160415599,0.186948500881544,
0.188051499118456));
#44339=CARTESIAN_POINT('Ctrl Pts',(-0.00161353998910187,0.18999314853095,
0.185));
#44340=CARTESIAN_POINT('Origin',(0.0342086910003853,0.194007127343405,0.04));
#44341=CARTESIAN_POINT('',(0.0314029373205391,0.18738691397118,0.04));
#44342=CARTESIAN_POINT('',(0.0345809907026646,0.186826537413779,0.04));
#44343=CARTESIAN_POINT('Origin',(0.,0.,0.04));
#44344=CARTESIAN_POINT('',(0.0319512646907152,0.181204626554246,0.04));
#44345=CARTESIAN_POINT('',(0.02957246303897,0.208025165376232,0.04));
#44346=CARTESIAN_POINT('',(0.0319512646907152,0.181204626554246,0.04));
#44347=CARTESIAN_POINT('Origin',(0.0319512646907152,0.181204626554246,0.04));
#44348=CARTESIAN_POINT('',(0.0345809907026646,0.186826537413779,0.185));
#44349=CARTESIAN_POINT('',(0.0345809907026646,0.186826537413779,0.0925));
#44350=CARTESIAN_POINT('',(0.0319512646907152,0.181204626554246,0.191));
#44351=CARTESIAN_POINT('',(0.0319512646907152,0.181204626554246,0.04));
#44352=CARTESIAN_POINT('Ctrl Pts',(0.0345809907026646,0.186826537413779,
0.185));
#44353=CARTESIAN_POINT('Ctrl Pts',(0.0332450336377822,0.183970486442384,
0.188051499118437));
#44354=CARTESIAN_POINT('Ctrl Pts',(0.0319512646907152,0.181204626554246,
0.191));
#44355=CARTESIAN_POINT('Origin',(0.02957246303897,0.208025165376232,0.04));
#44356=CARTESIAN_POINT('',(0.0314029373205391,0.18738691397118,0.185));
#44357=CARTESIAN_POINT('',(0.0314029373205391,0.18738691397118,0.0925));
#44358=CARTESIAN_POINT('Ctrl Pts',(0.0319512646907152,0.181204626554246,
0.191));
#44359=CARTESIAN_POINT('Ctrl Pts',(0.0316814993535166,0.184246179721932,
0.188051499118467));
#44360=CARTESIAN_POINT('Ctrl Pts',(0.0314029373205392,0.18738691397118,
0.185));
#44361=CARTESIAN_POINT('Origin',(0.0673779682351568,0.185119446294824,0.04));
#44362=CARTESIAN_POINT('',(0.0634652522703486,0.179087022852749,0.04));
#44363=CARTESIAN_POINT('',(0.0664977155125526,0.17798329649608,0.04));
#44364=CARTESIAN_POINT('Origin',(0.,0.,0.04));
#44365=CARTESIAN_POINT('',(0.0629317063719231,0.172903442224607,0.04));
#44366=CARTESIAN_POINT('',(0.0652463817528891,0.199729591368321,0.04));
#44367=CARTESIAN_POINT('',(0.0629317063719231,0.172903442224607,0.04));
#44368=CARTESIAN_POINT('Origin',(0.0629317063719231,0.172903442224607,0.04));
#44369=CARTESIAN_POINT('',(0.0664977155125526,0.17798329649608,0.185));
#44370=CARTESIAN_POINT('',(0.0664977155125526,0.17798329649608,0.0925));
#44371=CARTESIAN_POINT('',(0.0629317063719231,0.172903442224607,0.191));
#44372=CARTESIAN_POINT('',(0.0629317063719231,0.172903442224607,0.04));
#44373=CARTESIAN_POINT('Ctrl Pts',(0.0664977155125526,0.17798329649608,
0.185));
#44374=CARTESIAN_POINT('Ctrl Pts',(0.0646861065908417,0.175402621866187,
0.188051499118464));
#44375=CARTESIAN_POINT('Ctrl Pts',(0.0629317063719231,0.172903442224607,
0.191));
#44376=CARTESIAN_POINT('Origin',(0.0652463817528891,0.199729591368321,0.04));
#44377=CARTESIAN_POINT('',(0.0634652522703485,0.179087022852749,0.185));
#44378=CARTESIAN_POINT('',(0.0634652522703485,0.179087022852749,0.0925));
#44379=CARTESIAN_POINT('Ctrl Pts',(0.0629317063719231,0.172903442224607,
0.191));
#44380=CARTESIAN_POINT('Ctrl Pts',(0.0631941995411996,0.175945631624522,
0.188051499118489));
#44381=CARTESIAN_POINT('Ctrl Pts',(0.0634652522703486,0.179087022852749,
0.185));
#44382=CARTESIAN_POINT('Origin',(0.0985,0.170607004545534,0.04));
#44383=CARTESIAN_POINT('',(0.0935992076448906,0.165345663167344,0.04));
#44384=CARTESIAN_POINT('',(0.0963939408860592,0.163732123178242,0.04));
#44385=CARTESIAN_POINT('Origin',(0.,0.,0.04));
#44386=CARTESIAN_POINT('',(0.092,0.159348674296337,0.04));
#44387=CARTESIAN_POINT('',(0.098937822173509,0.185365334794732,0.04));
#44388=CARTESIAN_POINT('',(0.092,0.159348674296337,0.04));
#44389=CARTESIAN_POINT('Origin',(0.092,0.159348674296337,0.04));
#44390=CARTESIAN_POINT('',(0.0963939408860592,0.163732123178242,0.185));
#44391=CARTESIAN_POINT('',(0.0963939408860592,0.163732123178242,0.0925));
#44392=CARTESIAN_POINT('',(0.092,0.159348674296337,0.191));
#44393=CARTESIAN_POINT('',(0.092,0.159348674296337,0.04));
#44394=CARTESIAN_POINT('Ctrl Pts',(0.0963939408860592,0.163732123178242,
0.185));
#44395=CARTESIAN_POINT('Ctrl Pts',(0.0941617249279218,0.161505237382642,
0.188051499118435));
#44396=CARTESIAN_POINT('Ctrl Pts',(0.092,0.159348674296337,0.191));
#44397=CARTESIAN_POINT('Origin',(0.098937822173509,0.185365334794732,0.04));
#44398=CARTESIAN_POINT('',(0.0935992076448906,0.165345663167344,0.185));
#44399=CARTESIAN_POINT('',(0.0935992076448906,0.165345663167344,0.0925));
#44400=CARTESIAN_POINT('Ctrl Pts',(0.092,0.159348674296337,0.191));
#44401=CARTESIAN_POINT('Ctrl Pts',(0.0927867759536358,0.162299064543034,
0.188051499118464));
#44402=CARTESIAN_POINT('Ctrl Pts',(0.0935992076448907,0.165345663167344,
0.185));
#44403=CARTESIAN_POINT('Origin',(0.126629159108248,0.150910755294439,0.04));
#44404=CARTESIAN_POINT('',(0.120889198458627,0.146580359175541,0.04));
#44405=CARTESIAN_POINT('',(0.123361285143431,0.144506032150084,0.04));
#44406=CARTESIAN_POINT('Origin',(0.,0.,0.04));
#44407=CARTESIAN_POINT('',(0.118272920182323,0.140952177533892,0.04));
#44408=CARTESIAN_POINT('',(0.12962308693234,0.165368846322791,0.04));
#44409=CARTESIAN_POINT('',(0.118272920182323,0.140952177533892,0.04));
#44410=CARTESIAN_POINT('Origin',(0.118272920182323,0.140952177533892,0.04));
#44411=CARTESIAN_POINT('',(0.123361285143431,0.144506032150084,0.185));
#44412=CARTESIAN_POINT('',(0.123361285143431,0.144506032150084,0.0925));
#44413=CARTESIAN_POINT('',(0.118272920182323,0.140952177533892,0.191));
#44414=CARTESIAN_POINT('',(0.118272920182323,0.140952177533892,0.04));
#44415=CARTESIAN_POINT('Ctrl Pts',(0.123361285143431,0.144506032150084,
0.185));
#44416=CARTESIAN_POINT('Ctrl Pts',(0.120776286901163,0.142700597986783,
0.188051499118455));
#44417=CARTESIAN_POINT('Ctrl Pts',(0.118272920182323,0.140952177533892,
0.191));
#44418=CARTESIAN_POINT('Origin',(0.12962308693234,0.165368846322791,0.04));
#44419=CARTESIAN_POINT('',(0.120889198458627,0.146580359175541,0.185));
#44420=CARTESIAN_POINT('',(0.120889198458627,0.146580359175541,0.0925));
#44421=CARTESIAN_POINT('Ctrl Pts',(0.118272920182323,0.140952177533892,
0.191));
#44422=CARTESIAN_POINT('Ctrl Pts',(0.119560073131097,0.14372112251268,0.188051499118454));
#44423=CARTESIAN_POINT('Ctrl Pts',(0.120889198458627,0.146580359175541,
0.185));
#44424=CARTESIAN_POINT('Origin',(0.150910755294439,0.126629159108248,0.04));
#44425=CARTESIAN_POINT('',(0.144506032150084,0.123361285143431,0.04));
#44426=CARTESIAN_POINT('',(0.146580359175541,0.120889198458627,0.04));
#44427=CARTESIAN_POINT('Origin',(0.,0.,0.04));
#44428=CARTESIAN_POINT('',(0.140952177533892,0.118272920182323,0.04));
#44429=CARTESIAN_POINT('',(0.15636981978718,0.140347709136006,0.04));
#44430=CARTESIAN_POINT('',(0.140952177533892,0.118272920182323,0.04));
#44431=CARTESIAN_POINT('Origin',(0.140952177533892,0.118272920182323,0.04));
#44432=CARTESIAN_POINT('',(0.146580359175541,0.120889198458627,0.185));
#44433=CARTESIAN_POINT('',(0.146580359175541,0.120889198458627,0.0925));
#44434=CARTESIAN_POINT('',(0.140952177533892,0.118272920182323,0.191));
#44435=CARTESIAN_POINT('',(0.140952177533892,0.118272920182323,0.04));
#44436=CARTESIAN_POINT('Ctrl Pts',(0.146580359175541,0.120889198458627,
0.185));
#44437=CARTESIAN_POINT('Ctrl Pts',(0.14372112251267,0.119560073131093,0.188051499118464));
#44438=CARTESIAN_POINT('Ctrl Pts',(0.140952177533892,0.118272920182323,
0.191));
#44439=CARTESIAN_POINT('Origin',(0.15636981978718,0.140347709136006,0.04));
#44440=CARTESIAN_POINT('',(0.144506032150084,0.123361285143431,0.185));
#44441=CARTESIAN_POINT('',(0.144506032150084,0.123361285143431,0.0925));
#44442=CARTESIAN_POINT('Ctrl Pts',(0.140952177533892,0.118272920182323,
0.191));
#44443=CARTESIAN_POINT('Ctrl Pts',(0.142700597986788,0.120776286901171,
0.188051499118446));
#44444=CARTESIAN_POINT('Ctrl Pts',(0.144506032150084,0.123361285143431,
0.185));
#44445=CARTESIAN_POINT('Origin',(0.170607004545534,0.0985,0.04));
#44446=CARTESIAN_POINT('',(0.163732123178242,0.0963939408860592,0.04));
#44447=CARTESIAN_POINT('',(0.165345663167344,0.0935992076448906,0.04));
#44448=CARTESIAN_POINT('Origin',(0.,0.,0.04));
#44449=CARTESIAN_POINT('',(0.159348674296337,0.092,0.04));
#44450=CARTESIAN_POINT('',(0.178365334794732,0.111062177826491,0.04));
#44451=CARTESIAN_POINT('',(0.159348674296337,0.092,0.04));
#44452=CARTESIAN_POINT('Origin',(0.159348674296337,0.092,0.04));
#44453=CARTESIAN_POINT('',(0.165345663167344,0.0935992076448906,0.185));
#44454=CARTESIAN_POINT('',(0.165345663167344,0.0935992076448906,0.0925));
#44455=CARTESIAN_POINT('',(0.159348674296337,0.092,0.191));
#44456=CARTESIAN_POINT('',(0.159348674296337,0.092,0.04));
#44457=CARTESIAN_POINT('Ctrl Pts',(0.165345663167344,0.0935992076448906,
0.185));
#44458=CARTESIAN_POINT('Ctrl Pts',(0.162299064543034,0.0927867759536356,
0.188051499118465));
#44459=CARTESIAN_POINT('Ctrl Pts',(0.159348674296337,0.092,0.191));
#44460=CARTESIAN_POINT('Origin',(0.178365334794732,0.111062177826491,0.04));
#44461=CARTESIAN_POINT('',(0.163732123178242,0.0963939408860592,0.185));
#44462=CARTESIAN_POINT('',(0.163732123178242,0.0963939408860592,0.0925));
#44463=CARTESIAN_POINT('Ctrl Pts',(0.159348674296337,0.092,0.191));
#44464=CARTESIAN_POINT('Ctrl Pts',(0.161505237382625,0.0941617249279039,
0.188051499118459));
#44465=CARTESIAN_POINT('Ctrl Pts',(0.163732123178242,0.0963939408860592,
0.185));
#44466=CARTESIAN_POINT('Origin',(0.185119446294824,0.0673779682351567,0.04));
#44467=CARTESIAN_POINT('',(0.17798329649608,0.0664977155125525,0.04));
#44468=CARTESIAN_POINT('',(0.179087022852749,0.0634652522703485,0.04));
#44469=CARTESIAN_POINT('Origin',(0.,0.,0.04));
#44470=CARTESIAN_POINT('',(0.172903442224607,0.062931706371923,0.04));
#44471=CARTESIAN_POINT('',(0.194941309361761,0.0784020784438918,0.04));
#44472=CARTESIAN_POINT('',(0.172903442224607,0.062931706371923,0.04));
#44473=CARTESIAN_POINT('Origin',(0.172903442224607,0.062931706371923,0.04));
#44474=CARTESIAN_POINT('',(0.179087022852749,0.0634652522703485,0.185));
#44475=CARTESIAN_POINT('',(0.179087022852749,0.0634652522703485,0.0925));
#44476=CARTESIAN_POINT('',(0.172903442224607,0.062931706371923,0.191));
#44477=CARTESIAN_POINT('',(0.172903442224607,0.062931706371923,0.04));
#44478=CARTESIAN_POINT('Ctrl Pts',(0.179087022852749,0.0634652522703485,
0.185));
#44479=CARTESIAN_POINT('Ctrl Pts',(0.175945631624537,0.0631941995412009,
0.188051499118474));
#44480=CARTESIAN_POINT('Ctrl Pts',(0.172903442224607,0.062931706371923,
0.191));
#44481=CARTESIAN_POINT('Origin',(0.194941309361761,0.0784020784438918,0.04));
#44482=CARTESIAN_POINT('',(0.17798329649608,0.0664977155125525,0.185));
#44483=CARTESIAN_POINT('',(0.17798329649608,0.0664977155125525,0.0925));
#44484=CARTESIAN_POINT('Ctrl Pts',(0.172903442224607,0.062931706371923,
0.191));
#44485=CARTESIAN_POINT('Ctrl Pts',(0.175402621866193,0.0646861065908464,
0.188051499118456));
#44486=CARTESIAN_POINT('Ctrl Pts',(0.17798329649608,0.0664977155125525,
0.185));
#44487=CARTESIAN_POINT('Origin',(0.194007127343405,0.0342086910003853,0.04));
#44488=CARTESIAN_POINT('',(0.186826537413779,0.0345809907026646,0.04));
#44489=CARTESIAN_POINT('',(0.18738691397118,0.0314029373205391,0.04));
#44490=CARTESIAN_POINT('Origin',(0.,0.,0.04));
#44491=CARTESIAN_POINT('',(0.181204626554246,0.0319512646907152,0.04));
#44492=CARTESIAN_POINT('',(0.205594090888895,0.0433597715811408,0.04));
#44493=CARTESIAN_POINT('',(0.181204626554246,0.0319512646907152,0.04));
#44494=CARTESIAN_POINT('Origin',(0.181204626554246,0.0319512646907152,0.04));
#44495=CARTESIAN_POINT('',(0.18738691397118,0.0314029373205391,0.185));
#44496=CARTESIAN_POINT('',(0.18738691397118,0.0314029373205391,0.0925));
#44497=CARTESIAN_POINT('',(0.181204626554246,0.0319512646907152,0.191));
#44498=CARTESIAN_POINT('',(0.181204626554246,0.0319512646907152,0.04));
#44499=CARTESIAN_POINT('Ctrl Pts',(0.18738691397118,0.0314029373205391,
0.185));
#44500=CARTESIAN_POINT('Ctrl Pts',(0.184246179721932,0.0316814993535165,
0.188051499118466));
#44501=CARTESIAN_POINT('Ctrl Pts',(0.181204626554246,0.0319512646907152,
0.191));
#44502=CARTESIAN_POINT('Origin',(0.205594090888895,0.0433597715811408,0.04));
#44503=CARTESIAN_POINT('',(0.186826537413779,0.0345809907026646,0.185));
#44504=CARTESIAN_POINT('',(0.186826537413779,0.0345809907026646,0.0925));
#44505=CARTESIAN_POINT('Ctrl Pts',(0.181204626554246,0.0319512646907152,
0.191));
#44506=CARTESIAN_POINT('Ctrl Pts',(0.183970486442399,0.0332450336377893,
0.18805149911842));
#44507=CARTESIAN_POINT('Ctrl Pts',(0.186826537413779,0.0345809907026646,
0.185));
#44508=CARTESIAN_POINT('Origin',(0.,0.,0.0925));
#44509=CARTESIAN_POINT('Origin',(0.,0.,0.185));
#44510=CARTESIAN_POINT('Origin',(0.,0.,0.185));
#44511=CARTESIAN_POINT('Origin',(0.,0.,0.185));
#44512=CARTESIAN_POINT('Origin',(0.,0.,0.185));
#44513=CARTESIAN_POINT('Origin',(0.,0.,0.185));
#44514=CARTESIAN_POINT('Origin',(0.,0.,0.185));
#44515=CARTESIAN_POINT('Origin',(0.,0.,0.185));
#44516=CARTESIAN_POINT('Origin',(0.,0.,0.185));
#44517=CARTESIAN_POINT('Origin',(0.,0.,0.185));
#44518=CARTESIAN_POINT('Origin',(0.,0.,0.185));
#44519=CARTESIAN_POINT('Origin',(0.,0.,0.185));
#44520=CARTESIAN_POINT('Origin',(0.,0.,0.185));
#44521=CARTESIAN_POINT('Origin',(0.,0.,0.185));
#44522=CARTESIAN_POINT('Origin',(0.,0.,0.185));
#44523=CARTESIAN_POINT('Origin',(0.,0.,0.185));
#44524=CARTESIAN_POINT('Origin',(0.,0.,0.185));
#44525=CARTESIAN_POINT('Origin',(0.,0.,0.185));
#44526=CARTESIAN_POINT('',(-0.19,-2.32682891837997E-17,0.));
#44527=CARTESIAN_POINT('',(-0.19,-2.32682891837997E-17,0.0925));
#44528=CARTESIAN_POINT('Origin',(0.,0.,0.));
#44529=CARTESIAN_POINT('Origin',(0.,0.,0.185));
#44530=CARTESIAN_POINT('Origin',(0.,0.,0.185));
#44531=CARTESIAN_POINT('Origin',(0.,0.,0.185));
#44532=CARTESIAN_POINT('Origin',(0.,0.,0.185));
#44533=CARTESIAN_POINT('Origin',(0.,0.,0.185));
#44534=CARTESIAN_POINT('Origin',(0.,0.,0.185));
#44535=CARTESIAN_POINT('Origin',(0.,0.,0.185));
#44536=CARTESIAN_POINT('Origin',(0.,0.,0.185));
#44537=CARTESIAN_POINT('Origin',(0.,0.,0.185));
#44538=CARTESIAN_POINT('Origin',(0.,0.,0.185));
#44539=CARTESIAN_POINT('Origin',(0.,0.,0.185));
#44540=CARTESIAN_POINT('Origin',(0.,0.,0.185));
#44541=CARTESIAN_POINT('Origin',(0.,0.,0.185));
#44542=CARTESIAN_POINT('Origin',(0.,0.,0.185));
#44543=CARTESIAN_POINT('Origin',(0.,0.,0.185));
#44544=CARTESIAN_POINT('Origin',(0.,0.,0.185));
#44545=CARTESIAN_POINT('Origin',(0.,0.,0.185));
#44546=CARTESIAN_POINT('',(0.18999314853095,0.00161353998910188,0.185));
#44547=CARTESIAN_POINT('Origin',(0.,0.,0.185));
#44548=CARTESIAN_POINT('',(0.18999314853095,0.00161353998910188,0.04));
#44549=CARTESIAN_POINT('',(0.18999314853095,0.00161353998910188,0.0925));
#44550=CARTESIAN_POINT('',(0.18999314853095,-0.00161353998910189,0.04));
#44551=CARTESIAN_POINT('Origin',(0.,0.,0.04));
#44552=CARTESIAN_POINT('',(0.18999314853095,-0.00161353998910189,0.185));
#44553=CARTESIAN_POINT('',(0.18999314853095,-0.00161353998910189,0.0925));
#44554=CARTESIAN_POINT('Origin',(0.,0.,0.185));
#44555=CARTESIAN_POINT('Origin',(0.184,0.,0.04));
#44556=CARTESIAN_POINT('',(0.184,0.,0.04));
#44557=CARTESIAN_POINT('',(0.184,0.,0.04));
#44558=CARTESIAN_POINT('',(0.184,0.,0.191));
#44559=CARTESIAN_POINT('',(0.184,0.,0.04));
#44560=CARTESIAN_POINT('Ctrl Pts',(0.18999314853095,-0.00161353998910188,
0.185));
#44561=CARTESIAN_POINT('Ctrl Pts',(0.186948500881579,-0.000793827160425129,
0.188051499118421));
#44562=CARTESIAN_POINT('Ctrl Pts',(0.184,0.,0.191));
#44563=CARTESIAN_POINT('Origin',(0.21,0.007,0.04));
#44564=CARTESIAN_POINT('Ctrl Pts',(0.184,0.,0.191));
#44565=CARTESIAN_POINT('Ctrl Pts',(0.1869485008816,0.000793827160430761,
0.1880514991184));
#44566=CARTESIAN_POINT('Ctrl Pts',(0.18999314853095,0.00161353998910188,
0.185));
#44567=CARTESIAN_POINT('',(0.21,0.007,0.04));
#44568=CARTESIAN_POINT('Origin',(0.197,0.,0.04));
#44569=CARTESIAN_POINT('Origin',(0.,0.,0.1925));
#44570=CARTESIAN_POINT('',(-0.175,-2.14313189850787E-17,0.2));
#44571=CARTESIAN_POINT('Origin',(0.,0.,0.2));
#44572=CARTESIAN_POINT('',(-0.1825,-2.23498040844392E-17,0.1925));
#44573=CARTESIAN_POINT('Origin',(0.,0.,0.078849364905389));
#44574=CARTESIAN_POINT('',(0.,0.,0.0566987298107781));
#44575=CARTESIAN_POINT('',(-0.0677181486487011,8.29308139868164E-18,0.1));
#44576=CARTESIAN_POINT('',(-0.0346410161513776,-4.24230095489963E-18,0.078849364905389));
#44577=CARTESIAN_POINT('Origin',(0.,0.,0.1));
#44578=CARTESIAN_POINT('Origin',(0.,0.0866025403784439,0.2));
#44579=CARTESIAN_POINT('',(5.30287619362453E-18,0.0866025403784439,0.2));
#44580=CARTESIAN_POINT('',(0.075,0.0433012701892219,0.2));
#44581=CARTESIAN_POINT('',(0.01875,0.0757772228311384,0.2));
#44582=CARTESIAN_POINT('',(0.,0.0866025403784439,0.1));
#44583=CARTESIAN_POINT('',(5.30287619362453E-18,0.0866025403784439,0.2));
#44584=CARTESIAN_POINT('',(0.075,0.0433012701892219,0.1));
#44585=CARTESIAN_POINT('',(0.075,0.0433012701892219,0.1));
#44586=CARTESIAN_POINT('',(0.075,0.0433012701892219,0.2));
#44587=CARTESIAN_POINT('Origin',(-0.075,0.0433012701892219,0.2));
#44588=CARTESIAN_POINT('',(-0.075,0.0433012701892219,0.2));
#44589=CARTESIAN_POINT('',(-0.05625,0.0541265877365274,0.2));
#44590=CARTESIAN_POINT('',(-0.075,0.0433012701892219,0.1));
#44591=CARTESIAN_POINT('',(-0.075,0.0433012701892219,0.2));
#44592=CARTESIAN_POINT('',(5.30287619362453E-18,0.0866025403784439,0.1));
#44593=CARTESIAN_POINT('Origin',(-0.075,-0.0433012701892219,0.2));
#44594=CARTESIAN_POINT('',(-0.075,-0.0433012701892219,0.2));
#44595=CARTESIAN_POINT('',(-0.075,-0.021650635094611,0.2));
#44596=CARTESIAN_POINT('',(-0.075,-0.0433012701892219,0.1));
#44597=CARTESIAN_POINT('',(-0.075,-0.0433012701892219,0.2));
#44598=CARTESIAN_POINT('',(-0.075,0.0433012701892219,0.1));
#44599=CARTESIAN_POINT('Origin',(-1.38777878078145E-17,-0.0866025403784439,
0.2));
#44600=CARTESIAN_POINT('',(-1.59086285808736E-17,-0.0866025403784439,0.2));
#44601=CARTESIAN_POINT('',(-0.01875,-0.0757772228311384,0.2));
#44602=CARTESIAN_POINT('',(-1.38777878078145E-17,-0.0866025403784439,0.1));
#44603=CARTESIAN_POINT('',(-1.59086285808736E-17,-0.0866025403784439,0.2));
#44604=CARTESIAN_POINT('',(-0.075,-0.0433012701892219,0.1));
#44605=CARTESIAN_POINT('Origin',(0.075,-0.043301270189222,0.2));
#44606=CARTESIAN_POINT('',(0.075,-0.043301270189222,0.2));
#44607=CARTESIAN_POINT('',(0.05625,-0.0541265877365275,0.2));
#44608=CARTESIAN_POINT('',(0.075,-0.043301270189222,0.1));
#44609=CARTESIAN_POINT('',(0.075,-0.043301270189222,0.2));
#44610=CARTESIAN_POINT('',(-1.59086285808736E-17,-0.0866025403784439,0.1));
#44611=CARTESIAN_POINT('Origin',(0.075,0.0433012701892219,0.2));
#44612=CARTESIAN_POINT('',(0.075,0.021650635094611,0.2));
#44613=CARTESIAN_POINT('',(0.075,-0.043301270189222,0.1));
#44614=CARTESIAN_POINT('Origin',(0.,0.,0.1));
#44615=CARTESIAN_POINT('Origin',(0.076,0.,-1.2));
#44616=CARTESIAN_POINT('',(-0.076,-9.30731567351988E-18,-1.2));
#44617=CARTESIAN_POINT('Origin',(0.,0.,-1.2));
#44618=CARTESIAN_POINT('Origin',(0.,0.,-1.188));
#44619=CARTESIAN_POINT('',(-0.088,-1.07768918324967E-17,-1.188));
#44620=CARTESIAN_POINT('Origin',(0.,0.,-0.593));
#44621=CARTESIAN_POINT('Origin',(0.,0.,-0.013325));
#44622=CARTESIAN_POINT('Origin',(0.,0.,-0.005));
#44623=CARTESIAN_POINT('',(-0.11,-1.34711147906209E-17,-3.46944695195361E-18));
#44624=CARTESIAN_POINT('Origin',(0.,0.,0.));
#44625=CARTESIAN_POINT('',(-0.105,-1.28587913910472E-17,-0.005));
#44626=CARTESIAN_POINT('Origin',(0.19,0.,0.));
#44627=CARTESIAN_POINT('Origin',(0.,0.,0.2));
#44628=CARTESIAN_POINT('',(0.,0.,0.));
#44629=CARTESIAN_POINT('Origin',(0.,0.,-0.493));
#44630=CARTESIAN_POINT('',(-0.0966111239073705,-8.03799554811163E-5,-0.926426408311032));
#44631=CARTESIAN_POINT('',(-0.0966191160461945,-8.04235544959989E-5,-0.932223591688968));
#44632=CARTESIAN_POINT('',(-0.096675,-1.1839272930757E-17,-0.493));
#44633=CARTESIAN_POINT('',(0.0869479092309507,-0.0426124462865253,-0.949325));
#44634=CARTESIAN_POINT('Ctrl Pts',(-0.0966111239073705,-8.03799554811163E-5,
-0.926426408311032));
#44635=CARTESIAN_POINT('Ctrl Pts',(-0.0964350902968673,0.0222712561995875,
-0.927896221307833));
#44636=CARTESIAN_POINT('Ctrl Pts',(-0.0887114911241552,0.044734022366812,
-0.929366034304633));
#44637=CARTESIAN_POINT('Ctrl Pts',(-0.0745208699991529,0.0618333618915069,
-0.930835847301434));
#44638=CARTESIAN_POINT('Ctrl Pts',(-0.0541569551612004,0.0863713641959035,
-0.932945067640058));
#44639=CARTESIAN_POINT('Ctrl Pts',(-0.0204754984960076,0.0998644590952887,
-0.935054287978682));
#44640=CARTESIAN_POINT('Ctrl Pts',(0.0111920394192712,0.0961816327255734,
-0.937163508317306));
#44641=CARTESIAN_POINT('Ctrl Pts',(0.0428595773345502,0.0924988063558581,
-0.93927272865593));
#44642=CARTESIAN_POINT('Ctrl Pts',(0.0725131964999154,0.0716400587170422,
-0.941381948994554));
#44643=CARTESIAN_POINT('Ctrl Pts',(0.0867090407236772,0.0430821191108494,
-0.943491169333178));
#44644=CARTESIAN_POINT('Ctrl Pts',(0.0997969971053929,0.0167529299463267,
-0.945435779555452));
#44645=CARTESIAN_POINT('Ctrl Pts',(0.0997457751378415,-0.0161206070811178,
-0.947380389777726));
#44646=CARTESIAN_POINT('Ctrl Pts',(0.0869479092309507,-0.0426124462865253,
-0.949325));
#44647=CARTESIAN_POINT('',(-0.096675,-1.1839272930757E-17,-0.949325));
#44648=CARTESIAN_POINT('Origin',(0.,0.,-0.949325));
#44649=CARTESIAN_POINT('',(-0.096675,-1.1839272930757E-17,-0.979325));
#44650=CARTESIAN_POINT('',(-0.096675,-1.1839272930757E-17,-0.493));
#44651=CARTESIAN_POINT('Origin',(0.,0.,-0.979325));
#44652=CARTESIAN_POINT('',(0.0868262223680489,0.042511912851507,-0.949325));
#44653=CARTESIAN_POINT('Origin',(0.,0.,-0.949325));
#44654=CARTESIAN_POINT('Ctrl Pts',(0.0868262223680489,0.042511912851507,
-0.949325));
#44655=CARTESIAN_POINT('Ctrl Pts',(0.0727413643237034,0.0712787909934627,
-0.947215779661376));
#44656=CARTESIAN_POINT('Ctrl Pts',(0.0433671481397557,0.0922558111466541,
-0.945106559322752));
#44657=CARTESIAN_POINT('Ctrl Pts',(0.0117674690472282,0.0961065728543937,
-0.942997338984128));
#44658=CARTESIAN_POINT('Ctrl Pts',(-0.0198322100452994,0.0999573345621333,
-0.940888118645504));
#44659=CARTESIAN_POINT('Ctrl Pts',(-0.0536573520464067,0.0866818378244212,
-0.938778898306881));
#44660=CARTESIAN_POINT('Ctrl Pts',(-0.0741790245420598,0.0622672145784177,
-0.936669677968257));
#44661=CARTESIAN_POINT('Ctrl Pts',(-0.0885984326427958,0.0451124521542337,
-0.935187649208494));
#44662=CARTESIAN_POINT('Ctrl Pts',(-0.0964498235569402,0.022458224021493,
-0.933705620448731));
#44663=CARTESIAN_POINT('Ctrl Pts',(-0.0966191160461945,-8.04235544959989E-5,
-0.932223591688968));
#44664=CARTESIAN_POINT('Origin',(0.,0.,-0.493));
#44665=CARTESIAN_POINT('',(-0.0968293357490093,1.06988599727479E-5,-0.886426408311032));
#44666=CARTESIAN_POINT('',(-0.0968280577919496,1.39804010291189E-5,-0.892223591688968));
#44667=CARTESIAN_POINT('',(-0.096675,-1.1839272930757E-17,-0.493));
#44668=CARTESIAN_POINT('Ctrl Pts',(-0.0968293357490093,1.06988599727479E-5,
-0.886426408311032));
#44669=CARTESIAN_POINT('Ctrl Pts',(-0.0968302582891165,0.00059431625353822,
-0.886465012270798));
#44670=CARTESIAN_POINT('Ctrl Pts',(-0.096825435141126,0.00117791800451826,
-0.886503616230564));
#44671=CARTESIAN_POINT('Ctrl Pts',(-0.0968148197274314,0.00176141437737019,
-0.88654222019033));
#44672=CARTESIAN_POINT('Ctrl Pts',(-0.0962348210277351,0.0336421443489341,
-0.888651440528954));
#44673=CARTESIAN_POINT('Ctrl Pts',(-0.0783634816289883,0.0652082946364147,
-0.890760660867579));
#44674=CARTESIAN_POINT('Ctrl Pts',(-0.0513251420952661,0.0821094183977308,
-0.892869881206202));
#44675=CARTESIAN_POINT('Ctrl Pts',(-0.0242868025615438,0.0990105421590469,
-0.894979101544826));
#44676=CARTESIAN_POINT('Ctrl Pts',(0.0119185371071539,0.101246639394198,
-0.89708832188345));
#44677=CARTESIAN_POINT('Ctrl Pts',(0.0408310098562432,0.0878012164778136,
-0.899197542222074));
#44678=CARTESIAN_POINT('Ctrl Pts',(0.0697434826053325,0.074355793561429,
-0.901306762560698));
#44679=CARTESIAN_POINT('Ctrl Pts',(0.0913630884348138,0.0452288504935087,
-0.903415982899322));
#44680=CARTESIAN_POINT('Ctrl Pts',(0.0958620419187354,0.0136617734053438,
-0.905525203237946));
#44681=CARTESIAN_POINT('Ctrl Pts',(0.100360995402657,-0.017905303682821,
-0.90763442357657));
#44682=CARTESIAN_POINT('Ctrl Pts',(0.087739296541019,-0.0519125147912303,
-0.909743643915194));
#44683=CARTESIAN_POINT('Ctrl Pts',(0.0637334499829788,-0.0728994661690192,
-0.911852864253818));
#44684=CARTESIAN_POINT('Ctrl Pts',(0.0397276034249385,-0.0938864175468081,
-0.913962084592442));
#44685=CARTESIAN_POINT('Ctrl Pts',(0.00433760917049605,-0.101853109193976,
-0.916071304931066));
#44686=CARTESIAN_POINT('Ctrl Pts',(-0.0263449122524892,-0.0931782315159874,
-0.91818052526969));
#44687=CARTESIAN_POINT('Ctrl Pts',(-0.0570274336754744,-0.0845033538379983,
-0.920289745608314));
#44688=CARTESIAN_POINT('Ctrl Pts',(-0.0830024822670023,-0.0591869068348518,
-0.922398965946938));
#44689=CARTESIAN_POINT('Ctrl Pts',(-0.0924668200574101,-0.0287372284785746,
-0.924508186285562));
#44690=CARTESIAN_POINT('Ctrl Pts',(-0.0953359214774314,-0.0195064489622592,
-0.925147593627386));
#44691=CARTESIAN_POINT('Ctrl Pts',(-0.0966877031614718,-0.00980393001962354,
-0.925787000969209));
#44692=CARTESIAN_POINT('Ctrl Pts',(-0.0966111239073705,-8.03799554811163E-5,
-0.926426408311032));
#44693=CARTESIAN_POINT('Ctrl Pts',(-0.0966191160461945,-8.04235544959989E-5,
-0.932223591688968));
#44694=CARTESIAN_POINT('Ctrl Pts',(-0.0966907602858392,-0.00961873370229752,
-0.931596400110107));
#44695=CARTESIAN_POINT('Ctrl Pts',(-0.0953865673460834,-0.0191363437733232,
-0.930969208531246));
#44696=CARTESIAN_POINT('Ctrl Pts',(-0.0926220973441531,-0.0282076709356274,
-0.930342016952384));
#44697=CARTESIAN_POINT('Ctrl Pts',(-0.0833252946603945,-0.0587141834493743,
-0.92823279661376));
#44698=CARTESIAN_POINT('Ctrl Pts',(-0.0575134863026783,-0.0841734587225733,
-0.926123576275137));
#44699=CARTESIAN_POINT('Ctrl Pts',(-0.0268854626848309,-0.0930233302060816,
-0.924014355936513));
#44700=CARTESIAN_POINT('Ctrl Pts',(0.00374256093301658,-0.10187320168959,
-0.921905135597888));
#44701=CARTESIAN_POINT('Ctrl Pts',(0.0391867998109952,-0.0941136693834075,
-0.919795915259264));
#44702=CARTESIAN_POINT('Ctrl Pts',(0.063315182280828,-0.0732660374240845,
-0.91768669492064));
#44703=CARTESIAN_POINT('Ctrl Pts',(0.0874435647506607,-0.0524184054647615,
-0.915577474582016));
#44704=CARTESIAN_POINT('Ctrl Pts',(0.100256090812348,-0.018482673852298,
-0.913468254243393));
#44705=CARTESIAN_POINT('Ctrl Pts',(0.0959378107493762,0.0131101896102531,
-0.911359033904769));
#44706=CARTESIAN_POINT('Ctrl Pts',(0.0916195306864047,0.0447030530728043,
-0.909249813566145));
#44707=CARTESIAN_POINT('Ctrl Pts',(0.0701704444987747,0.0739530483854431,
-0.90714059322752));
#44708=CARTESIAN_POINT('Ctrl Pts',(0.0413364389978215,0.087564466214271,
-0.905031372888896));
#44709=CARTESIAN_POINT('Ctrl Pts',(0.0125024334968684,0.101175884043099,
-0.902922152550272));
#44710=CARTESIAN_POINT('Ctrl Pts',(-0.0237164913174078,0.0991487243881159,
-0.900812932211648));
#44711=CARTESIAN_POINT('Ctrl Pts',(-0.0508519843711625,0.0824036418801622,
-0.898703711873024));
#44712=CARTESIAN_POINT('Ctrl Pts',(-0.0779874774249174,0.0656585593722084,
-0.896594491534401));
#44713=CARTESIAN_POINT('Ctrl Pts',(-0.0960395387181506,0.0341955540112833,
-0.894485271195776));
#44714=CARTESIAN_POINT('Ctrl Pts',(-0.0968028858565612,0.00231863128268832,
-0.892376050857152));
#44715=CARTESIAN_POINT('Ctrl Pts',(-0.0968212780032749,0.00155058616913002,
-0.892325231134424));
#44716=CARTESIAN_POINT('Ctrl Pts',(-0.0968296336248802,0.000782300766327763,
-0.892274411411696));
#44717=CARTESIAN_POINT('Ctrl Pts',(-0.0968280577919496,1.39804010291189E-5,
-0.892223591688968));
#44718=CARTESIAN_POINT('Origin',(0.,0.,-0.493));
#44719=CARTESIAN_POINT('',(-0.0965815334425764,7.1292991562881E-5,-0.846426408311032));
#44720=CARTESIAN_POINT('',(-0.0965773242360877,6.95087071336693E-5,-0.852223591688968));
#44721=CARTESIAN_POINT('',(-0.096675,-1.1839272930757E-17,-0.493));
#44722=CARTESIAN_POINT('Ctrl Pts',(-0.0965815334425764,7.1292991562881E-5,
-0.846426408311032));
#44723=CARTESIAN_POINT('Ctrl Pts',(-0.096656839197146,0.0109770781310021,
-0.847143023572388));
#44724=CARTESIAN_POINT('Ctrl Pts',(-0.0949511484573878,0.0218600075058422,
-0.847859638833743));
#44725=CARTESIAN_POINT('Ctrl Pts',(-0.091361885510168,0.0320815246121575,
-0.848576254095099));
#44726=CARTESIAN_POINT('Ctrl Pts',(-0.080797574620909,0.0621666106197558,
-0.850685474433722));
#44727=CARTESIAN_POINT('Ctrl Pts',(-0.0539157469163047,0.0865218362212725,
-0.852794694772346));
#44728=CARTESIAN_POINT('Ctrl Pts',(-0.0229372507921025,0.0940749760435912,
-0.854903915110971));
#44729=CARTESIAN_POINT('Ctrl Pts',(0.00804124533209912,0.10162811586591,
-0.857013135449595));
#44730=CARTESIAN_POINT('Ctrl Pts',(0.0431164098758985,0.092379169909031,
-0.859122355788219));
#44731=CARTESIAN_POINT('Ctrl Pts',(0.0663425758270414,0.0705328392060976,
-0.861231576126843));
#44732=CARTESIAN_POINT('Ctrl Pts',(0.0895687417781846,0.0486865085031638,
-0.863340796465467));
#44733=CARTESIAN_POINT('Ctrl Pts',(0.100945909136671,0.0142427930541751,
-0.86545001680409));
#44734=CARTESIAN_POINT('Ctrl Pts',(0.0953018761651522,-0.0171397173428181,
-0.867559237142714));
#44735=CARTESIAN_POINT('Ctrl Pts',(0.0896578431936334,-0.0485222277398107,
-0.869668457481338));
#44736=CARTESIAN_POINT('Ctrl Pts',(0.06699260989211,-0.0768435330848077,
-0.871777677819963));
#44737=CARTESIAN_POINT('Ctrl Pts',(0.037610074738181,-0.0892283685032535,
-0.873886898158587));
#44738=CARTESIAN_POINT('Ctrl Pts',(0.00822753958425157,-0.101613203921699,
-0.875996118497211));
#44739=CARTESIAN_POINT('Ctrl Pts',(-0.0278722974220837,-0.0980615694135937,
-0.878105338835835));
#44740=CARTESIAN_POINT('Ctrl Pts',(-0.0542778869249285,-0.0801880973317172,
-0.880214559174458));
#44741=CARTESIAN_POINT('Ctrl Pts',(-0.0802001886952881,-0.0626417540872089,
-0.882285175553316));
#44742=CARTESIAN_POINT('Ctrl Pts',(-0.0967798530879647,-0.0312930259762486,
-0.884355791932174));
#44743=CARTESIAN_POINT('Ctrl Pts',(-0.0968293357490093,1.06988599727479E-5,
-0.886426408311032));
#44744=CARTESIAN_POINT('Ctrl Pts',(-0.0968280577919496,1.39804010291189E-5,
-0.892223591688968));
#44745=CARTESIAN_POINT('Ctrl Pts',(-0.0967642302993774,-0.0311060460027344,
-0.890165191073072));
#44746=CARTESIAN_POINT('Ctrl Pts',(-0.080407139247537,-0.0622834308897126,
-0.888106790457176));
#44747=CARTESIAN_POINT('Ctrl Pts',(-0.0547386896099341,-0.0798742794120905,
-0.886048389841281));
#44748=CARTESIAN_POINT('Ctrl Pts',(-0.028436513241308,-0.0978994272820098,
-0.883939169502657));
#44749=CARTESIAN_POINT('Ctrl Pts',(0.00764247247953262,-0.101658882925584,
-0.881829949164033));
#44750=CARTESIAN_POINT('Ctrl Pts',(0.0370958592149572,-0.0894434105834474,
-0.879720728825409));
#44751=CARTESIAN_POINT('Ctrl Pts',(0.0665492459503818,-0.0772279382413112,
-0.877611508486785));
#44752=CARTESIAN_POINT('Ctrl Pts',(0.0893770337003904,-0.0490375379134651,
-0.87550228814816));
#44753=CARTESIAN_POINT('Ctrl Pts',(0.0952016028206863,-0.0176880291495755,
-0.873393067809536));
#44754=CARTESIAN_POINT('Ctrl Pts',(0.101026171940982,0.0136614796143141,
-0.871283847470913));
#44755=CARTESIAN_POINT('Ctrl Pts',(0.089847522431565,0.0481700968142471,
-0.869174627132289));
#44756=CARTESIAN_POINT('Ctrl Pts',(0.0667475130189973,0.0701497621673904,
-0.867065406793665));
#44757=CARTESIAN_POINT('Ctrl Pts',(0.0436475036064297,0.0921294275205335,
-0.864956186455041));
#44758=CARTESIAN_POINT('Ctrl Pts',(0.00862613429071169,0.101580141026887,
-0.862846966116416));
#44759=CARTESIAN_POINT('Ctrl Pts',(-0.0223953343972411,0.09420545699243,
-0.860737745777792));
#44760=CARTESIAN_POINT('Ctrl Pts',(-0.053416803085194,0.0868307729579728,
-0.858628525439168));
#44761=CARTESIAN_POINT('Ctrl Pts',(-0.0804383711453816,0.0626306913827048,
-0.856519305100545));
#44762=CARTESIAN_POINT('Ctrl Pts',(-0.0911756884108397,0.0326069166667885,
-0.854410084761921));
#44763=CARTESIAN_POINT('Ctrl Pts',(-0.0948859171611054,0.0222323445657248,
-0.853681253737604));
#44764=CARTESIAN_POINT('Ctrl Pts',(-0.0966517818572679,0.0111624147385034,
-0.852952422713286));
#44765=CARTESIAN_POINT('Ctrl Pts',(-0.0965773242360877,6.95087071336693E-5,
-0.852223591688968));
#44766=CARTESIAN_POINT('Origin',(0.,0.,-0.493));
#44767=CARTESIAN_POINT('',(-0.0965822410032082,-7.15798389840372E-5,-0.806426408311033));
#44768=CARTESIAN_POINT('',(-0.0965865764190601,-7.32614358284168E-5,-0.812223591688968));
#44769=CARTESIAN_POINT('',(-0.096675,-1.1839272930757E-17,-0.493));
#44770=CARTESIAN_POINT('Ctrl Pts',(-0.0965822410032082,-7.15798389840372E-5,
-0.806426408311033));
#44771=CARTESIAN_POINT('Ctrl Pts',(-0.0964350243461911,0.021152105978162,
-0.807821034873977));
#44772=CARTESIAN_POINT('Ctrl Pts',(-0.0895412391802931,0.0424627517956176,
-0.809215661436921));
#44773=CARTESIAN_POINT('Ctrl Pts',(-0.0766614365121771,0.0591543965841834,
-0.810610287999866));
#44774=CARTESIAN_POINT('Ctrl Pts',(-0.0571821418630841,0.0843986860653691,
-0.81271950833849));
#44775=CARTESIAN_POINT('Ctrl Pts',(-0.0240108747313753,0.0990778151604882,
-0.814828728677115));
#44776=CARTESIAN_POINT('Ctrl Pts',(0.00777224516368064,0.096518447416171,
-0.816937949015739));
#44777=CARTESIAN_POINT('Ctrl Pts',(0.0395553650587365,0.0939590796718537,
-0.819047169354363));
#44778=CARTESIAN_POINT('Ctrl Pts',(0.0699503377171397,0.0741612150881001,
-0.821156389692986));
#44779=CARTESIAN_POINT('Ctrl Pts',(0.0851391852437711,0.0461252385447729,
-0.82326561003161));
#44780=CARTESIAN_POINT('Ctrl Pts',(0.100328032770402,0.0180892620014455,
-0.825374830370234));
#44781=CARTESIAN_POINT('Ctrl Pts',(0.100310755165262,-0.0181848265014556,
-0.827484050708859));
#44782=CARTESIAN_POINT('Ctrl Pts',(0.0850952074316202,-0.0462063214123137,
-0.829593271047483));
#44783=CARTESIAN_POINT('Ctrl Pts',(0.0698796596979782,-0.0742278163231718,
-0.831702491386107));
#44784=CARTESIAN_POINT('Ctrl Pts',(0.0394658418358345,-0.0939967176419867,
-0.833811711724731));
#44785=CARTESIAN_POINT('Ctrl Pts',(0.00768029815127167,-0.096525807511727,
-0.835920932063354));
#44786=CARTESIAN_POINT('Ctrl Pts',(-0.0241052455332914,-0.0990548973814673,
-0.838030152401978));
#44787=CARTESIAN_POINT('Ctrl Pts',(-0.0572625150402736,-0.0843441758021326,
-0.840139372740602));
#44788=CARTESIAN_POINT('Ctrl Pts',(-0.0767177527568075,-0.0590813418056254,
-0.842248593079227));
#44789=CARTESIAN_POINT('Ctrl Pts',(-0.0895630028842492,-0.0424016473016928,
-0.843641198156495));
#44790=CARTESIAN_POINT('Ctrl Pts',(-0.0964351910719676,-0.0211220203186491,
-0.845033803233764));
#44791=CARTESIAN_POINT('Ctrl Pts',(-0.0965815334425764,7.1292991562881E-5,
-0.846426408311032));
#44792=CARTESIAN_POINT('Ctrl Pts',(-0.0965773242360877,6.95087071336693E-5,
-0.852223591688968));
#44793=CARTESIAN_POINT('Ctrl Pts',(-0.0964363032021079,-0.0209402019657099,
-0.850843202374662));
#44794=CARTESIAN_POINT('Ctrl Pts',(-0.0896937709124859,-0.042032331717466,
-0.849462813060355));
#44795=CARTESIAN_POINT('Ctrl Pts',(-0.0770565847627674,-0.0586387344727256,
-0.848082423746049));
#44796=CARTESIAN_POINT('Ctrl Pts',(-0.0577470973785083,-0.084013143039759,
-0.845973203407424));
#44797=CARTESIAN_POINT('Ctrl Pts',(-0.0246750561392616,-0.0989144923172608,
-0.843863983068801));
#44798=CARTESIAN_POINT('Ctrl Pts',(0.00712452003262372,-0.0965684185823616,
-0.841754762730177));
#44799=CARTESIAN_POINT('Ctrl Pts',(0.0389240962045089,-0.0942223448474623,
-0.839645542391553));
#44800=CARTESIAN_POINT('Ctrl Pts',(0.0694512073090326,-0.0746288481001618,
-0.837536322052929));
#44801=CARTESIAN_POINT('Ctrl Pts',(0.0848278081861491,-0.0466954062534146,
-0.835427101714305));
#44802=CARTESIAN_POINT('Ctrl Pts',(0.100204409063266,-0.0187619644066672,
-0.833317881375681));
#44803=CARTESIAN_POINT('Ctrl Pts',(0.100430499712975,0.0175114225395272,
-0.831208661037057));
#44804=CARTESIAN_POINT('Ctrl Pts',(0.0854032937950573,0.0456343687175503,
-0.829099440698433));
#44805=CARTESIAN_POINT('Ctrl Pts',(0.0703760878771397,0.0737573148955733,
-0.826990220359809));
#44806=CARTESIAN_POINT('Ctrl Pts',(0.0400955853915954,0.0937298203054251,
-0.824881000021185));
#44807=CARTESIAN_POINT('Ctrl Pts',(0.00832772556442014,0.0964721055228851,
-0.822771779682561));
#44808=CARTESIAN_POINT('Ctrl Pts',(-0.023440134262755,0.0992143907403452,
-0.820662559343937));
#44809=CARTESIAN_POINT('Ctrl Pts',(-0.0566953514315609,0.0847264557654135,
-0.818553339005313));
#44810=CARTESIAN_POINT('Ctrl Pts',(-0.0763196419287051,0.0595947177503087,
-0.816444118666689));
#44811=CARTESIAN_POINT('Ctrl Pts',(-0.08940897260778,0.0428319395256663,
-0.815037276340782));
#44812=CARTESIAN_POINT('Ctrl Pts',(-0.0964341198149447,0.0213339018407355,
-0.813630434014875));
#44813=CARTESIAN_POINT('Ctrl Pts',(-0.0965865764190601,-7.32614358284168E-5,
-0.812223591688968));
#44814=CARTESIAN_POINT('Origin',(0.,0.,-0.493));
#44815=CARTESIAN_POINT('',(-0.0968295223683655,-1.01472914774969E-5,-0.766426408311033));
#44816=CARTESIAN_POINT('',(-0.0968302674661193,-6.76949675972993E-6,-0.772223591688968));
#44817=CARTESIAN_POINT('',(-0.096675,-1.1839272930757E-17,-0.493));
#44818=CARTESIAN_POINT('Ctrl Pts',(-0.0968295223683655,-1.01472914774969E-5,
-0.766426408311033));
#44819=CARTESIAN_POINT('Ctrl Pts',(-0.0967824824364324,0.0313240025753763,
-0.768499046175567));
#44820=CARTESIAN_POINT('Ctrl Pts',(-0.0801658005353392,0.0627010190930274,
-0.7705716840401));
#44821=CARTESIAN_POINT('Ctrl Pts',(-0.0542014570286708,0.0802397690797426,
-0.772644321904635));
#44822=CARTESIAN_POINT('Ctrl Pts',(-0.0277788376505428,0.0980880815220773,
-0.774753542243259));
#44823=CARTESIAN_POINT('Ctrl Pts',(0.00832433161131209,0.101605320043514,
-0.776862762581884));
#44824=CARTESIAN_POINT('Ctrl Pts',(0.0376950474149603,0.0891924990478497,
-0.778971982920508));
#44825=CARTESIAN_POINT('Ctrl Pts',(0.067065763218609,0.0767796780521847,
-0.781081203259132));
#44826=CARTESIAN_POINT('Ctrl Pts',(0.0897040255640509,0.0484367975394173,
-0.783190423597755));
#44827=CARTESIAN_POINT('Ctrl Pts',(0.0953181652342701,0.0170489255568315,
-0.785299643936379));
#44828=CARTESIAN_POINT('Ctrl Pts',(0.100932304904489,-0.0143389464257542,
-0.787408864275003));
#44829=CARTESIAN_POINT('Ctrl Pts',(0.0895223218994858,-0.0487718098781582,
-0.789518084613627));
#44830=CARTESIAN_POINT('Ctrl Pts',(0.0662753533412323,-0.0705960057310972,
-0.791627304952251));
#44831=CARTESIAN_POINT('Ctrl Pts',(0.0430283847829787,-0.0924202015840362,
-0.793736525290875));
#44832=CARTESIAN_POINT('Ctrl Pts',(0.007944430671475,-0.10163572983751,
-0.795845745629498));
#44833=CARTESIAN_POINT('Ctrl Pts',(-0.0230268550599761,-0.0940530830543341,
-0.797954965968123));
#44834=CARTESIAN_POINT('Ctrl Pts',(-0.0539981407914274,-0.0864704362711582,
-0.800064186306747));
#44835=CARTESIAN_POINT('Ctrl Pts',(-0.0808567581428261,-0.0620896144513321,
-0.802173406645372));
#44836=CARTESIAN_POINT('Ctrl Pts',(-0.0913924057352866,-0.0319944786077929,
-0.804282626983995));
#44837=CARTESIAN_POINT('Ctrl Pts',(-0.0949618328143147,-0.0217983903384935,
-0.804997220759675));
#44838=CARTESIAN_POINT('Ctrl Pts',(-0.0966576734591616,-0.0109464005149062,
-0.805711814535354));
#44839=CARTESIAN_POINT('Ctrl Pts',(-0.0965822410032082,-7.15798389840372E-5,
-0.806426408311033));
#44840=CARTESIAN_POINT('Ctrl Pts',(-0.0965865764190601,-7.32614358284168E-5,
-0.812223591688968));
#44841=CARTESIAN_POINT('Ctrl Pts',(-0.0966626916770759,-0.0107609700178141,
-0.811521213676251));
#44842=CARTESIAN_POINT('Ctrl Pts',(-0.0950257264917633,-0.0214260273296114,
-0.810818835663534));
#44843=CARTESIAN_POINT('Ctrl Pts',(-0.0915750664262514,-0.0314678465331367,
-0.810116457650817));
#44844=CARTESIAN_POINT('Ctrl Pts',(-0.0812128366011709,-0.0616231317461982,
-0.808007237312193));
#44845=CARTESIAN_POINT('Ctrl Pts',(-0.054495013125528,-0.0861581611170432,
-0.805898016973569));
#44846=CARTESIAN_POINT('Ctrl Pts',(-0.0235678906783709,-0.0939189686756064,
-0.803788796634945));
#44847=CARTESIAN_POINT('Ctrl Pts',(0.00735923176878642,-0.10167977623417,
-0.801679576296321));
#44848=CARTESIAN_POINT('Ctrl Pts',(0.042495653187458,-0.0926663619804508,
-0.799570355957697));
#44849=CARTESIAN_POINT('Ctrl Pts',(0.0658678673583969,-0.0709763495441025,
-0.797461135619073));
#44850=CARTESIAN_POINT('Ctrl Pts',(0.0892400815293357,-0.0492863371077543,
-0.795351915280449));
#44851=CARTESIAN_POINT('Ctrl Pts',(0.100848088452542,-0.0149197264887765,
-0.793242694941826));
#44852=CARTESIAN_POINT('Ctrl Pts',(0.0954147265327156,0.0164999427199751,
-0.791133474603202));
#44853=CARTESIAN_POINT('Ctrl Pts',(0.0899813646128891,0.0479196119287269,
-0.789024254264578));
#44854=CARTESIAN_POINT('Ctrl Pts',(0.0675066338500296,0.0763923397272526,
-0.786915033925953));
#44855=CARTESIAN_POINT('Ctrl Pts',(0.0382078597500414,0.0889740276760835,
-0.784805813587329));
#44856=CARTESIAN_POINT('Ctrl Pts',(0.00890908565005346,0.101555715624914,
-0.782696593248705));
#44857=CARTESIAN_POINT('Ctrl Pts',(-0.0272137317870626,0.0982463637240508,
-0.780587372910081));
#44858=CARTESIAN_POINT('Ctrl Pts',(-0.0537386568974374,0.0805504494224217,
-0.778478152571458));
#44859=CARTESIAN_POINT('Ctrl Pts',(-0.0799571535252079,0.0630589666939328,
-0.776393298943961));
#44860=CARTESIAN_POINT('Ctrl Pts',(-0.0967982356800078,0.0315114022882873,
-0.774308445316464));
#44861=CARTESIAN_POINT('Ctrl Pts',(-0.0968302674661193,-6.76949675972993E-6,
-0.772223591688968));
#44862=CARTESIAN_POINT('Origin',(0.,0.,-0.493));
#44863=CARTESIAN_POINT('',(-0.096609779660466,8.02748517758078E-5,-0.726426408311033));
#44864=CARTESIAN_POINT('',(-0.0966049344323358,7.90599391692882E-5,-0.732223591688968));
#44865=CARTESIAN_POINT('',(-0.096675,-1.1839272930757E-17,-0.493));
#44866=CARTESIAN_POINT('Ctrl Pts',(-0.096609779660466,8.02748517758078E-5,
-0.726426408311033));
#44867=CARTESIAN_POINT('Ctrl Pts',(-0.096687244674842,0.00983463108919295,
-0.727067837138532));
#44868=CARTESIAN_POINT('Ctrl Pts',(-0.0953275566972926,0.0195678958140022,
-0.727709265966032));
#44869=CARTESIAN_POINT('Ctrl Pts',(-0.092440982531473,0.0288250452673198,
-0.728350694793532));
#44870=CARTESIAN_POINT('Ctrl Pts',(-0.0829490160365677,0.0592654730552798,
-0.730459915132156));
#44871=CARTESIAN_POINT('Ctrl Pts',(-0.0569468007063695,0.0845576575314614,
-0.732569135470779));
#44872=CARTESIAN_POINT('Ctrl Pts',(-0.0262553056107718,0.0932034195366821,
-0.734678355809403));
#44873=CARTESIAN_POINT('Ctrl Pts',(0.00443618948482572,0.101849181541903,
-0.736787576148027));
#44874=CARTESIAN_POINT('Ctrl Pts',(0.0398169643458228,0.0938485210761628,
-0.738896796486651));
#44875=CARTESIAN_POINT('Ctrl Pts',(0.0638024261793546,0.072838649765581,
-0.741006016825275));
#44876=CARTESIAN_POINT('Ctrl Pts',(0.0877878880128864,0.0518287784549991,
-0.7431152371639));
#44877=CARTESIAN_POINT('Ctrl Pts',(0.100378036818953,0.0178096962995753,
-0.745224457502523));
#44878=CARTESIAN_POINT('Ctrl Pts',(0.0958492156808683,-0.0137530483680479,
-0.747333677841147));
#44879=CARTESIAN_POINT('Ctrl Pts',(0.0913203945427836,-0.0453157930356709,
-0.749442898179771));
#44880=CARTESIAN_POINT('Ctrl Pts',(0.0696726034605476,-0.0744222002154934,
-0.751552118518395));
#44881=CARTESIAN_POINT('Ctrl Pts',(0.0407472296224764,-0.0878400920089121,
-0.753661338857019));
#44882=CARTESIAN_POINT('Ctrl Pts',(0.0118218557844046,-0.101257983802331,
-0.755770559195643));
#44883=CARTESIAN_POINT('Ctrl Pts',(-0.0243811008095024,-0.0989873602093457,
-0.757879779534267));
#44884=CARTESIAN_POINT('Ctrl Pts',(-0.0514032721051547,-0.082060478324969,
-0.759988999872891));
#44885=CARTESIAN_POINT('Ctrl Pts',(-0.0784254434008066,-0.0651335964405926,
-0.762098220211515));
#44886=CARTESIAN_POINT('Ctrl Pts',(-0.0962668293982039,-0.0335504562648253,
-0.76420744055014));
#44887=CARTESIAN_POINT('Ctrl Pts',(-0.0968164876497021,-0.00166919299532548,
-0.766316660888763));
#44888=CARTESIAN_POINT('Ctrl Pts',(-0.0968260209632092,-0.00111624199909807,
-0.766353243362853));
#44889=CARTESIAN_POINT('Ctrl Pts',(-0.0968303526326005,-0.000563201322402664,
-0.766389825836943));
#44890=CARTESIAN_POINT('Ctrl Pts',(-0.0968295223683655,-1.01472914774969E-5,
-0.766426408311033));
#44891=CARTESIAN_POINT('Ctrl Pts',(-0.0968302674661193,-6.76949675972993E-6,
-0.772223591688968));
#44892=CARTESIAN_POINT('Ctrl Pts',(-0.0968306418373791,-0.00037513789299813,
-0.77219922497784));
#44893=CARTESIAN_POINT('Ctrl Pts',(-0.096828720134703,-0.000743502274278584,
-0.772174858266713));
#44894=CARTESIAN_POINT('Ctrl Pts',(-0.0968244904936179,-0.00111184015339449,
-0.772150491555585));
#44895=CARTESIAN_POINT('Ctrl Pts',(-0.0964583661957905,-0.0329957387251863,
-0.770041271216961));
#44896=CARTESIAN_POINT('Ctrl Pts',(-0.0787990848165025,-0.064681059166375,
-0.767932050878338));
#44897=CARTESIAN_POINT('Ctrl Pts',(-0.0518748015122534,-0.0817632137069352,
-0.765822830539714));
#44898=CARTESIAN_POINT('Ctrl Pts',(-0.0249505182080041,-0.0988453682474956,
-0.76371361020109));
#44899=CARTESIAN_POINT('Ctrl Pts',(0.0112387670212067,-0.101324356887427,
-0.761604389862466));
#44900=CARTESIAN_POINT('Ctrl Pts',(0.0402409013157684,-0.0880731968813481,
-0.759495169523841));
#44901=CARTESIAN_POINT('Ctrl Pts',(0.06924303561033,-0.0748220368752688,
-0.757385949185217));
#44902=CARTESIAN_POINT('Ctrl Pts',(0.0910580189702425,-0.0458407282231786,
-0.755276728846593));
#44903=CARTESIAN_POINT('Ctrl Pts',(0.0957684562693173,-0.0143045772911135,
-0.753167508507969));
#44904=CARTESIAN_POINT('Ctrl Pts',(0.100478893568392,0.0172315736409515,
-0.751058288169346));
#44905=CARTESIAN_POINT('Ctrl Pts',(0.0880847848066293,0.0513225668529911,
-0.748949067830722));
#44906=CARTESIAN_POINT('Ctrl Pts',(0.0642206643679629,0.0724701622447588,
-0.746839847492098));
#44907=CARTESIAN_POINT('Ctrl Pts',(0.0403565439292966,0.0936177576365265,
-0.744730627153474));
#44908=CARTESIAN_POINT('Ctrl Pts',(0.00502241181372707,0.101821955208023,
-0.74262140681485));
#44909=CARTESIAN_POINT('Ctrl Pts',(-0.0257183436275326,0.0933530125314768,
-0.740512186476226));
#44910=CARTESIAN_POINT('Ctrl Pts',(-0.0564590990687925,0.084884069854931,
-0.738402966137602));
#44911=CARTESIAN_POINT('Ctrl Pts',(-0.0826064778357426,0.0597419869303427,
-0.736293745798978));
#44912=CARTESIAN_POINT('Ctrl Pts',(-0.0922735175391629,0.0293567046619034,
-0.734184525460354));
#44913=CARTESIAN_POINT('Ctrl Pts',(-0.0952693203446887,0.0199403459151532,
-0.733530880869892));
#44914=CARTESIAN_POINT('Ctrl Pts',(-0.0966823977057856,0.0100204450398257,
-0.73287723627943));
#44915=CARTESIAN_POINT('Ctrl Pts',(-0.0966049344323358,7.90599391692882E-5,
-0.732223591688968));
#44916=CARTESIAN_POINT('Origin',(0.,0.,-0.493));
#44917=CARTESIAN_POINT('',(-0.09655822028916,-5.94095412307302E-5,-0.686426408311032));
#44918=CARTESIAN_POINT('',(-0.0965617881854164,-6.15864372647569E-5,-0.692223591688968));
#44919=CARTESIAN_POINT('',(-0.096675,-1.1839272930757E-17,-0.493));
#44920=CARTESIAN_POINT('Ctrl Pts',(-0.09655822028916,-5.94095412307302E-5,
-0.686426408311032));
#44921=CARTESIAN_POINT('Ctrl Pts',(-0.096444469996802,0.0200326449855016,
-0.687745848440121));
#44922=CARTESIAN_POINT('Ctrl Pts',(-0.0903271586571913,0.0401881545090195,
-0.689065288569211));
#44923=CARTESIAN_POINT('Ctrl Pts',(-0.0787087709636884,0.0564016653959087,
-0.6903847286983));
#44924=CARTESIAN_POINT('Ctrl Pts',(-0.0601359391353336,0.0823201335167296,
-0.692493949036924));
#44925=CARTESIAN_POINT('Ctrl Pts',(-0.0275054744417361,0.0981650876515461,
-0.694603169375547));
#44926=CARTESIAN_POINT('Ctrl Pts',(0.00434835961377499,0.0967331910706748,
-0.696712389714171));
#44927=CARTESIAN_POINT('Ctrl Pts',(0.0362021936692865,0.0953012944898034,
-0.698821610052795));
#44928=CARTESIAN_POINT('Ctrl Pts',(0.0672793970867115,0.076592547193244,
-0.70093083039142));
#44929=CARTESIAN_POINT('Ctrl Pts',(0.0834518405620545,0.0491122061493044,
-0.703040050730044));
#44930=CARTESIAN_POINT('Ctrl Pts',(0.0996242840373975,0.0216318651053648,
-0.705149271068668));
#44931=CARTESIAN_POINT('Ctrl Pts',(0.100891967570659,-0.0146200696859549,
-0.707258491407292));
#44932=CARTESIAN_POINT('Ctrl Pts',(0.0866785845800015,-0.0431629639998695,
-0.709367711745916));
#44933=CARTESIAN_POINT('Ctrl Pts',(0.0724652015893446,-0.0717058583137836,
-0.71147693208454));
#44934=CARTESIAN_POINT('Ctrl Pts',(0.0427707520747702,-0.0925397121502928,
-0.713586152423164));
#44935=CARTESIAN_POINT('Ctrl Pts',(0.0110947461665166,-0.0961931655241,
-0.715695372761788));
#44936=CARTESIAN_POINT('Ctrl Pts',(-0.0205812597417374,-0.0998466188979071,
-0.717804593100411));
#44937=CARTESIAN_POINT('Ctrl Pts',(-0.0542388220436707,-0.0863196718090117,
-0.719913813439035));
#44938=CARTESIAN_POINT('Ctrl Pts',(-0.0745767443648309,-0.0617618627146946,
-0.722023033777659));
#44939=CARTESIAN_POINT('Ctrl Pts',(-0.0887297606193485,-0.0446722571100165,
-0.723490825288783));
#44940=CARTESIAN_POINT('Ctrl Pts',(-0.0964325152694136,-0.0222407694604564,
-0.724958616799908));
#44941=CARTESIAN_POINT('Ctrl Pts',(-0.096609779660466,8.02748517758078E-5,
-0.726426408311033));
#44942=CARTESIAN_POINT('Ctrl Pts',(-0.0966049344323358,7.90599391692882E-5,
-0.732223591688968));
#44943=CARTESIAN_POINT('Ctrl Pts',(-0.0964324344776936,-0.0220590243757753,
-0.730768015940806));
#44944=CARTESIAN_POINT('Ctrl Pts',(-0.0888684767602903,-0.0443036470435852,
-0.729312440192644));
#44945=CARTESIAN_POINT('Ctrl Pts',(-0.0749310401969944,-0.0613315364445268,
-0.727856864444482));
#44946=CARTESIAN_POINT('Ctrl Pts',(-0.0547348225115145,-0.0860060136702274,
-0.725747644105858));
#44947=CARTESIAN_POINT('Ctrl Pts',(-0.0211556865006636,-0.0997264865093382,
-0.723638423767234));
#44948=CARTESIAN_POINT('Ctrl Pts',(0.0105408251448544,-0.0962554370044433,
-0.72152920342861));
#44949=CARTESIAN_POINT('Ctrl Pts',(0.0422373367903726,-0.0927843874995483,
-0.719419983089986));
#44950=CARTESIAN_POINT('Ctrl Pts',(0.0720512240705579,-0.0721218156506473,
-0.717310762751361));
#44951=CARTESIAN_POINT('Ctrl Pts',(0.0864286787841937,-0.0436612142670213,
-0.715201542412737));
#44952=CARTESIAN_POINT('Ctrl Pts',(0.100806133497829,-0.0152006128833955,
-0.713092322074114));
#44953=CARTESIAN_POINT('Ctrl Pts',(0.0997471556449157,0.0210580180349552,
-0.71098310173549));
#44954=CARTESIAN_POINT('Ctrl Pts',(0.0837331712995902,0.0486310001106758,
-0.708873881396866));
#44955=CARTESIAN_POINT('Ctrl Pts',(0.0677191869542648,0.0762039821863965,
-0.706764661058242));
#44956=CARTESIAN_POINT('Ctrl Pts',(0.0367501961165274,0.0950913154194871,
-0.704655440719617));
#44957=CARTESIAN_POINT('Ctrl Pts',(0.0049051331451982,0.0967065551887728,
-0.702546220380993));
#44958=CARTESIAN_POINT('Ctrl Pts',(-0.0269399298261309,0.0983217949580586,
-0.700437000042369));
#44959=CARTESIAN_POINT('Ctrl Pts',(-0.0596610649310518,0.0826649412635394,
-0.698327779703746));
#44960=CARTESIAN_POINT('Ctrl Pts',(-0.078382788635008,0.056853817756164,
-0.696218559365122));
#44961=CARTESIAN_POINT('Ctrl Pts',(-0.0902027456225251,0.0405579694421437,
-0.694886903473071));
#44962=CARTESIAN_POINT('Ctrl Pts',(-0.0964425008026231,0.0202146027618285,
-0.693555247581019));
#44963=CARTESIAN_POINT('Ctrl Pts',(-0.0965617881854164,-6.15864372647569E-5,
-0.692223591688968));
#44964=CARTESIAN_POINT('Origin',(0.,0.,-0.493));
#44965=CARTESIAN_POINT('',(-0.0968190249341983,-3.03081917537168E-5,-0.646426408311032));
#44966=CARTESIAN_POINT('',(-0.0968213716511174,-2.71350648972155E-5,-0.652223591688967));
#44967=CARTESIAN_POINT('',(-0.096675,-1.1839272930757E-17,-0.493));
#44968=CARTESIAN_POINT('Ctrl Pts',(-0.0968190249341983,-3.03081917537168E-5,
-0.646426408311032));
#44969=CARTESIAN_POINT('Ctrl Pts',(-0.0966942363656106,0.0301759440623484,
-0.648423859741711));
#44970=CARTESIAN_POINT('Ctrl Pts',(-0.0814178221682262,0.0604911215757958,
-0.65042131117239));
#44971=CARTESIAN_POINT('Ctrl Pts',(-0.0570098021767794,0.0782694125556777,
-0.652418762603068));
#44972=CARTESIAN_POINT('Ctrl Pts',(-0.0312360129367518,0.0970425012750384,
-0.654527982941692));
#44973=CARTESIAN_POINT('Ctrl Pts',(0.00471990542191003,0.10183642791609,
-0.656637203280316));
#44974=CARTESIAN_POINT('Ctrl Pts',(0.034511891865597,0.0904718066908345,
-0.65874642361894));
#44975=CARTESIAN_POINT('Ctrl Pts',(0.0643038783092844,0.079107185465579,
-0.660855643957563));
#44976=CARTESIAN_POINT('Ctrl Pts',(0.087931932837997,0.051584016374016,
-0.662964864296188));
#44977=CARTESIAN_POINT('Ctrl Pts',(0.0946544129332718,0.0204147152393576,
-0.665074084634812));
#44978=CARTESIAN_POINT('Ctrl Pts',(0.101376893028546,-0.0107545858953003,
-0.667183304973436));
#44979=CARTESIAN_POINT('Ctrl Pts',(0.0911937986903842,-0.0455700190730532,
-0.66929252531206));
#44980=CARTESIAN_POINT('Ctrl Pts',(0.068734506365305,-0.0682040037004004,
-0.671401745650684));
#44981=CARTESIAN_POINT('Ctrl Pts',(0.0462752140402253,-0.0908379883277482,
-0.673510965989308));
#44982=CARTESIAN_POINT('Ctrl Pts',(0.0115397237282281,-0.101290524404689,
-0.675620186327932));
#44983=CARTESIAN_POINT('Ctrl Pts',(-0.0196807271168537,-0.0948097435193152,
-0.677729406666556));
#44984=CARTESIAN_POINT('Ctrl Pts',(-0.0509011779619347,-0.0883289626339413,
-0.67983862700518));
#44985=CARTESIAN_POINT('Ctrl Pts',(-0.0786065893401007,-0.0649148647862529,
-0.681947847343803));
#44986=CARTESIAN_POINT('Ctrl Pts',(-0.0902016955476279,-0.035211824808996,
-0.684057067682427));
#44987=CARTESIAN_POINT('Ctrl Pts',(-0.0945433877086917,-0.0240897657678029,
-0.684846847891962));
#44988=CARTESIAN_POINT('Ctrl Pts',(-0.0966263080543815,-0.0120859552588177,
-0.685636628101497));
#44989=CARTESIAN_POINT('Ctrl Pts',(-0.09655822028916,-5.94095412307302E-5,
-0.686426408311032));
#44990=CARTESIAN_POINT('Ctrl Pts',(-0.0965617881854164,-6.15864372647569E-5,
-0.692223591688968));
#44991=CARTESIAN_POINT('Ctrl Pts',(-0.0966314410351792,-0.0119010142709122,
-0.691446027242395));
#44992=CARTESIAN_POINT('Ctrl Pts',(-0.0946143296894111,-0.0237175380444123,
-0.690668462795823));
#44993=CARTESIAN_POINT('Ctrl Pts',(-0.0904028966310228,-0.03469199372149,
-0.68989089834925));
#44994=CARTESIAN_POINT('Ctrl Pts',(-0.0789789686200898,-0.0644612883715367,
-0.687781678010626));
#44995=CARTESIAN_POINT('Ctrl Pts',(-0.0514088002952321,-0.0880344843513981,
-0.685672457672002));
#44996=CARTESIAN_POINT('Ctrl Pts',(-0.0202261739853999,-0.0946948786026133,
-0.683563237333378));
#44997=CARTESIAN_POINT('Ctrl Pts',(0.0109564523244319,-0.101355272853828,
-0.681454016994754));
#44998=CARTESIAN_POINT('Ctrl Pts',(0.0457515366192382,-0.091102865376398,
-0.679344796656129));
#44999=CARTESIAN_POINT('Ctrl Pts',(0.0683407491909844,-0.0685985433348721,
-0.677235576317506));
#45000=CARTESIAN_POINT('Ctrl Pts',(0.0909299617627307,-0.046094221293346,
-0.675126355978882));
#45001=CARTESIAN_POINT('Ctrl Pts',(0.101313302611417,-0.0113379846877243,
-0.673017135640258));
#45002=CARTESIAN_POINT('Ctrl Pts',(0.0947703604391765,0.0198694974742666,
-0.670907915301634));
#45003=CARTESIAN_POINT('Ctrl Pts',(0.0882274182669362,0.0510769796362577,
-0.66879869496301));
#45004=CARTESIAN_POINT('Ctrl Pts',(0.0647581930737698,0.0787357073546175,
-0.666689474624386));
#45005=CARTESIAN_POINT('Ctrl Pts',(0.0350321213511129,0.090271637967261,
-0.664580254285762));
#45006=CARTESIAN_POINT('Ctrl Pts',(0.00530604962845649,0.101807568579904,
-0.662471033947138));
#45007=CARTESIAN_POINT('Ctrl Pts',(-0.03067686862369,0.0972207020868314,
-0.660361813608514));
#45008=CARTESIAN_POINT('Ctrl Pts',(-0.0565582978442699,0.0785962918502532,
-0.65825259326989));
#45009=CARTESIAN_POINT('Ctrl Pts',(-0.0812181488217498,0.0608509356311975,
-0.656242926076249));
#45010=CARTESIAN_POINT('Ctrl Pts',(-0.0967075680763441,0.0303618803342572,
-0.654233258882608));
#45011=CARTESIAN_POINT('Ctrl Pts',(-0.0968213716511174,-2.71350648972155E-5,
-0.652223591688967));
#45012=CARTESIAN_POINT('Origin',(0.,0.,-0.493));
#45013=CARTESIAN_POINT('',(-0.0966413181482248,8.54984747835699E-5,-0.606426408311032));
#45014=CARTESIAN_POINT('',(-0.0966360180667763,8.49218538845601E-5,-0.612223591688967));
#45015=CARTESIAN_POINT('',(-0.096675,-1.1839272930757E-17,-0.493));
#45016=CARTESIAN_POINT('Ctrl Pts',(-0.0966413181482248,8.54984747835699E-5,
-0.606426408311032));
#45017=CARTESIAN_POINT('Ctrl Pts',(-0.0967160133304872,0.0086893470084329,
-0.606992650704676));
#45018=CARTESIAN_POINT('Ctrl Pts',(-0.0956611835672563,0.0172751935884665,
-0.60755889309832));
#45019=CARTESIAN_POINT('Ctrl Pts',(-0.0934040461356575,0.0255323843683732,
-0.608125135491964));
#45020=CARTESIAN_POINT('Ctrl Pts',(-0.0849963390631441,0.0562899449614566,
-0.610234355830588));
#45021=CARTESIAN_POINT('Ctrl Pts',(-0.0599063769810964,0.0824873417858737,
-0.612343576169212));
#45022=CARTESIAN_POINT('Ctrl Pts',(-0.0295404059331587,0.0922148735473329,
-0.614452796507836));
#45023=CARTESIAN_POINT('Ctrl Pts',(0.000825565114778395,0.101942405308792,
-0.61656201684646));
#45024=CARTESIAN_POINT('Ctrl Pts',(0.0364675451286056,0.0952000720072934,
-0.618671237185084));
#45025=CARTESIAN_POINT('Ctrl Pts',(0.0611821938166583,0.0750530322227374,
-0.620780457523708));
#45026=CARTESIAN_POINT('Ctrl Pts',(0.0858968425047111,0.0549059924381812,
-0.622889677862332));
#45027=CARTESIAN_POINT('Ctrl Pts',(0.0996841598669897,0.0213542461705674,
-0.624998898200956));
#45028=CARTESIAN_POINT('Ctrl Pts',(0.0962762394952784,-0.010349115647928,
-0.62710811853958));
#45029=CARTESIAN_POINT('Ctrl Pts',(0.0928683191235671,-0.042052477466424,
-0.629217338878204));
#45030=CARTESIAN_POINT('Ctrl Pts',(0.0722651610178653,-0.0719074548358012,
-0.631326559216828));
#45031=CARTESIAN_POINT('Ctrl Pts',(0.0438332476726959,-0.086341559428299,
-0.633435779555452));
#45032=CARTESIAN_POINT('Ctrl Pts',(0.0154013343275267,-0.100775664020797,
-0.635544999894076));
#45033=CARTESIAN_POINT('Ctrl Pts',(-0.0208593342571104,-0.0997888958364151,
-0.6376542202327));
#45034=CARTESIAN_POINT('Ctrl Pts',(-0.0484641533524033,-0.0838298534287226,
-0.639763440571324));
#45035=CARTESIAN_POINT('Ctrl Pts',(-0.0760689724476961,-0.0678708110210303,
-0.641872660909948));
#45036=CARTESIAN_POINT('Ctrl Pts',(-0.0950179420536452,-0.0369394943900277,
-0.643981881248572));
#45037=CARTESIAN_POINT('Ctrl Pts',(-0.0966965967959232,-0.00509771067569107,
-0.646091101587196));
#45038=CARTESIAN_POINT('Ctrl Pts',(-0.0967855497630107,-0.00341039459608733,
-0.646202870495141));
#45039=CARTESIAN_POINT('Ctrl Pts',(-0.0968260075730854,-0.00172052191896296,
-0.646314639403087));
#45040=CARTESIAN_POINT('Ctrl Pts',(-0.0968190249341983,-3.03081917537168E-5,
-0.646426408311032));
#45041=CARTESIAN_POINT('Ctrl Pts',(-0.0968213716511174,-2.71350648972155E-5,
-0.652223591688967));
#45042=CARTESIAN_POINT('Ctrl Pts',(-0.0968270091535929,-0.00153251967061721,
-0.652124038543984));
#45043=CARTESIAN_POINT('Ctrl Pts',(-0.0967949160138212,-0.00303765878570629,
-0.652024485399001));
#45044=CARTESIAN_POINT('Ctrl Pts',(-0.0967243379264574,-0.00454099111866625,
-0.651924932254018));
#45045=CARTESIAN_POINT('Ctrl Pts',(-0.0952290085990514,-0.0363919098709228,
-0.649815711915394));
#45046=CARTESIAN_POINT('Ctrl Pts',(-0.0764584097552263,-0.0674317933953525,
-0.64770649157677));
#45047=CARTESIAN_POINT('Ctrl Pts',(-0.0489459169377222,-0.0835494785308498,
-0.645597271238146));
#45048=CARTESIAN_POINT('Ctrl Pts',(-0.0214334241202177,-0.0996671636663474,
-0.643488050899522));
#45049=CARTESIAN_POINT('Ctrl Pts',(0.0148209626709659,-0.100862650412913,
-0.641378830560898));
#45050=CARTESIAN_POINT('Ctrl Pts',(0.0433354944977714,-0.0865924538530059,
-0.639269610222274));
#45051=CARTESIAN_POINT('Ctrl Pts',(0.0718500263245767,-0.0723222572930992,
-0.63716038988365));
#45052=CARTESIAN_POINT('Ctrl Pts',(0.0926247031870034,-0.0425863774267208,
-0.635051169545026));
#45053=CARTESIAN_POINT('Ctrl Pts',(0.0962150677759835,-0.0109031591987936,
-0.632941949206402));
#45054=CARTESIAN_POINT('Ctrl Pts',(0.0998054323649636,0.0207800590291337,
-0.630832728867778));
#45055=CARTESIAN_POINT('Ctrl Pts',(0.0862114846804966,0.0544106156186099,
-0.628723508529154));
#45056=CARTESIAN_POINT('Ctrl Pts',(0.0616132225833369,0.074699591368009,
-0.62661428819053));
#45057=CARTESIAN_POINT('Ctrl Pts',(0.0370149604861774,0.0949885671174079,
-0.624505067851906));
#45058=CARTESIAN_POINT('Ctrl Pts',(0.00141238397632584,0.10193596202673,
-0.622395847513282));
#45059=CARTESIAN_POINT('Ctrl Pts',(-0.0290090800360038,0.0923833936544662,
-0.620286627174659));
#45060=CARTESIAN_POINT('Ctrl Pts',(-0.0594305440483332,0.0828308252822022,
-0.618177406836035));
#45061=CARTESIAN_POINT('Ctrl Pts',(-0.0846708955631408,0.0567782936283514,
-0.61606818649741));
#45062=CARTESIAN_POINT('Ctrl Pts',(-0.0932555194070551,0.0260696422639763,
-0.613958966158786));
#45063=CARTESIAN_POINT('Ctrl Pts',(-0.0956098707249212,0.0176477294202516,
-0.61338050800218));
#45064=CARTESIAN_POINT('Ctrl Pts',(-0.0967114743576563,0.00887561013077407,
-0.612802049845574));
#45065=CARTESIAN_POINT('Ctrl Pts',(-0.0966360180667763,8.49218538845601E-5,
-0.612223591688967));
#45066=CARTESIAN_POINT('Origin',(0.,0.,-0.493));
#45067=CARTESIAN_POINT('',(-0.0965393946746019,-4.45580922561403E-5,-0.566426408311032));
#45068=CARTESIAN_POINT('',(-0.0965420680789469,-4.71254655582805E-5,-0.572223591688968));
#45069=CARTESIAN_POINT('',(-0.096675,-1.1839272930757E-17,-0.493));
#45070=CARTESIAN_POINT('Ctrl Pts',(-0.0965393946746019,-4.45580922561403E-5,
-0.566426408311032));
#45071=CARTESIAN_POINT('Ctrl Pts',(-0.0964598943699223,0.0189118469550805,
-0.567670662006265));
#45072=CARTESIAN_POINT('Ctrl Pts',(-0.0910651542801533,0.0379100173100681,
-0.568914915701499));
#45073=CARTESIAN_POINT('Ctrl Pts',(-0.0806573094966741,0.0535781383663534,
-0.570159169396732));
#45074=CARTESIAN_POINT('Ctrl Pts',(-0.0630142532753806,0.0801382520526055,
-0.572268389735356));
#45075=CARTESIAN_POINT('Ctrl Pts',(-0.030965549107614,0.097129142518426,
-0.57437761007398));
#45076=CARTESIAN_POINT('Ctrl Pts',(0.00091901593711588,0.0968265144253046,
-0.576486830412604));
#45077=CARTESIAN_POINT('Ctrl Pts',(0.0328035809818462,0.0965238863321833,
-0.578596050751228));
#45078=CARTESIAN_POINT('Ctrl Pts',(0.0645240069035398,0.0789277396801196,
-0.580705271089852));
#45079=CARTESIAN_POINT('Ctrl Pts',(0.0816597464933621,0.0520375276957528,
-0.582814491428476));
#45080=CARTESIAN_POINT('Ctrl Pts',(0.0987954860831841,0.0251473157113864,
-0.5849237117671));
#45081=CARTESIAN_POINT('Ctrl Pts',(0.101346539341135,-0.0110369616052829,
-0.587032932105724));
#45082=CARTESIAN_POINT('Ctrl Pts',(0.0881531619425538,-0.0400654280593166,
-0.589142152444348));
#45083=CARTESIAN_POINT('Ctrl Pts',(0.0749597845439722,-0.0690938945133507,
-0.591251372782972));
#45084=CARTESIAN_POINT('Ctrl Pts',(0.0460219764888577,-0.090966550104749,
-0.593360593121596));
#45085=CARTESIAN_POINT('Ctrl Pts',(0.0144952681666549,-0.0957397811091249,
-0.59546981346022));
#45086=CARTESIAN_POINT('Ctrl Pts',(-0.0170314401555474,-0.100513012113501,
-0.597579033798844));
#45087=CARTESIAN_POINT('Ctrl Pts',(-0.0511470487448379,-0.0881868185308549,
-0.599688254137468));
#45088=CARTESIAN_POINT('Ctrl Pts',(-0.0723421270079938,-0.0643648595586574,
-0.601797474476092));
#45089=CARTESIAN_POINT('Ctrl Pts',(-0.0878471634915268,-0.0469381561331164,
-0.603340452421072));
#45090=CARTESIAN_POINT('Ctrl Pts',(-0.0964377780740077,-0.0233594937730345,
-0.604883430366052));
#45091=CARTESIAN_POINT('Ctrl Pts',(-0.0966413181482248,8.54984747835699E-5,
-0.606426408311032));
#45092=CARTESIAN_POINT('Ctrl Pts',(-0.0966360180667763,8.49218538845601E-5,
-0.612223591688967));
#45093=CARTESIAN_POINT('Ctrl Pts',(-0.0964363396023009,-0.0231776996762786,
-0.610692829506949));
#45094=CARTESIAN_POINT('Ctrl Pts',(-0.0879939491883497,-0.0465703560596884,
-0.609162067324932));
#45095=CARTESIAN_POINT('Ctrl Pts',(-0.0727114440849164,-0.0639473537117637,
-0.607631305142914));
#45096=CARTESIAN_POINT('Ctrl Pts',(-0.0516538487458423,-0.0878909272482276,
-0.60552208480429));
#45097=CARTESIAN_POINT('Ctrl Pts',(-0.0176097618946735,-0.100413303246256,
-0.603412864465667));
#45098=CARTESIAN_POINT('Ctrl Pts',(0.0139439006531827,-0.0958216352512599,
-0.601303644127043));
#45099=CARTESIAN_POINT('Ctrl Pts',(0.0454975632010391,-0.0912299672562642,
-0.599194423788419));
#45100=CARTESIAN_POINT('Ctrl Pts',(0.0745608014455828,-0.0695242552682441,
-0.597085203449794));
#45101=CARTESIAN_POINT('Ctrl Pts',(0.0879210626871216,-0.0405722181254436,
-0.59497598311117));
#45102=CARTESIAN_POINT('Ctrl Pts',(0.10128132392866,-0.0116201809826433,
-0.592866762772546));
#45103=CARTESIAN_POINT('Ctrl Pts',(0.0989386081671945,0.0245781813149372,
-0.590757542433923));
#45104=CARTESIAN_POINT('Ctrl Pts',(0.0819579466011862,0.0515665893439584,
-0.588648322095299));
#45105=CARTESIAN_POINT('Ctrl Pts',(0.0649772850351777,0.0785549973729798,
-0.586539101756675));
#45106=CARTESIAN_POINT('Ctrl Pts',(0.033358677664626,0.0963334511334416,
-0.58442988141805));
#45107=CARTESIAN_POINT('Ctrl Pts',(0.00147638356758545,0.0968196180493019,
-0.582320661079426));
#45108=CARTESIAN_POINT('Ctrl Pts',(-0.0304059105294553,0.0973057849651621,
-0.580211440740802));
#45109=CARTESIAN_POINT('Ctrl Pts',(-0.0625518913529849,0.080499665036421,
-0.578102220402179));
#45110=CARTESIAN_POINT('Ctrl Pts',(-0.0803475485115806,0.0540415543432139,
-0.575993000063555));
#45111=CARTESIAN_POINT('Ctrl Pts',(-0.0909484797176978,0.0382803712184285,
-0.574736530605359));
#45112=CARTESIAN_POINT('Ctrl Pts',(-0.096457020786623,0.0190940595933471,
-0.573480061147164));
#45113=CARTESIAN_POINT('Ctrl Pts',(-0.0965420680789469,-4.71254655582805E-5,
-0.572223591688968));
#45114=CARTESIAN_POINT('Origin',(0.,0.,-0.493));
#45115=CARTESIAN_POINT('',(-0.0967998842052739,-4.85300446802506E-5,-0.526426408311032));
#45116=CARTESIAN_POINT('',(-0.0968034943207674,-4.57450494820897E-5,-0.532223591688968));
#45117=CARTESIAN_POINT('',(-0.096675,-1.1839272930757E-17,-0.493));
#45118=CARTESIAN_POINT('Ctrl Pts',(-0.0967998842052739,-4.85300446802506E-5,
-0.526426408311032));
#45119=CARTESIAN_POINT('Ctrl Pts',(-0.0966204449976918,0.0290359816449859,
-0.528348673307855));
#45120=CARTESIAN_POINT('Ctrl Pts',(-0.0826150578079472,0.058270385292619,
-0.530270938304678));
#45121=CARTESIAN_POINT('Ctrl Pts',(-0.0597465881474668,0.0762008116149912,
-0.5321932033015));
#45122=CARTESIAN_POINT('Ctrl Pts',(-0.034653980520104,0.095875112474578,
-0.534302423640124));
#45123=CARTESIAN_POINT('Ctrl Pts',(0.00110955476683836,0.101939709858917,
-0.536411643978749));
#45124=CARTESIAN_POINT('Ctrl Pts',(0.0312854167023489,0.0916375533709122,
-0.538520864317373));
#45125=CARTESIAN_POINT('Ctrl Pts',(0.0614612786378607,0.0813353968829074,
-0.540630084655997));
#45126=CARTESIAN_POINT('Ctrl Pts',(0.0860494672219405,0.0546664865225578,
-0.54273930499462));
#45127=CARTESIAN_POINT('Ctrl Pts',(0.093871849628384,0.0237548802016017,
-0.544848525333244));
#45128=CARTESIAN_POINT('Ctrl Pts',(0.101694232034827,-0.0071567261193535,
-0.546957745671868));
#45129=CARTESIAN_POINT('Ctrl Pts',(0.0927508082636355,-0.0423110284009153,
-0.549066966010493));
#45130=CARTESIAN_POINT('Ctrl Pts',(0.0711073832639433,-0.0657263914375426,
-0.551176186349117));
#45131=CARTESIAN_POINT('Ctrl Pts',(0.0494639582642506,-0.0891417544741703,
-0.553285406687741));
#45132=CARTESIAN_POINT('Ctrl Pts',(0.0151205320360575,-0.100818178265863,
-0.555394627026364));
#45133=CARTESIAN_POINT('Ctrl Pts',(-0.0163098957572849,-0.0954473980076612,
-0.557503847364988));
#45134=CARTESIAN_POINT('Ctrl Pts',(-0.0477403235506265,-0.0900766177494595,
-0.559613067703612));
#45135=CARTESIAN_POINT('Ctrl Pts',(-0.0762577529091172,-0.0676586334413634,
-0.561722288042237));
#45136=CARTESIAN_POINT('Ctrl Pts',(-0.0888977634509525,-0.0383849728339736,
-0.563831508380861));
#45137=CARTESIAN_POINT('Ctrl Pts',(-0.0940812842479904,-0.0263801862824427,
-0.564696475024251));
#45138=CARTESIAN_POINT('Ctrl Pts',(-0.0965946608248659,-0.0132224639384352,
-0.565561441667642));
#45139=CARTESIAN_POINT('Ctrl Pts',(-0.0965393946746019,-4.45580922561403E-5,
-0.566426408311032));
#45140=CARTESIAN_POINT('Ctrl Pts',(-0.0965420680789469,-4.71254655582805E-5,
-0.572223591688968));
#45141=CARTESIAN_POINT('Ctrl Pts',(-0.0965997886649382,-0.0130380201546043,
-0.571370840808539));
#45142=CARTESIAN_POINT('Ctrl Pts',(-0.0941593528399191,-0.0260081287553386,
-0.570518089928111));
#45143=CARTESIAN_POINT('Ctrl Pts',(-0.0891172524233399,-0.0378725952129777,
-0.569665339047682));
#45144=CARTESIAN_POINT('Ctrl Pts',(-0.076645965682842,-0.0672185326182907,
-0.567556118709058));
#45145=CARTESIAN_POINT('Ctrl Pts',(-0.0482580587081843,-0.0898003059712441,
-0.565446898370435));
#45146=CARTESIAN_POINT('Ctrl Pts',(-0.0168590692023799,-0.0953519267413129,
-0.563337678031811));
#45147=CARTESIAN_POINT('Ctrl Pts',(0.014539920303424,-0.100903547511382,
-0.561228457693187));
#45148=CARTESIAN_POINT('Ctrl Pts',(0.0489499923403744,-0.0894250156985665,
-0.559119237354563));
#45149=CARTESIAN_POINT('Ctrl Pts',(0.0707278491326723,-0.0661346316593453,
-0.557010017015939));
#45150=CARTESIAN_POINT('Ctrl Pts',(0.0925057059249705,-0.0428442476201238,
-0.554900796677315));
#45151=CARTESIAN_POINT('Ctrl Pts',(0.101651347472616,-0.00774201135449594,
-0.552791576338691));
#45152=CARTESIAN_POINT('Ctrl Pts',(0.0940070378101934,0.0232141118676594,
-0.550682356000067));
#45153=CARTESIAN_POINT('Ctrl Pts',(0.0863627281477711,0.0541702350898143,
-0.548573135661443));
#45154=CARTESIAN_POINT('Ctrl Pts',(0.0619284672752818,0.0809802452684969,
-0.546463915322819));
#45155=CARTESIAN_POINT('Ctrl Pts',(0.031812410338389,0.0914559385502838,
-0.544354694984195));
#45156=CARTESIAN_POINT('Ctrl Pts',(0.00169635340149625,0.101931631832071,
-0.542245474645571));
#45157=CARTESIAN_POINT('Ctrl Pts',(-0.0341014995998,0.0960730082169618,
-0.540136254306947));
#45158=CARTESIAN_POINT('Ctrl Pts',(-0.059306946343801,0.0765434795591685,
-0.538027033968323));
#45159=CARTESIAN_POINT('Ctrl Pts',(-0.0824242332745107,0.0586318859980991,
-0.536092553208537));
#45160=CARTESIAN_POINT('Ctrl Pts',(-0.0966314821794818,0.0292207067132771,
-0.534158072448753));
#45161=CARTESIAN_POINT('Ctrl Pts',(-0.0968034943207674,-4.57450494820897E-5,
-0.532223591688968));
#45162=CARTESIAN_POINT('Origin',(0.,0.,-0.493));
#45163=CARTESIAN_POINT('',(-0.0966749003444729,8.66157029079558E-5,-0.486426408311032));
#45164=CARTESIAN_POINT('',(-0.096669360704088,8.67233818675543E-5,-0.492223591688967));
#45165=CARTESIAN_POINT('',(-0.096675,-1.1839272930757E-17,-0.493));
#45166=CARTESIAN_POINT('Ctrl Pts',(-0.0966749003444729,8.66157029079557E-5,
-0.486426408311032));
#45167=CARTESIAN_POINT('Ctrl Pts',(-0.0967425505848559,0.00754142010055274,
-0.48691746427082));
#45168=CARTESIAN_POINT('Ctrl Pts',(-0.0959524121396197,0.0149820405673192,
-0.487408520230609));
#45169=CARTESIAN_POINT('Ctrl Pts',(-0.0942498682055356,0.0222076750085543,
-0.487899576190397));
#45170=CARTESIAN_POINT('Ctrl Pts',(-0.0869369739791434,0.0532437612613018,
-0.490008796529021));
#45171=CARTESIAN_POINT('Ctrl Pts',(-0.0627907582739773,0.0803134872439226,
-0.492118016867645));
#45172=CARTESIAN_POINT('Ctrl Pts',(-0.0327884268927159,0.0911105786829796,
-0.494227237206269));
#45173=CARTESIAN_POINT('Ctrl Pts',(-0.00278609551145491,0.101907670122036,
-0.496336457544893));
#45174=CARTESIAN_POINT('Ctrl Pts',(0.0330723515459016,0.09643212701753,
-0.498445677883517));
#45175=CARTESIAN_POINT('Ctrl Pts',(0.0584851650562304,0.0771732074906303,
-0.500554898222141));
#45176=CARTESIAN_POINT('Ctrl Pts',(0.0838979785665599,0.05791428796373,
-0.502664118560765));
#45177=CARTESIAN_POINT('Ctrl Pts',(0.0988651585298612,0.0248719920144367,
-0.504773338899389));
#45178=CARTESIAN_POINT('Ctrl Pts',(0.0965824165744489,-0.00693219263191769,
-0.506882559238013));
#45179=CARTESIAN_POINT('Ctrl Pts',(0.0942996746190366,-0.0387363772782712,
-0.508991779576637));
#45180=CARTESIAN_POINT('Ctrl Pts',(0.0747670107449108,-0.0693024506216854,
-0.511100999915261));
#45181=CARTESIAN_POINT('Ctrl Pts',(0.0468642458664085,-0.0847346502053275,
-0.513210220253885));
#45182=CARTESIAN_POINT('Ctrl Pts',(0.0189614809879057,-0.10016684978897,
-0.515319440592508));
#45183=CARTESIAN_POINT('Ctrl Pts',(-0.0173113848949743,-0.10046517561284,
-0.517428660931132));
#45184=CARTESIAN_POINT('Ctrl Pts',(-0.0454642019918381,-0.0854940046043682,
-0.519537881269756));
#45185=CARTESIAN_POINT('Ctrl Pts',(-0.0736170190887016,-0.0705228335958964,
-0.52164710160838));
#45186=CARTESIAN_POINT('Ctrl Pts',(-0.0936497873995494,-0.0402821657550826,
-0.523756321947005));
#45187=CARTESIAN_POINT('Ctrl Pts',(-0.0964553315710817,-0.00851982966725782,
-0.525865542285629));
#45188=CARTESIAN_POINT('Ctrl Pts',(-0.0967040070934641,-0.00570450578147726,
-0.52605249762743));
#45189=CARTESIAN_POINT('Ctrl Pts',(-0.0968173360750429,-0.00287722683364963,
-0.526239452969231));
#45190=CARTESIAN_POINT('Ctrl Pts',(-0.0967998842052739,-4.85300446802506E-5,
-0.526426408311032));
#45191=CARTESIAN_POINT('Ctrl Pts',(-0.0968034943207674,-4.57450494820897E-5,
-0.532223591688968));
#45192=CARTESIAN_POINT('Ctrl Pts',(-0.0968190319935881,-0.00268935234785623,
-0.532048852110129));
#45193=CARTESIAN_POINT('Ctrl Pts',(-0.0967200517379734,-0.00533177876867958,
-0.53187411253129));
#45194=CARTESIAN_POINT('Ctrl Pts',(-0.0965027761683216,-0.00796444219378559,
-0.531699372952451));
#45195=CARTESIAN_POINT('Ctrl Pts',(-0.0938801187621351,-0.0397424015884674,
-0.529590152613827));
#45196=CARTESIAN_POINT('Ctrl Pts',(-0.0740217634630564,-0.0700978866773524,
-0.527480932275203));
#45197=CARTESIAN_POINT('Ctrl Pts',(-0.0459555950412053,-0.0852308713557481,
-0.525371711936579));
#45198=CARTESIAN_POINT('Ctrl Pts',(-0.0178894266193546,-0.100363856034144,
-0.523262491597955));
#45199=CARTESIAN_POINT('Ctrl Pts',(0.0183845549252683,-0.10027434030205,
-0.521153271259331));
#45200=CARTESIAN_POINT('Ctrl Pts',(0.046375692606911,-0.0850030192574396,
-0.519044050920707));
#45201=CARTESIAN_POINT('Ctrl Pts',(0.074366830288554,-0.0697316982128287,
-0.516934830582083));
#45202=CARTESIAN_POINT('Ctrl Pts',(0.0940751241072166,-0.0392785718557001,
-0.514825610243459));
#45203=CARTESIAN_POINT('Ctrl Pts',(0.0965409093308046,-0.00748805537056879,
-0.512716389904835));
#45204=CARTESIAN_POINT('Ctrl Pts',(0.0990066945543925,0.0243024611145621,
-0.510607169566211));
#45205=CARTESIAN_POINT('Ctrl Pts',(0.0842299711829063,0.0574303677276956,
-0.508497949227587));
#45206=CARTESIAN_POINT('Ctrl Pts',(0.0589284433700178,0.0768352569439182,
-0.506388728888963));
#45207=CARTESIAN_POINT('Ctrl Pts',(0.0336269155571289,0.096240146160141,
-0.504279508550339));
#45208=CARTESIAN_POINT('Ctrl Pts',(-0.00219941669716259,0.101922017979453,
-0.502170288211715));
#45209=CARTESIAN_POINT('Ctrl Pts',(-0.032263404006282,0.0912978143745992,
-0.500061067873091));
#45210=CARTESIAN_POINT('Ctrl Pts',(-0.0623273913154009,0.080673610769746,
-0.497951847534467));
#45211=CARTESIAN_POINT('Ctrl Pts',(-0.0866290336793479,0.0537433317407283,
-0.495842627195843));
#45212=CARTESIAN_POINT('Ctrl Pts',(-0.0941204661726449,0.0227498570346129,
-0.493733406857219));
#45213=CARTESIAN_POINT('Ctrl Pts',(-0.095907963698499,0.0153546413126034,
-0.493230135134469));
#45214=CARTESIAN_POINT('Ctrl Pts',(-0.0967384119606225,0.00772809722163936,
-0.492726863411718));
#45215=CARTESIAN_POINT('Ctrl Pts',(-0.096669360704088,8.67233818675543E-5,
-0.492223591688967));
#45216=CARTESIAN_POINT('Origin',(0.,0.,-0.493));
#45217=CARTESIAN_POINT('',(-0.096526423484871,-2.77199618692811E-5,-0.446426408311032));
#45218=CARTESIAN_POINT('',(-0.0965281097149038,-3.05597964714245E-5,-0.452223591688967));
#45219=CARTESIAN_POINT('',(-0.096675,-1.1839272930757E-17,-0.493));
#45220=CARTESIAN_POINT('Ctrl Pts',(-0.096526423484871,-2.77199618692811E-5,
-0.446426408311032));
#45221=CARTESIAN_POINT('Ctrl Pts',(-0.0964803188479194,0.017789197404952,
-0.44759547557241));
#45222=CARTESIAN_POINT('Ctrl Pts',(-0.0917559201737887,0.0356288516457462,
-0.448764542833788));
#45223=CARTESIAN_POINT('Ctrl Pts',(-0.0825046063050242,0.0506873596126229,
-0.449933610095166));
#45224=CARTESIAN_POINT('Ctrl Pts',(-0.0658134714014635,0.0778557803890599,
-0.45204283043379));
#45225=CARTESIAN_POINT('Ctrl Pts',(-0.0343867555591216,0.0959712800790841,
-0.454152050772413));
#45226=CARTESIAN_POINT('Ctrl Pts',(-0.00251148129597715,0.0967983003350077,
-0.456261271111037));
#45227=CARTESIAN_POINT('Ctrl Pts',(0.0293637929671665,0.0976253205909313,
-0.458370491449661));
#45228=CARTESIAN_POINT('Ctrl Pts',(0.0616876256511122,0.0811638614127553,
-0.460479711788285));
#45229=CARTESIAN_POINT('Ctrl Pts',(0.0797651524327904,0.0548975313053337,
-0.462588932126909));
#45230=CARTESIAN_POINT('Ctrl Pts',(0.0978426792144691,0.0286312011979114,
-0.464698152465533));
#45231=CARTESIAN_POINT('Ctrl Pts',(0.101673900093879,-0.00743999983875827,
-0.466807372804157));
#45232=CARTESIAN_POINT('Ctrl Pts',(0.0895170887242362,-0.0369176016607743,
-0.468916593142781));
#45233=CARTESIAN_POINT('Ctrl Pts',(0.0773602773545936,-0.0663952034827903,
-0.471025813481405));
#45234=CARTESIAN_POINT('Ctrl Pts',(0.0492154337359004,-0.0892792060901528,
-0.473135033820029));
#45235=CARTESIAN_POINT('Ctrl Pts',(0.0178775955858247,-0.0951662233259054,
-0.475244254158653));
#45236=CARTESIAN_POINT('Ctrl Pts',(-0.0134602425642505,-0.101053240561658,
-0.477353474497277));
#45237=CARTESIAN_POINT('Ctrl Pts',(-0.0479910752457083,-0.0899432724257991,
-0.479462694835901));
#45238=CARTESIAN_POINT('Ctrl Pts',(-0.0700167052126272,-0.0668870650964328,
-0.481571915174525));
#45239=CARTESIAN_POINT('Ctrl Pts',(-0.0869144608340886,-0.0491986649192516,
-0.483190079553361));
#45240=CARTESIAN_POINT('Ctrl Pts',(-0.096451974205353,-0.0244790141138182,
-0.484808243932196));
#45241=CARTESIAN_POINT('Ctrl Pts',(-0.0966749003444729,8.66157029079557E-5,
-0.486426408311032));
#45242=CARTESIAN_POINT('Ctrl Pts',(-0.096669360704088,8.67233818675543E-5,
-0.492223591688967));
#45243=CARTESIAN_POINT('Ctrl Pts',(-0.0964490169715812,-0.0242970303372613,
-0.490617643073094));
#45244=CARTESIAN_POINT('Ctrl Pts',(-0.0870694389706079,-0.0488317892994789,
-0.489011694457221));
#45245=CARTESIAN_POINT('Ctrl Pts',(-0.0704005799644349,-0.0664829037296246,
-0.487405745841347));
#45246=CARTESIAN_POINT('Ctrl Pts',(-0.0485080386402814,-0.0896655194045322,
-0.485296525502723));
#45247=CARTESIAN_POINT('Ctrl Pts',(-0.0140417333693276,-0.100974080371134,
-0.483187305164099));
#45248=CARTESIAN_POINT('Ctrl Pts',(0.017329473661618,-0.0952675573858311,
-0.481078084825475));
#45249=CARTESIAN_POINT('Ctrl Pts',(0.048700680692564,-0.0895610344005279,
-0.478968864486851));
#45250=CARTESIAN_POINT('Ctrl Pts',(0.0769767894835017,-0.0668394274633188,
-0.476859644148227));
#45251=CARTESIAN_POINT('Ctrl Pts',(0.0893030873420965,-0.0374322953987758,
-0.474750423809603));
#45252=CARTESIAN_POINT('Ctrl Pts',(0.101629385200691,-0.00802516333423281,
-0.472641203470979));
#45253=CARTESIAN_POINT('Ctrl Pts',(0.0980058721269431,0.0280674938576442,
-0.470531983132355));
#45254=CARTESIAN_POINT('Ctrl Pts',(0.0800798476076497,0.0544374517661044,
-0.468422762793731));
#45255=CARTESIAN_POINT('Ctrl Pts',(0.0621538230883563,0.0808074096745646,
-0.466313542455107));
#45256=CARTESIAN_POINT('Ctrl Pts',(0.0299252871235178,0.0974546682996081,
-0.464204322116483));
#45257=CARTESIAN_POINT('Ctrl Pts',(-0.00195421917894117,0.0968111521212923,
-0.462095101777859));
#45258=CARTESIAN_POINT('Ctrl Pts',(-0.0338337254813997,0.0961676359429765,
-0.459985881439235));
#45259=CARTESIAN_POINT('Ctrl Pts',(-0.0653642021214785,0.0782333449613021,
-0.457876661100611));
#45260=CARTESIAN_POINT('Ctrl Pts',(-0.0822114554780782,0.0511614575225072,
-0.455767440761987));
#45261=CARTESIAN_POINT('Ctrl Pts',(-0.0916468729318517,0.0359996650427535,
-0.454586157737647));
#45262=CARTESIAN_POINT('Ctrl Pts',(-0.0964766987464544,0.0179717418073378,
-0.453404874713307));
#45263=CARTESIAN_POINT('Ctrl Pts',(-0.0965281097149038,-3.05597964714245E-5,
-0.452223591688967));
#45264=CARTESIAN_POINT('Origin',(0.,0.,-0.493));
#45265=CARTESIAN_POINT('',(-0.0967741445435993,-6.3845289803563E-5,-0.406426408311032));
#45266=CARTESIAN_POINT('',(-0.0967786908216685,-6.15870636970637E-5,-0.412223591688967));
#45267=CARTESIAN_POINT('',(-0.096675,-1.1839272930757E-17,-0.493));
#45268=CARTESIAN_POINT('Ctrl Pts',(-0.0967741445435993,-6.3845289803563E-5,
-0.406426408311032));
#45269=CARTESIAN_POINT('Ctrl Pts',(-0.096560293855864,0.0279026272071614,
-0.408273486873999));
#45270=CARTESIAN_POINT('Ctrl Pts',(-0.0837582806333823,0.0560398774460321,
-0.410120565436966));
#45271=CARTESIAN_POINT('Ctrl Pts',(-0.0624083797045926,0.0740365627828155,
-0.411967643999934));
#45272=CARTESIAN_POINT('Ctrl Pts',(-0.0380284501393496,0.0945873804368201,
-0.414076864338557));
#45273=CARTESIAN_POINT('Ctrl Pts',(-0.00250218861058814,0.10191503623145,
-0.416186084677181));
#45274=CARTESIAN_POINT('Ctrl Pts',(0.0280196718242732,0.0926882758330654,
-0.418295305015805));
#45275=CARTESIAN_POINT('Ctrl Pts',(0.058541532259135,0.0834615154346805,
-0.420404525354429));
#45276=CARTESIAN_POINT('Ctrl Pts',(0.0840589916000967,0.0576803388432805,
-0.422513745693054));
#45277=CARTESIAN_POINT('Ctrl Pts',(0.0929714575983574,0.0270652278409629,
-0.424622966031678));
#45278=CARTESIAN_POINT('Ctrl Pts',(0.101883923596618,-0.00354988316135429,
-0.426732186370302));
#45279=CARTESIAN_POINT('Ctrl Pts',(0.0941913962521782,-0.038998928574589,
-0.428841406708925));
#45280=CARTESIAN_POINT('Ctrl Pts',(0.0733910055846535,-0.0631662788623783,
-0.430950627047549));
#45281=CARTESIAN_POINT('Ctrl Pts',(0.0525906149171285,-0.087333629150168,
-0.433059847386173));
#45282=CARTESIAN_POINT('Ctrl Pts',(0.0186823609265183,-0.100219284312512,
-0.435169067724798));
#45283=CARTESIAN_POINT('Ctrl Pts',(-0.0129185920811288,-0.0959652461294597,
-0.437278288063422));
#45284=CARTESIAN_POINT('Ctrl Pts',(-0.0445195450887755,-0.0917112079464077,
-0.439387508402046));
#45285=CARTESIAN_POINT('Ctrl Pts',(-0.0738131971134591,-0.0703174764179602,
-0.441496728740669));
#45286=CARTESIAN_POINT('Ctrl Pts',(-0.0874822461434114,-0.041509939722312,
-0.443605949079293));
#45287=CARTESIAN_POINT('Ctrl Pts',(-0.0935750180900934,-0.0286694157730852,
-0.444546102156539));
#45288=CARTESIAN_POINT('Ctrl Pts',(-0.0965635004074205,-0.0143559200944416,
-0.445486255233785));
#45289=CARTESIAN_POINT('Ctrl Pts',(-0.096526423484871,-2.77199618692811E-5,
-0.446426408311032));
#45290=CARTESIAN_POINT('Ctrl Pts',(-0.0965281097149038,-3.05597964714245E-5,
-0.452223591688967));
#45291=CARTESIAN_POINT('Ctrl Pts',(-0.0965684947496539,-0.0141719696508128,
-0.451295654374683));
#45292=CARTESIAN_POINT('Ctrl Pts',(-0.0936602978316979,-0.028297569349907,
-0.4503677170604));
#45293=CARTESIAN_POINT('Ctrl Pts',(-0.0877197475004104,-0.0410056587084708,
-0.449439779746116));
#45294=CARTESIAN_POINT('Ctrl Pts',(-0.0742167560930221,-0.0698914036047387,
-0.447330559407492));
#45295=CARTESIAN_POINT('Ctrl Pts',(-0.0450467432051246,-0.0914534095013585,
-0.445221339068867));
#45296=CARTESIAN_POINT('Ctrl Pts',(-0.0134708027757043,-0.0958892883497912,
-0.443112118730243));
#45297=CARTESIAN_POINT('Ctrl Pts',(0.0181051376537155,-0.100325167198224,
-0.441002898391619));
#45298=CARTESIAN_POINT('Ctrl Pts',(0.0520870056246581,-0.0876349189984701,
-0.438893678052996));
#45299=CARTESIAN_POINT('Ctrl Pts',(0.0730261708908248,-0.0635877072449965,
-0.436784457714372));
#45300=CARTESIAN_POINT('Ctrl Pts',(0.0939653361569919,-0.0395404954915226,
-0.434675237375748));
#45301=CARTESIAN_POINT('Ctrl Pts',(0.101861798718383,-0.00413632018432857,
-0.432566017037124));
#45302=CARTESIAN_POINT('Ctrl Pts',(0.0931257167667431,0.0265295877150718,
-0.4304567966985));
#45303=CARTESIAN_POINT('Ctrl Pts',(0.0843896348151035,0.0571954956144718,
-0.428347576359876));
#45304=CARTESIAN_POINT('Ctrl Pts',(0.0590210083504338,0.0831231361060782,
-0.426238356021252));
#45305=CARTESIAN_POINT('Ctrl Pts',(0.0285527681240471,0.092525442879814,
-0.424129135682628));
#45306=CARTESIAN_POINT('Ctrl Pts',(-0.00191547210233993,0.10192774965355,
-0.422019915344004));
#45307=CARTESIAN_POINT('Ctrl Pts',(-0.0374833260904441,0.0948047227094148,
-0.41991069500538));
#45308=CARTESIAN_POINT('Ctrl Pts',(-0.0619811522718143,0.0743945892569446,
-0.417801474666756));
#45309=CARTESIAN_POINT('Ctrl Pts',(-0.0835761788238258,0.0564028960114691,
-0.415942180340826));
#45310=CARTESIAN_POINT('Ctrl Pts',(-0.0965691724858363,0.0280863752955406,
-0.414082886014897));
#45311=CARTESIAN_POINT('Ctrl Pts',(-0.0967786908216685,-6.15870636970637E-5,
-0.412223591688967));
#45312=CARTESIAN_POINT('Origin',(0.,0.,-0.493));
#45313=CARTESIAN_POINT('',(-0.0967091013458909,8.3442749783804E-5,-0.366426408311032));
#45314=CARTESIAN_POINT('',(-0.096703565001884,8.42524377135991E-5,-0.372223591688967));
#45315=CARTESIAN_POINT('',(-0.096675,-1.1839272930757E-17,-0.493));
#45316=CARTESIAN_POINT('Ctrl Pts',(-0.0967091013458909,8.3442749783804E-5,
-0.366426408311032));
#45317=CARTESIAN_POINT('Ctrl Pts',(-0.0967663269514072,0.0063910955402476,
-0.366842277836965));
#45318=CARTESIAN_POINT('Ctrl Pts',(-0.0962015802620651,0.0126885502496758,
-0.367258147362897));
#45319=CARTESIAN_POINT('Ctrl Pts',(-0.0949773870582177,0.0188550903906585,
-0.36767401688883));
#45320=CARTESIAN_POINT('Ctrl Pts',(-0.0887684848835039,0.0501307455498909,
-0.369783237227454));
#45321=CARTESIAN_POINT('Ctrl Pts',(-0.0655963240856761,0.0780388225458823,
-0.371892457566078));
#45322=CARTESIAN_POINT('Ctrl Pts',(-0.0359952915465715,0.0898919210637069,
-0.374001677904702));
#45323=CARTESIAN_POINT('Ctrl Pts',(-0.00639425900746725,0.101745019581531,
-0.376110898243326));
#45324=CARTESIAN_POINT('Ctrl Pts',(0.0296356452729136,0.0975431396211891,
-0.37822011858195));
#45325=CARTESIAN_POINT('Ctrl Pts',(0.0557147252309796,0.0791965143076565,
-0.380329338920574));
#45326=CARTESIAN_POINT('Ctrl Pts',(0.081793805189046,0.0608498889941236,
-0.382438559259198));
#45327=CARTESIAN_POINT('Ctrl Pts',(0.0979220608247974,0.0283585183273998,
-0.384547779597822));
#45328=CARTESIAN_POINT('Ctrl Pts',(0.0967673626023422,-0.00350656827015149,
-0.386656999936446));
#45329=CARTESIAN_POINT('Ctrl Pts',(0.095612664379887,-0.0353716548677019,
-0.38876622027507));
#45330=CARTESIAN_POINT('Ctrl Pts',(0.0771750122992263,-0.0666104573960799,
-0.390875440613694));
#45331=CARTESIAN_POINT('Ctrl Pts',(0.0498364196695632,-0.0830213813458049,
-0.392984660952318));
#45332=CARTESIAN_POINT('Ctrl Pts',(0.0224978270398989,-0.0994323052955306,
-0.395093881290942));
#45333=CARTESIAN_POINT('Ctrl Pts',(-0.0137417061387687,-0.101015350666602,
-0.397203101629565));
#45334=CARTESIAN_POINT('Ctrl Pts',(-0.0424071835874108,-0.0870508429955163,
-0.399312321968189));
#45335=CARTESIAN_POINT('Ctrl Pts',(-0.071072661036052,-0.0730863353244312,
-0.401421542306813));
#45336=CARTESIAN_POINT('Ctrl Pts',(-0.0921640827546683,-0.0435742746111902,
-0.403530762645437));
#45337=CARTESIAN_POINT('Ctrl Pts',(-0.0960929948131144,-0.01193125449788,
-0.405639982984062));
#45338=CARTESIAN_POINT('Ctrl Pts',(-0.0965812946671128,-0.00799854186101098,
-0.405902124759718));
#45339=CARTESIAN_POINT('Ctrl Pts',(-0.0968044947410041,-0.00403291347466469,
-0.406164266535375));
#45340=CARTESIAN_POINT('Ctrl Pts',(-0.0967741445435993,-6.3845289803563E-5,
-0.406426408311032));
#45341=CARTESIAN_POINT('Ctrl Pts',(-0.0967786908216685,-6.15870636970637E-5,
-0.412223591688967));
#45342=CARTESIAN_POINT('Ctrl Pts',(-0.0968068542391171,-0.0038452311591,
-0.411973665676273));
#45343=CARTESIAN_POINT('Ctrl Pts',(-0.0966040370216943,-0.00762582962604524,
-0.411723739663579));
#45344=CARTESIAN_POINT('Ctrl Pts',(-0.0961600833242075,-0.0113778962349287,
-0.411473813650884));
#45345=CARTESIAN_POINT('Ctrl Pts',(-0.0924133898205945,-0.043043008313528,
-0.40936459331226));
#45346=CARTESIAN_POINT('Ctrl Pts',(-0.071492204438732,-0.0726759925099216,
-0.407255372973636));
#45347=CARTESIAN_POINT('Ctrl Pts',(-0.0429075893001909,-0.0868052816831873,
-0.405146152635012));
#45348=CARTESIAN_POINT('Ctrl Pts',(-0.0143229741616502,-0.100934570856453,
-0.403036932296388));
#45349=CARTESIAN_POINT('Ctrl Pts',(0.02192507073357,-0.0995601650065905,
-0.400927711957764));
#45350=CARTESIAN_POINT('Ctrl Pts',(0.0493576795616014,-0.0833068881662591,
-0.39881849161914));
#45351=CARTESIAN_POINT('Ctrl Pts',(0.0767902883896333,-0.0670536113259275,
-0.396709271280516));
#45352=CARTESIAN_POINT('Ctrl Pts',(0.0954074611504771,-0.035921463495128,
-0.394600050941892));
#45353=CARTESIAN_POINT('Ctrl Pts',(0.0967455719345851,-0.00406355247306422,
-0.392490830603268));
#45354=CARTESIAN_POINT('Ctrl Pts',(0.0980836827186931,0.0277943585489991,
-0.390381610264644));
#45355=CARTESIAN_POINT('Ctrl Pts',(0.0821427315260642,0.0603780327623262,
-0.38827238992602));
#45356=CARTESIAN_POINT('Ctrl Pts',(0.0561696966852534,0.0788744782672949,
-0.386163169587396));
#45357=CARTESIAN_POINT('Ctrl Pts',(0.0301966618444426,0.0973709237722636,
-0.384053949248772));
#45358=CARTESIAN_POINT('Ctrl Pts',(-0.00580845664455006,0.101780140568875,
-0.381944728910148));
#45359=CARTESIAN_POINT('Ctrl Pts',(-0.0354772306839452,0.0900976373200178,
-0.379835508571524));
#45360=CARTESIAN_POINT('Ctrl Pts',(-0.0651460047233408,0.0784151340711604,
-0.3777262882329));
#45361=CARTESIAN_POINT('Ctrl Pts',(-0.0884784343131384,0.050640910776834,
-0.375617067894276));
#45362=CARTESIAN_POINT('Ctrl Pts',(-0.0948672721475454,0.01940151599579,
-0.373507847555652));
#45363=CARTESIAN_POINT('Ctrl Pts',(-0.0961639444012508,0.0130611991048246,
-0.373079762266757));
#45364=CARTESIAN_POINT('Ctrl Pts',(-0.0967626700723313,0.00657814361201625,
-0.372651676977862));
#45365=CARTESIAN_POINT('Ctrl Pts',(-0.096703565001884,8.42524377135991E-5,
-0.372223591688967));
#45366=CARTESIAN_POINT('Origin',(0.,0.,-0.493));
#45367=CARTESIAN_POINT('',(-0.0965197516312923,-9.65577020483471E-6,-0.326426408311032));
#45368=CARTESIAN_POINT('',(-0.0965203932006718,-1.26410680933947E-5,-0.332223591688967));
#45369=CARTESIAN_POINT('',(-0.096675,-1.1839272930757E-17,-0.493));
#45370=CARTESIAN_POINT('Ctrl Pts',(-0.0965197516312923,-9.65577020483471E-6,
-0.326426408311032));
#45371=CARTESIAN_POINT('Ctrl Pts',(-0.0965047840234489,0.0166642787646163,
-0.327520289138554));
#45372=CARTESIAN_POINT('Ctrl Pts',(-0.0924001255268703,0.0333451168327119,
-0.328614169966076));
#45373=CARTESIAN_POINT('Ctrl Pts',(-0.0842483426464452,0.0477329576642131,
-0.329708050793598));
#45374=CARTESIAN_POINT('Ctrl Pts',(-0.0685300799117474,0.0754755835034765,
-0.331817271132222));
#45375=CARTESIAN_POINT('Ctrl Pts',(-0.0377647994695152,0.0946929536920675,
-0.333926491470846));
#45376=CARTESIAN_POINT('Ctrl Pts',(-0.00593882609689562,0.0966485842143444,
-0.33603571180947));
#45377=CARTESIAN_POINT('Ctrl Pts',(0.0258871472757249,0.0986042147366213,
-0.338144932148094));
#45378=CARTESIAN_POINT('Ctrl Pts',(0.0587738135787319,0.083298105592584,
-0.340254152486718));
#45379=CARTESIAN_POINT('Ctrl Pts',(0.0777704364905394,0.0576886270777644,
-0.342363372825342));
#45380=CARTESIAN_POINT('Ctrl Pts',(0.0967670594023461,0.0320791485629459,
-0.344472593163966));
#45381=CARTESIAN_POINT('Ctrl Pts',(0.101873638922953,-0.00383369932265502,
-0.34658181350259));
#45382=CARTESIAN_POINT('Ctrl Pts',(0.0907686529128285,-0.0337234359820715,
-0.348691033841214));
#45383=CARTESIAN_POINT('Ctrl Pts',(0.0796636669027034,-0.0636131726414893,
-0.350800254179838));
#45384=CARTESIAN_POINT('Ctrl Pts',(0.0523471153618471,-0.0874797980747228,
-0.352909474518462));
#45385=CARTESIAN_POINT('Ctrl Pts',(0.0212374828985647,-0.0944732121089336,
-0.355018694857086));
#45386=CARTESIAN_POINT('Ctrl Pts',(-0.00987214956471671,-0.101466626143144,
-0.35712791519571));
#45387=CARTESIAN_POINT('Ctrl Pts',(-0.0447748629504247,-0.0915868287783316,
-0.359237135534334));
#45388=CARTESIAN_POINT('Ctrl Pts',(-0.067603397867478,-0.069325313434689,
-0.361346355872958));
#45389=CARTESIAN_POINT('Ctrl Pts',(-0.0859308895223161,-0.0514530435686153,
-0.363039706685649));
#45390=CARTESIAN_POINT('Ctrl Pts',(-0.0964760882983722,-0.0256002592597677,
-0.364733057498341));
#45391=CARTESIAN_POINT('Ctrl Pts',(-0.0967091013458909,8.3442749783804E-5,
-0.366426408311032));
#45392=CARTESIAN_POINT('Ctrl Pts',(-0.096703565001884,8.42524377135991E-5,
-0.372223591688967));
#45393=CARTESIAN_POINT('Ctrl Pts',(-0.0964714532986248,-0.0254179274910308,
-0.370542456639238));
#45394=CARTESIAN_POINT('Ctrl Pts',(-0.0860941848055461,-0.0510872168002652,
-0.368861321589509));
#45395=CARTESIAN_POINT('Ctrl Pts',(-0.0680013484513945,-0.0689350038546699,
-0.36718018653978));
#45396=CARTESIAN_POINT('Ctrl Pts',(-0.0453013408418207,-0.0913275626563238,
-0.365070966201156));
#45397=CARTESIAN_POINT('Ctrl Pts',(-0.0104560795436565,-0.101408113991871,
-0.362961745862532));
#45398=CARTESIAN_POINT('Ctrl Pts',(0.0206932945708154,-0.0945938988912964,
-0.360852525523908));
#45399=CARTESIAN_POINT('Ctrl Pts',(0.0518426686852874,-0.0877796837907218,
-0.358743305185284));
#45400=CARTESIAN_POINT('Ctrl Pts',(0.0792961556160677,-0.0640707022540251,
-0.35663408484666));
#45401=CARTESIAN_POINT('Ctrl Pts',(0.090573018020292,-0.0342453873440962,
-0.354524864508036));
#45402=CARTESIAN_POINT('Ctrl Pts',(0.101849880424517,-0.00442007243416647,
-0.352415644169412));
#45403=CARTESIAN_POINT('Ctrl Pts',(0.096950118302185,0.0315215758489951,
-0.350306423830788));
#45404=CARTESIAN_POINT('Ctrl Pts',(0.0781012317244362,0.0572399838467591,
-0.348197203492164));
#45405=CARTESIAN_POINT('Ctrl Pts',(0.059252345146688,0.0829583918445225,
-0.34608798315354));
#45406=CARTESIAN_POINT('Ctrl Pts',(0.026454334113523,0.098453559556888,
-0.343978762814916));
#45407=CARTESIAN_POINT('Ctrl Pts',(-0.00538236897332435,0.0966811680312477,
-0.341869542476292));
#45408=CARTESIAN_POINT('Ctrl Pts',(-0.0372190720601721,0.0949087765056073,
-0.339760322137668));
#45409=CARTESIAN_POINT('Ctrl Pts',(-0.0680944672007028,0.0758688257419608,
-0.337651101799044));
#45410=CARTESIAN_POINT('Ctrl Pts',(-0.083972169942999,0.0482171424154877,
-0.33554188146042));
#45411=CARTESIAN_POINT('Ctrl Pts',(-0.0922985986931762,0.0337163185383023,
-0.334435784869936));
#45412=CARTESIAN_POINT('Ctrl Pts',(-0.0965005716954632,0.0168472163336972,
-0.333329688279452));
#45413=CARTESIAN_POINT('Ctrl Pts',(-0.0965203932006718,-1.26410680933947E-5,
-0.332223591688967));
#45414=CARTESIAN_POINT('Origin',(0.,0.,-0.493));
#45415=CARTESIAN_POINT('',(-0.0967437690459326,-7.5552805846299E-5,-0.286426408311032));
#45416=CARTESIAN_POINT('',(-0.0967489390155672,-7.39178419271937E-5,-0.292223591688967));
#45417=CARTESIAN_POINT('',(-0.096675,-1.1839272930757E-17,-0.493));
#45418=CARTESIAN_POINT('Ctrl Pts',(-0.0967437690459326,-7.5552805846299E-5,
-0.286426408311032));
#45419=CARTESIAN_POINT('Ctrl Pts',(-0.0965129181057634,0.0267745038977835,
-0.288198300440143));
#45420=CARTESIAN_POINT('Ctrl Pts',(-0.0848482692534772,0.05380059796138,
-0.289970192569255));
#45421=CARTESIAN_POINT('Ctrl Pts',(-0.0649918357452926,0.0717793826422552,
-0.291742084698366));
#45422=CARTESIAN_POINT('Ctrl Pts',(-0.0413551861322041,0.0931809215337106,
-0.29385130503699));
#45423=CARTESIAN_POINT('Ctrl Pts',(-0.00611079122009462,0.101762438004232,
-0.295960525375614));
#45424=CARTESIAN_POINT('Ctrl Pts',(0.024718756421455,0.0936226552017361,
-0.298069745714238));
#45425=CARTESIAN_POINT('Ctrl Pts',(0.0555483040630038,0.0854828723992403,
-0.300178966052862));
#45426=CARTESIAN_POINT('Ctrl Pts',(0.0819630044339925,0.0606217903237279,
-0.302288186391486));
#45427=CARTESIAN_POINT('Ctrl Pts',(0.0919543670227436,0.0303416029815987,
-0.30439740673011));
#45428=CARTESIAN_POINT('Ctrl Pts',(0.101945729611495,6.14156394686538E-5,
-0.306506627068734));
#45429=CARTESIAN_POINT('Ctrl Pts',(0.0955137544180066,-0.0356378769692795,
-0.308615847407358));
#45430=CARTESIAN_POINT('Ctrl Pts',(0.0755825069057357,-0.0605268794494711,
-0.310725067745982));
#45431=CARTESIAN_POINT('Ctrl Pts',(0.055651259393465,-0.0854158819296624,
-0.312834288084606));
#45432=CARTESIAN_POINT('Ctrl Pts',(0.0222207395624123,-0.0994945942812985,
-0.31494350842323));
#45433=CARTESIAN_POINT('Ctrl Pts',(-0.00951107288091885,-0.0963626378774484,
-0.317052728761854));
#45434=CARTESIAN_POINT('Ctrl Pts',(-0.0412428853242505,-0.0932306814735982,
-0.319161949100478));
#45435=CARTESIAN_POINT('Ctrl Pts',(-0.0712759903798599,-0.0728880563142611,
-0.321271169439102));
#45436=CARTESIAN_POINT('Ctrl Pts',(-0.0859569203940831,-0.0445828029896242,
-0.323380389777726));
#45437=CARTESIAN_POINT('Ctrl Pts',(-0.093024047535901,-0.0309571795561787,
-0.324395729288828));
#45438=CARTESIAN_POINT('Ctrl Pts',(-0.0965336445556838,-0.0154863915468829,
-0.32541106879993));
#45439=CARTESIAN_POINT('Ctrl Pts',(-0.0965197516312923,-9.65577020483471E-6,
-0.326426408311032));
#45440=CARTESIAN_POINT('Ctrl Pts',(-0.0965203932006718,-1.26410680933947E-5,
-0.332223591688967));
#45441=CARTESIAN_POINT('Ctrl Pts',(-0.0965383694088707,-0.0153029181519232,
-0.331220467940828));
#45442=CARTESIAN_POINT('Ctrl Pts',(-0.0931166288935622,-0.0305855916128645,
-0.330217344192688));
#45443=CARTESIAN_POINT('Ctrl Pts',(-0.0862121360220177,-0.0440872515606547,
-0.329214220444548));
#45444=CARTESIAN_POINT('Ctrl Pts',(-0.0716943890146783,-0.072476546321024,
-0.327105000105924));
#45445=CARTESIAN_POINT('Ctrl Pts',(-0.0417788846559379,-0.0929917199524636,
-0.3249957797673));
#45446=CARTESIAN_POINT('Ctrl Pts',(-0.0100656276855269,-0.0963062889272953,
-0.322886559428676));
#45447=CARTESIAN_POINT('Ctrl Pts',(0.0216476292848846,-0.0996208579021272,
-0.320777339090052));
#45448=CARTESIAN_POINT('Ctrl Pts',(0.0551586388669668,-0.0857348222203507,
-0.318668118751428));
#45449=CARTESIAN_POINT('Ctrl Pts',(0.0752328295928874,-0.0609609670124983,
-0.316558898412804));
#45450=CARTESIAN_POINT('Ctrl Pts',(0.0953070203188076,-0.0361871118046462,
-0.31444967807418));
#45451=CARTESIAN_POINT('Ctrl Pts',(0.101944392188567,-0.000525437070718525,
-0.312340457735557));
#45452=CARTESIAN_POINT('Ctrl Pts',(0.0921275035503174,0.02981176340369,
-0.310231237396933));
#45453=CARTESIAN_POINT('Ctrl Pts',(0.0823106149120679,0.0601489638780991,
-0.308122017058309));
#45454=CARTESIAN_POINT('Ctrl Pts',(0.0560394657658096,0.0851616900929888,
-0.306012796719685));
#45455=CARTESIAN_POINT('Ctrl Pts',(0.0252572862380605,0.0934788085051367,
-0.30390357638106));
#45456=CARTESIAN_POINT('Ctrl Pts',(-0.00552489328968782,0.101795926917284,
-0.301794356042436));
#45457=CARTESIAN_POINT('Ctrl Pts',(-0.0408181031989268,0.0934174375266914,
-0.299685135703812));
#45458=CARTESIAN_POINT('Ctrl Pts',(-0.0645775589428199,0.0721523182485355,
-0.297575915365188));
#45459=CARTESIAN_POINT('Ctrl Pts',(-0.0846747634538068,0.0541649764638451,
-0.295791807473115));
#45460=CARTESIAN_POINT('Ctrl Pts',(-0.0965197817739755,0.0269574911179326,
-0.294007699581041));
#45461=CARTESIAN_POINT('Ctrl Pts',(-0.0967489390155672,-7.39178419271937E-5,
-0.292223591688967));
#45462=CARTESIAN_POINT('Origin',(0.,0.,-0.493));
#45463=CARTESIAN_POINT('',(-0.0967423356012983,7.59830402560519E-5,-0.246426408311031));
#45464=CARTESIAN_POINT('',(-0.0967370704137262,7.74805285259637E-5,-0.252223591688967));
#45465=CARTESIAN_POINT('',(-0.096675,-1.1839272930757E-17,-0.493));
#45466=CARTESIAN_POINT('Ctrl Pts',(-0.0967423356012983,7.59830402560519E-5,
-0.246426408311031));
#45467=CARTESIAN_POINT('Ctrl Pts',(-0.0967868821729931,0.00523866323318436,
-0.246767091403108));
#45468=CARTESIAN_POINT('Ctrl Pts',(-0.096408980193914,0.0103948133764852,
-0.247107774495185));
#45469=CARTESIAN_POINT('Ctrl Pts',(-0.0955856895060027,0.0154788387067367,
-0.247448457587262));
#45470=CARTESIAN_POINT('Ctrl Pts',(-0.0904885728485377,0.046954805310395,
-0.249557677925886));
#45471=CARTESIAN_POINT('Ctrl Pts',(-0.0683195528466901,0.0756662028697691,
-0.251666898264511));
#45472=CARTESIAN_POINT('Ctrl Pts',(-0.0391569746115824,0.0885604303586767,
-0.253776118603135));
#45473=CARTESIAN_POINT('Ctrl Pts',(-0.00999439637647477,0.101454657847584,
-0.255885338941759));
#45474=CARTESIAN_POINT('Ctrl Pts',(0.0261617400918925,0.0985317152660251,
-0.257994559280382));
#45475=CARTESIAN_POINT('Ctrl Pts',(0.0528743518199786,0.0811204130022984,
-0.260103779619006));
#45476=CARTESIAN_POINT('Ctrl Pts',(0.0795869635480646,0.0637091107385717,
-0.26221299995763));
#45477=CARTESIAN_POINT('Ctrl Pts',(0.0968560505358691,0.0318094487926776,
-0.264322220296255));
#45478=CARTESIAN_POINT('Ctrl Pts',(0.0968308454331686,-7.65424347751696E-5,
-0.266431440634879));
#45479=CARTESIAN_POINT('Ctrl Pts',(0.0968056403304681,-0.031962533662227,
-0.268540660973503));
#45480=CARTESIAN_POINT('Ctrl Pts',(0.0794861431372628,-0.0638348541712385,
-0.270649881312126));
#45481=CARTESIAN_POINT('Ctrl Pts',(0.0527460383849185,-0.0812039033590322,
-0.27275910165075));
#45482=CARTESIAN_POINT('Ctrl Pts',(0.0260059336325734,-0.0985729525468265,
-0.274868321989374));
#45483=CARTESIAN_POINT('Ctrl Pts',(-0.0101547786789113,-0.101438730413403,
-0.276977542327999));
#45484=CARTESIAN_POINT('Ctrl Pts',(-0.0392969353340071,-0.0884984144456908,
-0.279086762666623));
#45485=CARTESIAN_POINT('Ctrl Pts',(-0.0684390919891021,-0.0755580984779786,
-0.281195983005247));
#45486=CARTESIAN_POINT('Ctrl Pts',(-0.0905626929878082,-0.0468116886759782,
-0.28330520334387));
#45487=CARTESIAN_POINT('Ctrl Pts',(-0.0956100413301282,-0.015327703118784,
-0.285414423682494));
#45488=CARTESIAN_POINT('Ctrl Pts',(-0.0964172651881209,-0.0102924603412303,
-0.285751751892007));
#45489=CARTESIAN_POINT('Ctrl Pts',(-0.0967877178467835,-0.00518719668322276,
-0.286089080101519));
#45490=CARTESIAN_POINT('Ctrl Pts',(-0.0967437690459326,-7.5552805846299E-5,
-0.286426408311032));
#45491=CARTESIAN_POINT('Ctrl Pts',(-0.0967489390155672,-7.39178419271937E-5,
-0.292223591688967));
#45492=CARTESIAN_POINT('Ctrl Pts',(-0.0967906976288156,-0.00499976764040804,
-0.291898479242417));
#45493=CARTESIAN_POINT('Ctrl Pts',(-0.0964467324983444,-0.00991977053332167,
-0.291573366795867));
#45494=CARTESIAN_POINT('Ctrl Pts',(-0.0956966895450183,-0.0147770686462416,
-0.291248254349317));
#45495=CARTESIAN_POINT('Ctrl Pts',(-0.0908306628247752,-0.0462895870971385,
-0.289139034010693));
#45496=CARTESIAN_POINT('Ctrl Pts',(-0.0688729078057432,-0.0751628748332125,
-0.287029813672068));
#45497=CARTESIAN_POINT('Ctrl Pts',(-0.0398057255967931,-0.0882707333002516,
-0.284920593333444));
#45498=CARTESIAN_POINT('Ctrl Pts',(-0.0107385433878433,-0.101378591767291,
-0.28281137299482));
#45499=CARTESIAN_POINT('Ctrl Pts',(0.0254380660110247,-0.0987210209652953,
-0.280702152656197));
#45500=CARTESIAN_POINT('Ctrl Pts',(0.0522777123470515,-0.0815061895772969,
-0.278592932317573));
#45501=CARTESIAN_POINT('Ctrl Pts',(0.0791173586830794,-0.0642913581892978,
-0.276483711978949));
#45502=CARTESIAN_POINT('Ctrl Pts',(0.0966200419562655,-0.0325192662152939,
-0.274374491640325));
#45503=CARTESIAN_POINT('Ctrl Pts',(0.0968287986931256,-0.000633948970751547,
-0.272265271301701));
#45504=CARTESIAN_POINT('Ctrl Pts',(0.0970375554299856,0.0312513682737899,
-0.270156050963076));
#45505=CARTESIAN_POINT('Ctrl Pts',(0.0799523856305208,0.0632499107888704,
-0.268046830624453));
#45506=CARTESIAN_POINT('Ctrl Pts',(0.0533404453307932,0.0808146956905983,
-0.265937610285829));
#45507=CARTESIAN_POINT('Ctrl Pts',(0.0267285050310652,0.0983794805923265,
-0.263828389947205));
#45508=CARTESIAN_POINT('Ctrl Pts',(-0.00941020576892441,0.101510507880702,
-0.261719169608581));
#45509=CARTESIAN_POINT('Ctrl Pts',(-0.0386465260470608,0.0887843689629269,
-0.259609949269957));
#45510=CARTESIAN_POINT('Ctrl Pts',(-0.0678828463251972,0.076058230045152,
-0.257500728931333));
#45511=CARTESIAN_POINT('Ctrl Pts',(-0.0902167760814793,0.0474749249212259,
-0.255391508592709));
#45512=CARTESIAN_POINT('Ctrl Pts',(-0.0954949999346953,0.016028822012986,
-0.253282288254085));
#45513=CARTESIAN_POINT('Ctrl Pts',(-0.0963781125807907,0.0107674970065134,
-0.252929389399046));
#45514=CARTESIAN_POINT('Ctrl Pts',(-0.0967837769872234,0.00542603238163979,
-0.252576490544006));
#45515=CARTESIAN_POINT('Ctrl Pts',(-0.0967370704137262,7.74805285259636E-5,
-0.252223591688967));
#45516=CARTESIAN_POINT('Origin',(0.,0.,-0.493));
#45517=CARTESIAN_POINT('',(-0.096519605166994,8.83378289982806E-6,-0.206426408311032));
#45518=CARTESIAN_POINT('',(-0.0965191803594238,5.8347464585056E-6,-0.212223591688967));
#45519=CARTESIAN_POINT('',(-0.096675,-1.1839272930757E-17,-0.493));
#45520=CARTESIAN_POINT('Ctrl Pts',(-0.096519605166994,8.83378289982806E-6,
-0.206426408311032));
#45521=CARTESIAN_POINT('Ctrl Pts',(-0.0965323562986513,0.0155367666085817,
-0.207445102704698));
#45522=CARTESIAN_POINT('Ctrl Pts',(-0.0929984118487813,0.0310592225023218,
-0.208463797098364));
#45523=CARTESIAN_POINT('Ctrl Pts',(-0.085886329768773,0.0447186409110356,
-0.209482491492031));
#45524=CARTESIAN_POINT('Ctrl Pts',(-0.0711606688969908,0.0730006490388526,
-0.211591711830655));
#45525=CARTESIAN_POINT('Ctrl Pts',(-0.0410954406900119,0.0932957679232711,
-0.213700932169279));
#45526=CARTESIAN_POINT('Ctrl Pts',(-0.00935871643388856,0.0963775539882049,
-0.215810152507903));
#45527=CARTESIAN_POINT('Ctrl Pts',(0.0223780078222335,0.0994593400531385,
-0.217919372846527));
#45528=CARTESIAN_POINT('Ctrl Pts',(0.0557862281274994,0.0853277932985902,
-0.220028593185151));
#45529=CARTESIAN_POINT('Ctrl Pts',(0.0756781024505724,0.0604073116064739,
-0.222137813523775));
#45530=CARTESIAN_POINT('Ctrl Pts',(0.0955699767736457,0.0354868299143573,
-0.224247033862399));
#45531=CARTESIAN_POINT('Ctrl Pts',(0.101945505114525,-0.000222586715327797,
-0.226356254201023));
#45532=CARTESIAN_POINT('Ctrl Pts',(0.0919062835345921,-0.0304869403665019,
-0.228465474539647));
#45533=CARTESIAN_POINT('Ctrl Pts',(0.081867061954659,-0.0607512940176778,
-0.230574694878271));
#45534=CARTESIAN_POINT('Ctrl Pts',(0.0554130904539123,-0.0855705846903427,
-0.232683915216895));
#45535=CARTESIAN_POINT('Ctrl Pts',(0.0245707127464045,-0.0936616173316404,
-0.234793135555519));
#45536=CARTESIAN_POINT('Ctrl Pts',(-0.00627166496110106,-0.101752649972938,
-0.236902355894143));
#45537=CARTESIAN_POINT('Ctrl Pts',(-0.0415024488753662,-0.0931154245828709,
-0.239011576232767));
#45538=CARTESIAN_POINT('Ctrl Pts',(-0.065105234175958,-0.0716765440638671,
-0.241120796571391));
#45539=CARTESIAN_POINT('Ctrl Pts',(-0.084895677195098,-0.0537004900557472,
-0.242889333817938));
#45540=CARTESIAN_POINT('Ctrl Pts',(-0.0965110876377789,-0.0267242674727368,
-0.244657871064485));
#45541=CARTESIAN_POINT('Ctrl Pts',(-0.0967423356012983,7.59830402560519E-5,
-0.246426408311031));
#45542=CARTESIAN_POINT('Ctrl Pts',(-0.0967370704137262,7.74805285259636E-5,
-0.252223591688967));
#45543=CARTESIAN_POINT('Ctrl Pts',(-0.0965046192247059,-0.0265414115181691,
-0.250467270205382));
#45544=CARTESIAN_POINT('Ctrl Pts',(-0.08506741559802,-0.0533358467394369,
-0.248710948721798));
#45545=CARTESIAN_POINT('Ctrl Pts',(-0.065516761081115,-0.0713005761904585,
-0.246954627238213));
#45546=CARTESIAN_POINT('Ctrl Pts',(-0.0420377804241679,-0.0928749707931102,
-0.244845406899589));
#45547=CARTESIAN_POINT('Ctrl Pts',(-0.00685730116012349,-0.101714859305859,
-0.242736186560965));
#45548=CARTESIAN_POINT('Ctrl Pts',(0.0240311410848332,-0.0938015053493915,
-0.240626966222341));
#45549=CARTESIAN_POINT('Ctrl Pts',(0.0549195833297894,-0.0858881513929241,
-0.238517745883717));
#45550=CARTESIAN_POINT('Ctrl Pts',(0.0815159885556585,-0.0612215549672399,
-0.236408525545093));
#45551=CARTESIAN_POINT('Ctrl Pts',(0.0917292606941796,-0.0310154941948588,
-0.234299305206469));
#45552=CARTESIAN_POINT('Ctrl Pts',(0.101942532832701,-0.000809433422477208,
-0.232190084867845));
#45553=CARTESIAN_POINT('Ctrl Pts',(0.0957726718838747,0.0349360916966021,
-0.230080864529221));
#45554=CARTESIAN_POINT('Ctrl Pts',(0.0760245825266243,0.0599706678243891,
-0.227971644190597));
#45555=CARTESIAN_POINT('Ctrl Pts',(0.0562764931693742,0.0850052439521758,
-0.225862423851973));
#45556=CARTESIAN_POINT('Ctrl Pts',(0.0229501754037008,0.0993288710886704,
-0.223753203513349));
#45557=CARTESIAN_POINT('Ctrl Pts',(-0.00880376277346886,0.0964298289362705,
-0.221643983174725));
#45558=CARTESIAN_POINT('Ctrl Pts',(-0.0405577009506385,0.0935307867838707,
-0.219534762836101));
#45559=CARTESIAN_POINT('Ctrl Pts',(-0.0707392595393038,0.0734090753425766,
-0.217425542497477));
#45560=CARTESIAN_POINT('Ctrl Pts',(-0.0856274818429496,0.0452123047509388,
-0.215316322158853));
#45561=CARTESIAN_POINT('Ctrl Pts',(-0.0929043031905888,0.0314307492373925,
-0.214285412002224));
#45562=CARTESIAN_POINT('Ctrl Pts',(-0.0965277014070608,0.0157201438856951,
-0.213254501845596));
#45563=CARTESIAN_POINT('Ctrl Pts',(-0.0965191803594238,5.8347464585056E-6,
-0.212223591688967));
#45564=CARTESIAN_POINT('Origin',(0.,0.,-0.493));
#45565=CARTESIAN_POINT('',(-0.0967106172141971,-8.32004823464877E-5,-0.166426408311032));
#45566=CARTESIAN_POINT('',(-0.0967161166967018,-8.22460629427947E-5,-0.172223591688967));
#45567=CARTESIAN_POINT('',(-0.096675,-1.1839272930757E-17,-0.493));
#45568=CARTESIAN_POINT('Ctrl Pts',(-0.0967106172141971,-8.32004823464877E-5,
-0.166426408311032));
#45569=CARTESIAN_POINT('Ctrl Pts',(-0.0964774108677986,0.025650346436811,
-0.168123114006287));
#45570=CARTESIAN_POINT('Ctrl Pts',(-0.0858858039544249,0.0515534804917154,
-0.169819819701543));
#45571=CARTESIAN_POINT('Ctrl Pts',(-0.0674937135020625,0.0694321044270534,
-0.171516525396799));
#45572=CARTESIAN_POINT('Ctrl Pts',(-0.0446300127669237,0.0916575011687899,
-0.173625745735423));
#45573=CARTESIAN_POINT('Ctrl Pts',(-0.00971172351316946,0.101482106719653,
-0.175734966074047));
#45574=CARTESIAN_POINT('Ctrl Pts',(0.0213868138345207,0.0944395186348712,
-0.177844186412671));
#45575=CARTESIAN_POINT('Ctrl Pts',(0.0524853511822118,0.0873969305500895,
-0.179953406751295));
#45576=CARTESIAN_POINT('Ctrl Pts',(0.079764136623838,0.0634871488296626,
-0.182062627089919));
#45577=CARTESIAN_POINT('Ctrl Pts',(0.0908218545598657,0.0335798930909097,
-0.184171847428543));
#45578=CARTESIAN_POINT('Ctrl Pts',(0.101879572495893,0.00367263735215799,
-0.186281067767167));
#45579=CARTESIAN_POINT('Ctrl Pts',(0.0967162229263223,-0.0322320924049201,
-0.188390288105791));
#45580=CARTESIAN_POINT('Ctrl Pts',(0.0776791364377021,-0.0578115061952451,
-0.190499508444415));
#45581=CARTESIAN_POINT('Ctrl Pts',(0.0586420499490815,-0.0833909199855704,
-0.192608728783039));
#45582=CARTESIAN_POINT('Ctrl Pts',(0.0257312265414111,-0.0986450178091434,
-0.194717949121663));
#45583=CARTESIAN_POINT('Ctrl Pts',(-0.00609161530366864,-0.0966390744420128,
-0.196827169460287));
#45584=CARTESIAN_POINT('Ctrl Pts',(-0.0379144571487484,-0.0946331310748821,
-0.198936389798911));
#45585=CARTESIAN_POINT('Ctrl Pts',(-0.0686493174312371,-0.0753671465170478,
-0.201045610137535));
#45586=CARTESIAN_POINT('Ctrl Pts',(-0.0843237008041889,-0.0475997055525231,
-0.203154830476159));
#45587=CARTESIAN_POINT('Ctrl Pts',(-0.0924277956805772,-0.0332431614578228,
-0.204245356421116));
#45588=CARTESIAN_POINT('Ctrl Pts',(-0.0965059549103652,-0.0166140255586733,
-0.205335882366074));
#45589=CARTESIAN_POINT('Ctrl Pts',(-0.096519605166994,8.83378289982806E-6,
-0.206426408311032));
#45590=CARTESIAN_POINT('Ctrl Pts',(-0.0965191803594238,5.8347464585056E-6,
-0.212223591688967));
#45591=CARTESIAN_POINT('Ctrl Pts',(-0.0965102675241303,-0.0164309996749581,
-0.211145281506972));
#45592=CARTESIAN_POINT('Ctrl Pts',(-0.0925277746875275,-0.0328718863054202,
-0.210066971324976));
#45593=CARTESIAN_POINT('Ctrl Pts',(-0.0845963103545643,-0.0471135057286142,
-0.208988661142981));
#45594=CARTESIAN_POINT('Ctrl Pts',(-0.0690820305439074,-0.0749707158745457,
-0.206879440804357));
#45595=CARTESIAN_POINT('Ctrl Pts',(-0.0384585849039681,-0.0944133064244279,
-0.204770220465733));
#45596=CARTESIAN_POINT('Ctrl Pts',(-0.00664781813597963,-0.096602405051195,
-0.202661000127109));
#45597=CARTESIAN_POINT('Ctrl Pts',(0.0251629486320089,-0.0987915036779621,
-0.200551779788485));
#45598=CARTESIAN_POINT('Ctrl Pts',(0.0581610365280471,-0.083727110381614,
-0.198442559449861));
#45599=CARTESIAN_POINT('Ctrl Pts',(0.0773450554226922,-0.0582577080680854,
-0.196333339111237));
#45600=CARTESIAN_POINT('Ctrl Pts',(0.096529074317338,-0.0327883057545557,
-0.194224118772613));
#45601=CARTESIAN_POINT('Ctrl Pts',(0.10189902421059,0.00308610557615446,
-0.192114898433989));
#45602=CARTESIAN_POINT('Ctrl Pts',(0.0910136511261294,0.0330565191194918,
-0.190005678095365));
#45603=CARTESIAN_POINT('Ctrl Pts',(0.0801282780416693,0.063026932662828,
-0.187896457756741));
#45604=CARTESIAN_POINT('Ctrl Pts',(0.0529875819794976,0.087093348418791,
-0.185787237418117));
#45605=CARTESIAN_POINT('Ctrl Pts',(0.0219301011972353,0.0943148387535103,
-0.183678017079493));
#45606=CARTESIAN_POINT('Ctrl Pts',(-0.00912737958502692,0.10153632908823,
-0.181568796740869));
#45607=CARTESIAN_POINT('Ctrl Pts',(-0.0441016450873802,0.0919128940017052,
-0.179459576402245));
#45608=CARTESIAN_POINT('Ctrl Pts',(-0.0670929073267039,0.0698194810516787,
-0.177350356063621));
#45609=CARTESIAN_POINT('Ctrl Pts',(-0.08572076742876,0.0519190716993752,
-0.175641434605403));
#45610=CARTESIAN_POINT('Ctrl Pts',(-0.0964824094446633,0.0258327707762626,
-0.173932513147185));
#45611=CARTESIAN_POINT('Ctrl Pts',(-0.0967161166967018,-8.22460629427947E-5,
-0.172223591688967));
#45612=CARTESIAN_POINT('Origin',(0.,0.,-0.493));
#45613=CARTESIAN_POINT('',(-0.0967728733759203,6.44486977623322E-5,-0.126426408311032));
#45614=CARTESIAN_POINT('',(-0.0967681696808917,6.65845257773007E-5,-0.132223591688967));
#45615=CARTESIAN_POINT('',(-0.096675,-1.1839272930757E-17,-0.493));
#45616=CARTESIAN_POINT('Ctrl Pts',(-0.0967728733759203,6.44486977623322E-5,
-0.126426408311032));
#45617=CARTESIAN_POINT('Ctrl Pts',(-0.0968038274783861,0.0040844511009329,
-0.126691904969253));
#45618=CARTESIAN_POINT('Ctrl Pts',(-0.0965748568526,0.00810090112065628,
-0.126957401627474));
#45619=CARTESIAN_POINT('Ctrl Pts',(-0.0960740112983165,0.0120831576363327,
-0.127222898285695));
#45620=CARTESIAN_POINT('Ctrl Pts',(-0.0920950774891978,0.0437199265989198,
-0.129332118624319));
#45621=CARTESIAN_POINT('Ctrl Pts',(-0.0709570263862882,0.0731986063626649,
-0.131441338962943));
#45622=CARTESIAN_POINT('Ctrl Pts',(-0.0422695078882135,0.0871177779818565,
-0.133550559301567));
#45623=CARTESIAN_POINT('Ctrl Pts',(-0.0135819893901388,0.101036949601048,
-0.135659779640191));
#45624=CARTESIAN_POINT('Ctrl Pts',(0.0226549965031015,0.0993966130756864,
-0.137768999978815));
#45625=CARTESIAN_POINT('Ctrl Pts',(0.0499676102792677,0.0829424886199023,
-0.139878220317439));
#45626=CARTESIAN_POINT('Ctrl Pts',(0.0772802240554347,0.0664883641641178,
-0.141987440656063));
#45627=CARTESIAN_POINT('Ctrl Pts',(0.0956684657145276,0.0352204517779098,
-0.144096660994687));
#45628=CARTESIAN_POINT('Ctrl Pts',(0.0967727852795511,0.00335357950948155,
-0.146205881333311));
#45629=CARTESIAN_POINT('Ctrl Pts',(0.0978771048445746,-0.0285132927589462,
-0.148315101671935));
#45630=CARTESIAN_POINT('Ctrl Pts',(0.0816975023155301,-0.0609791249095938,
-0.150424322010559));
#45631=CARTESIAN_POINT('Ctrl Pts',(0.0555894498893144,-0.0792844975754325,
-0.152533542349183));
#45632=CARTESIAN_POINT('Ctrl Pts',(0.0294813974630983,-0.0975898702412715,
-0.154642762687807));
#45633=CARTESIAN_POINT('Ctrl Pts',(-0.00655510486028936,-0.1017347834223,
-0.156751983026431));
#45634=CARTESIAN_POINT('Ctrl Pts',(-0.0361373612697451,-0.0898349019422432,
-0.158861203365055));
#45635=CARTESIAN_POINT('Ctrl Pts',(-0.0657196176792,-0.0779350204621864,
-0.160970423703679));
#45636=CARTESIAN_POINT('Ctrl Pts',(-0.0888476281747239,-0.0499903443210447,
-0.163079644042303));
#45637=CARTESIAN_POINT('Ctrl Pts',(-0.0950070773142242,-0.0187049122841689,
-0.165188864380927));
#45638=CARTESIAN_POINT('Ctrl Pts',(-0.096211722897522,-0.0125862064273259,
-0.165601379024295));
#45639=CARTESIAN_POINT('Ctrl Pts',(-0.0967673159292923,-0.00633971565739204,
-0.166013893667664));
#45640=CARTESIAN_POINT('Ctrl Pts',(-0.0967106172141971,-8.32004823464877E-5,
-0.166426408311032));
#45641=CARTESIAN_POINT('Ctrl Pts',(-0.0967161166967018,-8.22460629427947E-5,
-0.172223591688967));
#45642=CARTESIAN_POINT('Ctrl Pts',(-0.0967708604363183,-0.00615259656181894,
-0.171823292808561));
#45643=CARTESIAN_POINT('Ctrl Pts',(-0.0962479502491979,-0.0122135489284046,
-0.171422993928155));
#45644=CARTESIAN_POINT('Ctrl Pts',(-0.0951131764843987,-0.0181576927593301,
-0.171022695047749));
#45645=CARTESIAN_POINT('Ctrl Pts',(-0.0891339244264755,-0.0494780628067843,
-0.168913474709125));
#45646=CARTESIAN_POINT('Ctrl Pts',(-0.066167161334334,-0.0775554120881626,
-0.166804254370501));
#45647=CARTESIAN_POINT('Ctrl Pts',(-0.0366538974200273,-0.0896253867579126,
-0.164695034031877));
#45648=CARTESIAN_POINT('Ctrl Pts',(-0.00714063350572054,-0.101695361427663,
-0.162585813693253));
#45649=CARTESIAN_POINT('Ctrl Pts',(0.0289191312307513,-0.0977579614857844,
-0.160476593354629));
#45650=CARTESIAN_POINT('Ctrl Pts',(0.0551321257213364,-0.0796031837461425,
-0.158367373016005));
#45651=CARTESIAN_POINT('Ctrl Pts',(0.0813451202119191,-0.0614484060065022,
-0.156258152677381));
#45652=CARTESIAN_POINT('Ctrl Pts',(0.097711344456617,-0.0290762504691009,
-0.154148932338757));
#45653=CARTESIAN_POINT('Ctrl Pts',(0.0967904851253458,0.00279645027672639,
-0.152039712000134));
#45654=CARTESIAN_POINT('Ctrl Pts',(0.0958696257940746,0.0346691510225565,
-0.14993049166151));
#45655=CARTESIAN_POINT('Ctrl Pts',(0.0776616828868309,0.0660423969768126,
-0.147821271322886));
#45656=CARTESIAN_POINT('Ctrl Pts',(0.0504442406332896,0.0826534738232335,
-0.145712050984262));
#45657=CARTESIAN_POINT('Ctrl Pts',(0.0232267983797483,0.0992645506696545,
-0.143602830645638));
#45658=CARTESIAN_POINT('Ctrl Pts',(-0.0130001432200904,0.10111345840824,
-0.141493610307013));
#45659=CARTESIAN_POINT('Ctrl Pts',(-0.0417673120207193,0.0873596577544192,
-0.139384389968389));
#45660=CARTESIAN_POINT('Ctrl Pts',(-0.0705344808213482,0.073605857100598,
-0.137275169629765));
#45661=CARTESIAN_POINT('Ctrl Pts',(-0.0918418768227671,0.0442493480543698,
-0.135165949291141));
#45662=CARTESIAN_POINT('Ctrl Pts',(-0.0960028615083386,0.0126360084708544,
-0.133056728952517));
#45663=CARTESIAN_POINT('Ctrl Pts',(-0.0965507213551153,0.00847360925790264,
-0.132779016531334));
#45664=CARTESIAN_POINT('Ctrl Pts',(-0.0968013325140246,0.0042720858280176,
-0.132501304110151));
#45665=CARTESIAN_POINT('Ctrl Pts',(-0.0967681696808917,6.65845257773007E-5,
-0.132223591688967));
#45666=CARTESIAN_POINT('Origin',(0.,0.,-0.493));
#45667=CARTESIAN_POINT('',(-0.0965260258856889,2.69457101370538E-5,-0.0864264083110318));
#45668=CARTESIAN_POINT('',(-0.0965245173086395,2.40562356700919E-5,-0.0922235916889671));
#45669=CARTESIAN_POINT('',(-0.096675,-1.1839272930757E-17,-0.493));
#45670=CARTESIAN_POINT('Ctrl Pts',(-0.0965260258856889,2.69457101370538E-5,
-0.0864264083110318));
#45671=CARTESIAN_POINT('Ctrl Pts',(-0.0965621452892423,0.0144064289818037,
-0.0873699162708424));
#45672=CARTESIAN_POINT('Ctrl Pts',(-0.0935513702939852,0.028771524918513,
-0.0883134242306529));
#45673=CARTESIAN_POINT('Ctrl Pts',(-0.0874164788557378,0.0416481827205965,
-0.0892569321904635));
#45674=CARTESIAN_POINT('Ctrl Pts',(-0.0737018751131272,0.0704340644370663,
-0.0913661525290875));
#45675=CARTESIAN_POINT('Ctrl Pts',(-0.0443745008367193,0.0917814772380087,
-0.0934753728677115));
#45676=CARTESIAN_POINT('Ctrl Pts',(-0.0127668769250902,0.0959855552481512,
-0.0955845932063354));
#45677=CARTESIAN_POINT('Ctrl Pts',(0.0188407469865399,0.100189633258294,
-0.0976938135449594));
#45678=CARTESIAN_POINT('Ctrl Pts',(0.0527286205333904,0.0872503764776352,
-0.0998030338835834));
#45679=CARTESIAN_POINT('Ctrl Pts',(0.0734907857447863,0.0630501695333001,
-0.101912254222207));
#45680=CARTESIAN_POINT('Ctrl Pts',(0.0942529509561815,0.0388499625889657,
-0.104021474560832));
#45681=CARTESIAN_POINT('Ctrl Pts',(0.101889407832122,0.00338880548095356,
-0.106130694899456));
#45682=CARTESIAN_POINT('Ctrl Pts',(0.0929285478197121,-0.027212175791531,
-0.10823991523808));
#45683=CARTESIAN_POINT('Ctrl Pts',(0.0839676878073023,-0.0578131570640146,
-0.110349135576704));
#45684=CARTESIAN_POINT('Ctrl Pts',(0.0584095109065445,-0.0835539625009726,
-0.112458355915327));
#45685=CARTESIAN_POINT('Ctrl Pts',(0.0278731037655201,-0.0927324585046492,
-0.114567576253951));
#45686=CARTESIAN_POINT('Ctrl Pts',(-0.00266330337550607,-0.101910954508326,
-0.116676796592575));
#45687=CARTESIAN_POINT('Ctrl Pts',(-0.0381779407567985,-0.0945271410787201,
-0.118786016931199));
#45688=CARTESIAN_POINT('Ctrl Pts',(-0.0625253511897811,-0.0739378052832015,
-0.120895237269823));
#45689=CARTESIAN_POINT('Ctrl Pts',(-0.0838080480942971,-0.0559401379580672,
-0.122738960950226));
#45690=CARTESIAN_POINT('Ctrl Pts',(-0.0965579146939385,-0.0278521875253081,
-0.124582684630629));
#45691=CARTESIAN_POINT('Ctrl Pts',(-0.0967728733759203,6.44486977623322E-5,
-0.126426408311032));
#45692=CARTESIAN_POINT('Ctrl Pts',(-0.0967681696808917,6.65845257773007E-5,
-0.132223591688967));
#45693=CARTESIAN_POINT('Ctrl Pts',(-0.096549461453191,-0.0276686132699799,
-0.130392083771527));
#45694=CARTESIAN_POINT('Ctrl Pts',(-0.0839883542531326,-0.0555768237062418,
-0.128560575854086));
#45695=CARTESIAN_POINT('Ctrl Pts',(-0.0629499367115576,-0.0735766513583343,
-0.126729067936645));
#45696=CARTESIAN_POINT('Ctrl Pts',(-0.0387214538594795,-0.094305801483208,
-0.124619847598021));
#45697=CARTESIAN_POINT('Ctrl Pts',(-0.00324991478559811,-0.101893931612153,
-0.122510627259397));
#45698=CARTESIAN_POINT('Ctrl Pts',(0.0273388238586198,-0.0928913715547443,
-0.120401406920773));
#45699=CARTESIAN_POINT('Ctrl Pts',(0.0579275625028361,-0.0838888114973365,
-0.118292186582149));
#45700=CARTESIAN_POINT('Ctrl Pts',(0.0836335007173896,-0.058295561253578,
-0.116182966243526));
#45701=CARTESIAN_POINT('Ctrl Pts',(0.0927703633790611,-0.0277466698065643,
-0.114073745904902));
#45702=CARTESIAN_POINT('Ctrl Pts',(0.101907226040733,0.00280222164045035,
-0.111964525566278));
#45703=CARTESIAN_POINT('Ctrl Pts',(0.0944750131495218,0.0383067542907205,
-0.109855305227654));
#45704=CARTESIAN_POINT('Ctrl Pts',(0.0738525078919995,0.0626260754898117,
-0.10774608488903));
#45705=CARTESIAN_POINT('Ctrl Pts',(0.0532300026344766,0.0869453966889036,
-0.105636864550406));
#45706=CARTESIAN_POINT('Ctrl Pts',(0.0194172050106418,0.100079506436816,
-0.103527644211782));
#45707=CARTESIAN_POINT('Ctrl Pts',(-0.0122141083892025,0.0960574515179389,
-0.101418423873158));
#45708=CARTESIAN_POINT('Ctrl Pts',(-0.043845421789046,0.0920353965990621,
-0.0993092035345336));
#45709=CARTESIAN_POINT('Ctrl Pts',(-0.073295250964899,0.0708571770133972,
-0.0971999831959097));
#45710=CARTESIAN_POINT('Ctrl Pts',(-0.0871753089182591,0.0421507139525716,
-0.0950907628572857));
#45711=CARTESIAN_POINT('Ctrl Pts',(-0.0934645999973232,0.0291433257524216,
-0.0941350391345129));
#45712=CARTESIAN_POINT('Ctrl Pts',(-0.0965571823799272,0.014590275702639,
-0.09317931541174));
#45713=CARTESIAN_POINT('Ctrl Pts',(-0.0965245173086395,2.40562356700919E-5,
-0.0922235916889671));
#45714=CARTESIAN_POINT('Origin',(0.,0.,-0.493));
#45715=CARTESIAN_POINT('',(-0.0966799176497682,-8.54770466914428E-5,-0.0464264083110319));
#45716=CARTESIAN_POINT('',(-0.0966824608565994,-8.60709826375376E-5,-0.0522235916889671));
#45717=CARTESIAN_POINT('',(-0.096675,-1.1839272930757E-17,-0.493));
#45718=CARTESIAN_POINT('Ctrl Pts',(-0.0966799176497682,-8.54770466914428E-5,
-0.0464264083110319));
#45719=CARTESIAN_POINT('Ctrl Pts',(-0.0964558808207423,0.0245299519874446,
-0.0480479275724319));
#45720=CARTESIAN_POINT('Ctrl Pts',(-0.0868711565580783,0.0492992357821797,
-0.0496694468338319));
#45721=CARTESIAN_POINT('Ctrl Pts',(-0.0699093451673916,0.066997198228178,
-0.051290966095232));
#45722=CARTESIAN_POINT('Ctrl Pts',(-0.0478459639811275,0.0900181411376509,
-0.0534001864338559));
#45723=CARTESIAN_POINT('Ctrl Pts',(-0.0133005709610127,0.101074427099992,
-0.05550940677248));
#45724=CARTESIAN_POINT('Ctrl Pts',(0.018027220984719,0.0951380919169941,
-0.0576186271111039));
#45725=CARTESIAN_POINT('Ctrl Pts',(0.0493550129304515,0.0892017567339961,
-0.0597278474497278));
#45726=CARTESIAN_POINT('Ctrl Pts',(0.0774652038018009,0.0662728004056583,
-0.0618370677883516));
#45727=CARTESIAN_POINT('Ctrl Pts',(0.0895757663479387,0.0367759010445744,
-0.0639462881269756));
#45728=CARTESIAN_POINT('Ctrl Pts',(0.101686328894077,0.00727900168348961,
-0.0660555084655996));
#45729=CARTESIAN_POINT('Ctrl Pts',(0.0977972631150027,-0.0287858407103417,
-0.0681647288042237));
#45730=CARTESIAN_POINT('Ctrl Pts',(0.0796780386229298,-0.0550234976588298,
-0.0702739491428478));
#45731=CARTESIAN_POINT('Ctrl Pts',(0.0615588141308575,-0.0812611546073171,
-0.0723831694814718));
#45732=CARTESIAN_POINT('Ctrl Pts',(0.0292094309257873,-0.0976716261104618,
-0.0744923898200957));
#45733=CARTESIAN_POINT('Ctrl Pts',(-0.00266439346619636,-0.0967942456364108,
-0.0766016101587197));
#45734=CARTESIAN_POINT('Ctrl Pts',(-0.0345382178581791,-0.0959168651623598,
-0.0787108304973436));
#45735=CARTESIAN_POINT('Ctrl Pts',(-0.0659364834370753,-0.0777516327111142,
-0.0808200508359675));
#45736=CARTESIAN_POINT('Ctrl Pts',(-0.0825846996221178,-0.0505568411694939,
-0.0829292711745914));
#45737=CARTESIAN_POINT('Ctrl Pts',(-0.0917857448314237,-0.0355269722843872,
-0.0840949835534049));
#45738=CARTESIAN_POINT('Ctrl Pts',(-0.0964814000450697,-0.0177390322834002,
-0.0852606959322183));
#45739=CARTESIAN_POINT('Ctrl Pts',(-0.0965260258856889,2.69457101370538E-5,
-0.0864264083110318));
#45740=CARTESIAN_POINT('Ctrl Pts',(-0.0965245173086395,2.40562356700919E-5,
-0.0922235916889671));
#45741=CARTESIAN_POINT('Ctrl Pts',(-0.0964850926838353,-0.0175564269735832,
-0.091070095073116));
#45742=CARTESIAN_POINT('Ctrl Pts',(-0.0918931431861939,-0.0351560939755392,
-0.0899165984572649));
#45743=CARTESIAN_POINT('Ctrl Pts',(-0.0828743072279342,-0.0500806183209312,
-0.0887631018414138));
#45744=CARTESIAN_POINT('Ctrl Pts',(-0.066382960853382,-0.0773707809976222,
-0.0866538815027898));
#45745=CARTESIAN_POINT('Ctrl Pts',(-0.0350899813734107,-0.0957163998150173,
-0.0845446611641659));
#45746=CARTESIAN_POINT('Ctrl Pts',(-0.00322164800733973,-0.0967772732126683,
-0.0824354408255419));
#45747=CARTESIAN_POINT('Ctrl Pts',(0.0286466853587313,-0.0978381466103194,
-0.080326220486918));
#45748=CARTESIAN_POINT('Ctrl Pts',(0.0610903726109036,-0.0816142745882247,
-0.0782170001482938));
#45749=CARTESIAN_POINT('Ctrl Pts',(0.079360166403506,-0.0554813080526386,
-0.0761077798096698));
#45750=CARTESIAN_POINT('Ctrl Pts',(0.0976299601961084,-0.0293483415170525,
-0.0739985594710458));
#45751=CARTESIAN_POINT('Ctrl Pts',(0.101725860529144,0.0066937195320257,
-0.0718893391324219));
#45752=CARTESIAN_POINT('Ctrl Pts',(0.0897856158264645,0.0362597525964753,
-0.0697801187937979));
#45753=CARTESIAN_POINT('Ctrl Pts',(0.0778453711237855,0.0658257856609249,
-0.0676708984551739));
#45754=CARTESIAN_POINT('Ctrl Pts',(0.0498689813853927,0.088915790740745,
-0.0655616781165499));
#45755=CARTESIAN_POINT('Ctrl Pts',(0.0185752788956987,0.0950325400363498,
-0.063452457777926));
#45756=CARTESIAN_POINT('Ctrl Pts',(-0.0127184235939963,0.101149289331955,
-0.0613432374393019));
#45757=CARTESIAN_POINT('Ctrl Pts',(-0.0473294388349918,0.090292782843343,
-0.0592340171006779));
#45758=CARTESIAN_POINT('Ctrl Pts',(-0.069523830713283,0.0673989000216935,
-0.0571247967620539));
#45759=CARTESIAN_POINT('Ctrl Pts',(-0.0867149011254147,0.0496660261609312,
-0.0554910617376916));
#45760=CARTESIAN_POINT('Ctrl Pts',(-0.0964565449248585,0.0247112571856237,
-0.0538573267133294));
#45761=CARTESIAN_POINT('Ctrl Pts',(-0.0966824608565994,-8.60709826375376E-5,
-0.0522235916889671));
#45762=CARTESIAN_POINT('Origin',(0.,0.,-1.05327725593024));
#45763=CARTESIAN_POINT('',(-0.0739037591343974,-6.53400956822213E-5,-0.0332772559302386));
#45764=CARTESIAN_POINT('',(-0.0740000552263865,4.36537410774818E-5,-0.0253727440697612));
#45765=CARTESIAN_POINT('',(-0.0739,6.54188504088864E-16,-1.05327725593024));
#45766=CARTESIAN_POINT('',(0.0740154662741573,-0.000526981588894721,-0.0133250000000002));
#45767=CARTESIAN_POINT('Ctrl Pts',(-0.0739037591343974,-6.53400956822266E-5,
-0.0332772559302386));
#45768=CARTESIAN_POINT('Ctrl Pts',(-0.0739552679160763,-0.00572472549920979,
-0.0327895548530145));
#45769=CARTESIAN_POINT('Ctrl Pts',(-0.0707828206579678,-0.0358032940414331,
-0.0301926334371664));
#45770=CARTESIAN_POINT('Ctrl Pts',(-0.0296542637309572,-0.082043730023256,
-0.0254864916826941));
#45771=CARTESIAN_POINT('Ctrl Pts',(0.0504128653233092,-0.0699260839861745,
-0.0193234407831724));
#45772=CARTESIAN_POINT('Ctrl Pts',(0.0737279762021362,-0.0230151521843795,
-0.0152696102222742));
#45773=CARTESIAN_POINT('Ctrl Pts',(0.0740154662741573,-0.000526981588894725,
-0.0133250000000001));
#45774=CARTESIAN_POINT('',(0.0233628051714152,-0.0701098376443883,-0.013325));
#45775=CARTESIAN_POINT('Origin',(0.,0.,-0.013325));
#45776=CARTESIAN_POINT('Ctrl Pts',(-0.0740000552263865,4.36537410774818E-5,
-0.0253727440697612));
#45777=CARTESIAN_POINT('Ctrl Pts',(-0.073837658281225,-0.022021592300188,
-0.0234660497184648));
#45778=CARTESIAN_POINT('Ctrl Pts',(-0.0516098552235117,-0.0687718438380149,
-0.0194501350285445));
#45779=CARTESIAN_POINT('Ctrl Pts',(0.00013432532901024,-0.0778502984302035,
-0.015434220338624));
#45780=CARTESIAN_POINT('Ctrl Pts',(0.0233628051714152,-0.0701098376443883,
-0.013325));
#45781=CARTESIAN_POINT('Origin',(0.,0.,-1.05327725593024));
#45782=CARTESIAN_POINT('',(-0.0737861216752254,2.05977551544039E-5,-0.0732772559302385));
#45783=CARTESIAN_POINT('',(-0.0739057032045792,-6.57941103356097E-5,-0.0653727440697609));
#45784=CARTESIAN_POINT('',(-0.0739,6.54188504088864E-16,-1.05327725593024));
#45785=CARTESIAN_POINT('Ctrl Pts',(-0.0737861216752254,2.05977551544058E-5,
-0.0732772559302385));
#45786=CARTESIAN_POINT('Ctrl Pts',(-0.0737520089302376,-0.0135600153684295,
-0.072111543551425));
#45787=CARTESIAN_POINT('Ctrl Pts',(-0.0636679022392886,-0.0517603253615703,
-0.0688366108339875));
#45788=CARTESIAN_POINT('Ctrl Pts',(-0.00240023246381204,-0.0872062789102198,
-0.0634524577779261));
#45789=CARTESIAN_POINT('Ctrl Pts',(0.071785009393588,-0.0495729555872598,
-0.057124796762054));
#45790=CARTESIAN_POINT('Ctrl Pts',(0.0807036117542888,0.033132765216591,
-0.050797135746182));
#45791=CARTESIAN_POINT('Ctrl Pts',(0.0162399001827532,0.0857146076576825,
-0.0444694747303104));
#45792=CARTESIAN_POINT('Ctrl Pts',(-0.0568754076960062,0.0623139836826857,
-0.0386295147916622));
#45793=CARTESIAN_POINT('Ctrl Pts',(-0.0737325016048901,0.0187511088892927,
-0.0348987751916385));
#45794=CARTESIAN_POINT('Ctrl Pts',(-0.0739037591343974,-6.53400956822266E-5,
-0.0332772559302386));
#45795=CARTESIAN_POINT('Ctrl Pts',(-0.0739057032045792,-6.57941103356053E-5,
-0.0653727440697609));
#45796=CARTESIAN_POINT('Ctrl Pts',(-0.0739559643758101,-0.00558263724541527,
-0.0648972587554992));
#45797=CARTESIAN_POINT('Ctrl Pts',(-0.070879856117806,-0.0355164036035382,
-0.0623125531026135));
#45798=CARTESIAN_POINT('Ctrl Pts',(-0.0301398485007547,-0.0818676840127184,
-0.0576186271111039));
#45799=CARTESIAN_POINT('Ctrl Pts',(0.0521761247033908,-0.0699113944796167,
-0.0512909660952318));
#45800=CARTESIAN_POINT('Ctrl Pts',(0.0870667295313287,0.00560289368117736,
-0.04496330507936));
#45801=CARTESIAN_POINT('Ctrl Pts',(0.0427661024466595,0.0760368969037317,
-0.0386356440634878));
#45802=CARTESIAN_POINT('Ctrl Pts',(-0.0403659317628278,0.0773093583706435,
-0.032307983047616));
#45803=CARTESIAN_POINT('Ctrl Pts',(-0.0728760131951745,0.0291232266081595,
-0.0278870163830404));
#45804=CARTESIAN_POINT('Ctrl Pts',(-0.074017304767004,0.00238738845508473,
-0.0255752700570888));
#45805=CARTESIAN_POINT('Ctrl Pts',(-0.0740000552263865,4.36537410774818E-5,
-0.0253727440697612));
#45806=CARTESIAN_POINT('Origin',(0.,0.,-1.05327725593024));
#45807=CARTESIAN_POINT('',(-0.0739748160587588,4.92656712164654E-5,-0.113277255930238));
#45808=CARTESIAN_POINT('',(-0.0737849684934933,1.83889921493083E-5,-0.105372744069761));
#45809=CARTESIAN_POINT('',(-0.0739,6.54188504088864E-16,-1.05327725593024));
#45810=CARTESIAN_POINT('Ctrl Pts',(-0.0739748160587588,4.92656712164654E-5,
-0.113277255930238));
#45811=CARTESIAN_POINT('Ctrl Pts',(-0.0738104980179169,-0.0212906817493676,
-0.111433532249835));
#45812=CARTESIAN_POINT('Ctrl Pts',(-0.0529146149777968,-0.0673243027675011,
-0.107480588230809));
#45813=CARTESIAN_POINT('Ctrl Pts',(0.0251121136077328,-0.0835467633888102,
-0.101418423873158));
#45814=CARTESIAN_POINT('Ctrl Pts',(0.0837234176563311,-0.0245166463433077,
-0.0950907628572859));
#45815=CARTESIAN_POINT('Ctrl Pts',(0.0662111084823356,0.0568046728275819,
-0.0887631018414139));
#45816=CARTESIAN_POINT('Ctrl Pts',(-0.0115022772465146,0.0864776309684878,
-0.0824354408255419));
#45817=CARTESIAN_POINT('Ctrl Pts',(-0.0663672499855129,0.0465413853866943,
-0.0772734921884835));
#45818=CARTESIAN_POINT('Ctrl Pts',(-0.0738137319562963,0.0110125172149529,
-0.074220763890049));
#45819=CARTESIAN_POINT('Ctrl Pts',(-0.0737861216752254,2.05977551544058E-5,
-0.0732772559302385));
#45820=CARTESIAN_POINT('Ctrl Pts',(-0.0737849684934933,1.83889921493057E-5,
-0.105372744069761));
#45821=CARTESIAN_POINT('Ctrl Pts',(-0.0737548316455695,-0.0134204287907709,
-0.10421924745391));
#45822=CARTESIAN_POINT('Ctrl Pts',(-0.0638261762896611,-0.0514742070674987,
-0.100956530499435));
#45823=CARTESIAN_POINT('Ctrl Pts',(-0.00290249226713311,-0.0871909301984517,
-0.0955845932063355));
#45824=CARTESIAN_POINT('Ctrl Pts',(0.0714990124011491,-0.0499855262439841,
-0.0892569321904637));
#45825=CARTESIAN_POINT('Ctrl Pts',(0.0808919382230671,0.032667951227759,
-0.0829292711745915));
#45826=CARTESIAN_POINT('Ctrl Pts',(0.0167350661775352,0.0856191188118938,
-0.0766016101587197));
#45827=CARTESIAN_POINT('Ctrl Pts',(-0.0566723609033016,0.0625932640986974,
-0.0707494344571094));
#45828=CARTESIAN_POINT('Ctrl Pts',(-0.0737330092572742,0.0188897016396973,
-0.0670064790941231));
#45829=CARTESIAN_POINT('Ctrl Pts',(-0.0739057032045792,-6.57941103356053E-5,
-0.0653727440697609));
#45830=CARTESIAN_POINT('Origin',(0.,0.,-1.05327725593024));
#45831=CARTESIAN_POINT('',(-0.0739272263990603,-6.35998515147437E-5,-0.153277255930238));
#45832=CARTESIAN_POINT('',(-0.0739712204749718,5.0898334158311E-5,-0.145372744069761));
#45833=CARTESIAN_POINT('',(-0.0739,6.54188504088864E-16,-1.05327725593024));
#45834=CARTESIAN_POINT('Ctrl Pts',(-0.0739272263990603,-6.35998515147395E-5,
-0.153277255930238));
#45835=CARTESIAN_POINT('Ctrl Pts',(-0.0739705678528545,-0.00484618554001679,
-0.15286474128687));
#45836=CARTESIAN_POINT('Ctrl Pts',(-0.0713743141958555,-0.0340356706082163,
-0.150343006304878));
#45837=CARTESIAN_POINT('Ctrl Pts',(-0.0325577426519127,-0.0809362252804344,
-0.145712050984262));
#45838=CARTESIAN_POINT('Ctrl Pts',(0.0500829872689032,-0.0714309007163379,
-0.139384389968389));
#45839=CARTESIAN_POINT('Ctrl Pts',(0.0871868701826791,0.00302138775326442,
-0.133056728952518));
#45840=CARTESIAN_POINT('Ctrl Pts',(0.0450180242988335,0.0747265460260562,
-0.126729067936645));
#45841=CARTESIAN_POINT('Ctrl Pts',(-0.0380824646851997,0.0784882487172661,
-0.120401406920774));
#45842=CARTESIAN_POINT('Ctrl Pts',(-0.0724329427199956,0.0305837973187204,
-0.115917469585305));
#45843=CARTESIAN_POINT('Ctrl Pts',(-0.0739984778965888,0.00312222328791404,
-0.113542752588459));
#45844=CARTESIAN_POINT('Ctrl Pts',(-0.0739748160587588,4.92656712164654E-5,
-0.113277255930238));
#45845=CARTESIAN_POINT('Ctrl Pts',(-0.0739712204749718,5.08983341583136E-5,
-0.145372744069761));
#45846=CARTESIAN_POINT('Ctrl Pts',(-0.0738040362181614,-0.0211503544934227,
-0.14354123615232));
#45847=CARTESIAN_POINT('Ctrl Pts',(-0.0531442479111094,-0.067052177514178,
-0.139600507896256));
#45848=CARTESIAN_POINT('Ctrl Pts',(0.0246307528823777,-0.083689933929838,
-0.133550559301567));
#45849=CARTESIAN_POINT('Ctrl Pts',(0.0835809106498128,-0.0249981979169972,
-0.127222898285695));
#45850=CARTESIAN_POINT('Ctrl Pts',(0.0665369841126368,0.0564225922414199,
-0.120895237269823));
#45851=CARTESIAN_POINT('Ctrl Pts',(-0.0110042337120753,0.0865423970628537,
-0.114567576253952));
#45852=CARTESIAN_POINT('Ctrl Pts',(-0.0662286724539735,0.0468289140681891,
-0.10939341185393));
#45853=CARTESIAN_POINT('Ctrl Pts',(-0.0738099382247387,0.0111530527481255,
-0.106328467792534));
#45854=CARTESIAN_POINT('Ctrl Pts',(-0.0737849684934933,1.83889921493057E-5,
-0.105372744069761));
#45855=CARTESIAN_POINT('Origin',(0.,0.,-1.05327725593024));
#45856=CARTESIAN_POINT('',(-0.0737812135695977,6.75269259391766E-6,-0.193277255930238));
#45857=CARTESIAN_POINT('',(-0.0739314302962117,-6.28702772325351E-5,-0.185372744069761));
#45858=CARTESIAN_POINT('',(-0.0739,6.54188504088864E-16,-1.05327725593024));
#45859=CARTESIAN_POINT('Ctrl Pts',(-0.0737812135695977,6.75269259391761E-6,
-0.193277255930238));
#45860=CARTESIAN_POINT('Ctrl Pts',(-0.0737707790832793,-0.0127000412597446,
-0.192186729985281));
#45861=CARTESIAN_POINT('Ctrl Pts',(-0.0646238781142857,-0.0499975205142205,
-0.188986983701699));
#45862=CARTESIAN_POINT('Ctrl Pts',(-0.00548820489699097,-0.0870664043988389,
-0.183678017079493));
#45863=CARTESIAN_POINT('Ctrl Pts',(0.0699845600316936,-0.0520849356893883,
-0.177350356063621));
#45864=CARTESIAN_POINT('Ctrl Pts',(0.0818254144363875,0.0302536067170679,
-0.17102269504775));
#45865=CARTESIAN_POINT('Ctrl Pts',(0.0192683238503164,0.0850847275592565,
-0.164695034031877));
#45866=CARTESIAN_POINT('Ctrl Pts',(-0.05558770111295,0.064023245622808,
-0.158779887659374));
#45867=CARTESIAN_POINT('Ctrl Pts',(-0.0737489595358703,0.0196075572969276,
-0.154973961625494));
#45868=CARTESIAN_POINT('Ctrl Pts',(-0.0739272263990603,-6.35998515147395E-5,
-0.153277255930238));
#45869=CARTESIAN_POINT('Ctrl Pts',(-0.0739314302962117,-6.2870277232539E-5,
-0.185372744069761));
#45870=CARTESIAN_POINT('Ctrl Pts',(-0.0739732773337877,-0.00470314854841896,
-0.184972445189355));
#45871=CARTESIAN_POINT('Ctrl Pts',(-0.0714673786331718,-0.0337485430234499,
-0.182462925970325));
#45872=CARTESIAN_POINT('Ctrl Pts',(-0.0330231128016351,-0.0807474638242463,
-0.177844186412671));
#45873=CARTESIAN_POINT('Ctrl Pts',(0.0496709636615209,-0.0717180191165734,
-0.171516525396799));
#45874=CARTESIAN_POINT('Ctrl Pts',(0.0872028169333057,0.00251944540519899,
-0.165188864380927));
#45875=CARTESIAN_POINT('Ctrl Pts',(0.0454474412670434,0.0744661599442045,
-0.158861203365055));
#45876=CARTESIAN_POINT('Ctrl Pts',(-0.0376300136353005,0.078706168691497,
-0.152533542349183));
#45877=CARTESIAN_POINT('Ctrl Pts',(-0.0723500183551033,0.030870284260848,
-0.148037389250752));
#45878=CARTESIAN_POINT('Ctrl Pts',(-0.0739965707037644,0.00326565443693249,
-0.145650456490944));
#45879=CARTESIAN_POINT('Ctrl Pts',(-0.0739712204749718,5.08983341583136E-5,
-0.145372744069761));
#45880=CARTESIAN_POINT('Origin',(0.,0.,-1.05327725593024));
#45881=CARTESIAN_POINT('',(-0.0739514724689521,5.80827170926923E-5,-0.233277255930238));
#45882=CARTESIAN_POINT('',(-0.0737808888395284,4.46017856624292E-6,-0.22537274406976));
#45883=CARTESIAN_POINT('',(-0.0739,6.54188504088864E-16,-1.05327725593024));
#45884=CARTESIAN_POINT('Ctrl Pts',(-0.0739514724689521,5.808271709269E-5,
-0.233277255930238));
#45885=CARTESIAN_POINT('Ctrl Pts',(-0.0737747026266549,-0.0204284806437574,
-0.231508718683691));
#45886=CARTESIAN_POINT('Ctrl Pts',(-0.0543062576718298,-0.0656429917484751,
-0.22763096109852));
#45887=CARTESIAN_POINT('Ctrl Pts',(0.0221368387963713,-0.0843838819687206,
-0.221643983174725));
#45888=CARTESIAN_POINT('Ctrl Pts',(0.0828024243326025,-0.0274670291926198,
-0.215316322158853));
#45889=CARTESIAN_POINT('Ctrl Pts',(0.0681817402553036,0.0544236112708011,
-0.208988661142981));
#45890=CARTESIAN_POINT('Ctrl Pts',(-0.00843168039820402,0.0868307890880593,
-0.202661000127109));
#45891=CARTESIAN_POINT('Ctrl Pts',(-0.0654962553541143,0.048310132439586,
-0.197423865056195));
#45892=CARTESIAN_POINT('Ctrl Pts',(-0.0737909607496282,0.0118765663550488,
-0.194295950323905));
#45893=CARTESIAN_POINT('Ctrl Pts',(-0.0737812135695977,6.75269259391761E-6,
-0.193277255930238));
#45894=CARTESIAN_POINT('Ctrl Pts',(-0.0737808888395284,4.46017856623859E-6,
-0.22537274406976));
#45895=CARTESIAN_POINT('Ctrl Pts',(-0.0737740757179536,-0.0125601331883079,
-0.224294433887765));
#45896=CARTESIAN_POINT('Ctrl Pts',(-0.0647750414269508,-0.0497107593494358,
-0.221106903367146));
#45897=CARTESIAN_POINT('Ctrl Pts',(-0.00598931255869429,-0.0870333673276597,
-0.215810152507903));
#45898=CARTESIAN_POINT('Ctrl Pts',(0.0696835717087142,-0.0524869386356467,
-0.209482491492031));
#45899=CARTESIAN_POINT('Ctrl Pts',(0.0819982124259003,0.0297820760219009,
-0.203154830476159));
#45900=CARTESIAN_POINT('Ctrl Pts',(0.0197577953896086,0.0849723979572207,
-0.196827169460287));
#45901=CARTESIAN_POINT('Ctrl Pts',(-0.0553730665477232,0.0642995700232107,
-0.190899807324821));
#45902=CARTESIAN_POINT('Ctrl Pts',(-0.0737527805323053,0.0197470055377898,
-0.187081665527979));
#45903=CARTESIAN_POINT('Ctrl Pts',(-0.0739314302962117,-6.2870277232539E-5,
-0.185372744069761));
#45904=CARTESIAN_POINT('Origin',(0.,0.,-1.05327725593024));
#45905=CARTESIAN_POINT('',(-0.0739525682181994,-5.77538386566367E-5,-0.273277255930238));
#45906=CARTESIAN_POINT('',(-0.0739474476707976,5.92274223705867E-5,-0.265372744069761));
#45907=CARTESIAN_POINT('',(-0.0739,6.54188504088864E-16,-1.05327725593024));
#45908=CARTESIAN_POINT('Ctrl Pts',(-0.0739525682181994,-5.77538386566322E-5,
-0.273277255930238));
#45909=CARTESIAN_POINT('Ctrl Pts',(-0.0739861634225736,-0.0039651806039843,
-0.272939927720726));
#45910=CARTESIAN_POINT('Ctrl Pts',(-0.0719323350430627,-0.0322692975822643,
-0.270493379172589));
#45911=CARTESIAN_POINT('Ctrl Pts',(-0.0354043422207423,-0.0797321247674219,
-0.265937610285828));
#45912=CARTESIAN_POINT('Ctrl Pts',(0.0475212323275497,-0.0731601780074524,
-0.259609949269957));
#45913=CARTESIAN_POINT('Ctrl Pts',(0.0872391793431545,-6.89604553678452E-5,
-0.253282288254085));
#45914=CARTESIAN_POINT('Ctrl Pts',(0.0476368355604161,0.0730849578627569,
-0.246954627238213));
#45915=CARTESIAN_POINT('Ctrl Pts',(-0.035278245432985,0.0797879976386212,
-0.240626966222341));
#45916=CARTESIAN_POINT('Ctrl Pts',(-0.0719081835391686,0.0323480695112505,
-0.236067842453016));
#45917=CARTESIAN_POINT('Ctrl Pts',(-0.0739855246194383,0.00400452250253258,
-0.233617939022315));
#45918=CARTESIAN_POINT('Ctrl Pts',(-0.0739514724689521,5.808271709269E-5,
-0.233277255930238));
#45919=CARTESIAN_POINT('Ctrl Pts',(-0.0739474476707976,5.92274223705815E-5,
-0.265372744069761));
#45920=CARTESIAN_POINT('Ctrl Pts',(-0.0737697580626393,-0.0202887024690249,
-0.263616422586176));
#45921=CARTESIAN_POINT('Ctrl Pts',(-0.0545274805569218,-0.0653684243106095,
-0.259750880763967));
#45922=CARTESIAN_POINT('Ctrl Pts',(0.0216507148888523,-0.0845099132536343,
-0.253776118603134));
#45923=CARTESIAN_POINT('Ctrl Pts',(0.0826429366480972,-0.0279432266482656,
-0.247448457587263));
#45924=CARTESIAN_POINT('Ctrl Pts',(0.0684938994372912,0.0540302196294675,
-0.241120796571391));
#45925=CARTESIAN_POINT('Ctrl Pts',(-0.00793169816963801,0.0868778858943854,
-0.234793135555519));
#45926=CARTESIAN_POINT('Ctrl Pts',(-0.065350690899438,0.0485972782324374,
-0.229543784721642));
#45927=CARTESIAN_POINT('Ctrl Pts',(-0.073787402472013,0.0120167430375237,
-0.226403654226389));
#45928=CARTESIAN_POINT('Ctrl Pts',(-0.0737808888395284,4.46017856623859E-6,
-0.22537274406976));
#45929=CARTESIAN_POINT('Origin',(0.,0.,-1.05327725593024));
#45930=CARTESIAN_POINT('',(-0.0737813255293768,-7.38103354979496E-6,-0.313277255930238));
#45931=CARTESIAN_POINT('',(-0.0739565202301569,-5.65040446714252E-5,-0.305372744069761));
#45932=CARTESIAN_POINT('',(-0.0739,6.54188504088864E-16,-1.05327725593024));
#45933=CARTESIAN_POINT('Ctrl Pts',(-0.0737813255293768,-7.38103354979737E-6,
-0.313277255930238));
#45934=CARTESIAN_POINT('Ctrl Pts',(-0.0737919455150245,-0.011838058808532,
-0.312261916419136));
#45935=CARTESIAN_POINT('Ctrl Pts',(-0.0655360332068969,-0.0482312596297118,
-0.30913735656941));
#45936=CARTESIAN_POINT('Ctrl Pts',(-0.00856894504114455,-0.0868173505060656,
-0.303903576381061));
#45937=CARTESIAN_POINT('Ctrl Pts',(0.0680956140128458,-0.0545313352140282,
-0.297575915365189));
#45938=CARTESIAN_POINT('Ctrl Pts',(0.0828457448677347,0.0273360883324843,
-0.291248254349316));
#45939=CARTESIAN_POINT('Ctrl Pts',(0.0222702178726658,0.0843487792674867,
-0.284920593333445));
#45940=CARTESIAN_POINT('Ctrl Pts',(-0.0542452639373956,0.0657183312475859,
-0.278930260527085));
#45941=CARTESIAN_POINT('Ctrl Pts',(-0.0737761018672454,0.0204668822140799,
-0.27504914805935));
#45942=CARTESIAN_POINT('Ctrl Pts',(-0.0739525682181994,-5.77538386566322E-5,
-0.273277255930238));
#45943=CARTESIAN_POINT('Ctrl Pts',(-0.0739565202301568,-5.6504044671423E-5,
-0.305372744069761));
#45944=CARTESIAN_POINT('Ctrl Pts',(-0.0739884412181998,-0.00382190668348843,
-0.305047631623211));
#45945=CARTESIAN_POINT('Ctrl Pts',(-0.0720196891488213,-0.0319825108223484,
-0.302613298838036));
#45946=CARTESIAN_POINT('Ctrl Pts',(-0.0358627338085138,-0.0795269967816936,
-0.298069745714238));
#45947=CARTESIAN_POINT('Ctrl Pts',(0.0470992967446723,-0.0734325209937202,
-0.291742084698366));
#45948=CARTESIAN_POINT('Ctrl Pts',(0.0872373353447779,-0.000571152587860333,
-0.285414423682494));
#45949=CARTESIAN_POINT('Ctrl Pts',(0.0480567597612106,0.0728095236530848,
-0.279086762666623));
#45950=CARTESIAN_POINT('Ctrl Pts',(-0.0348183598080465,0.0799897538039288,
-0.27275910165075));
#45951=CARTESIAN_POINT('Ctrl Pts',(-0.0718196555148094,0.032634929251857,
-0.268187762118463));
#45952=CARTESIAN_POINT('Ctrl Pts',(-0.0739831509630807,0.00414775063876829,
-0.2657256429248));
#45953=CARTESIAN_POINT('Ctrl Pts',(-0.0739474476707976,5.92274223705815E-5,
-0.265372744069761));
#45954=CARTESIAN_POINT('Origin',(0.,0.,-1.05327725593024));
#45955=CARTESIAN_POINT('',(-0.0739260676437687,6.37850448278505E-5,-0.353277255930238));
#45956=CARTESIAN_POINT('',(-0.0737818159558278,-9.66304559187059E-6,-0.345372744069761));
#45957=CARTESIAN_POINT('',(-0.0739,6.54188504088864E-16,-1.05327725593024));
#45958=CARTESIAN_POINT('Ctrl Pts',(-0.0739260676437687,6.37850448278517E-5,
-0.353277255930238));
#45959=CARTESIAN_POINT('Ctrl Pts',(-0.0737479485415012,-0.0195692698142952,
-0.351583905117547));
#45960=CARTESIAN_POINT('Ctrl Pts',(-0.0556464121921038,-0.0639472967095582,
-0.347781333966231));
#45961=CARTESIAN_POINT('Ctrl Pts',(0.019133785015476,-0.0851150834987123,
-0.341869542476292));
#45962=CARTESIAN_POINT('Ctrl Pts',(0.0817774827305826,-0.030382930837239,
-0.33554188146042));
#45963=CARTESIAN_POINT('Ctrl Pts',(0.0700668162737063,0.0519742284721753,
-0.329214220444548));
#45964=CARTESIAN_POINT('Ctrl Pts',(-0.00535055036065351,0.0870749721725439,
-0.322886559428676));
#45965=CARTESIAN_POINT('Ctrl Pts',(-0.0645821602000743,0.0500762594422092,
-0.317574237923906));
#45966=CARTESIAN_POINT('Ctrl Pts',(-0.0737698840375787,0.012738455657667,
-0.31437113675776));
#45967=CARTESIAN_POINT('Ctrl Pts',(-0.0737813255293768,-7.38103354979737E-6,
-0.313277255930238));
#45968=CARTESIAN_POINT('Ctrl Pts',(-0.0737818159558278,-9.6630455918784E-6,
-0.345372744069761));
#45969=CARTESIAN_POINT('Ctrl Pts',(-0.0737955572724641,-0.0116978086519519,
-0.344369620321621));
#45970=CARTESIAN_POINT('Ctrl Pts',(-0.0656801480854143,-0.0479440254684255,
-0.341257276234857));
#45971=CARTESIAN_POINT('Ctrl Pts',(-0.00906856792307098,-0.086766583251621,
-0.33603571180947));
#45972=CARTESIAN_POINT('Ctrl Pts',(0.0677805742992985,-0.0549224238448479,
-0.329708050793598));
#45973=CARTESIAN_POINT('Ctrl Pts',(0.0830017312015545,0.0268587324883495,
-0.323380389777726));
#45974=CARTESIAN_POINT('Ctrl Pts',(0.0227554031361251,0.0842191814342093,
-0.317052728761854));
#45975=CARTESIAN_POINT('Ctrl Pts',(-0.0540223059082473,0.0659924114034696,
-0.311050180192533));
#45976=CARTESIAN_POINT('Ctrl Pts',(-0.0737813485709526,0.0206067607304377,
-0.307156851961835));
#45977=CARTESIAN_POINT('Ctrl Pts',(-0.0739565202301568,-5.6504044671423E-5,
-0.305372744069761));
#45978=CARTESIAN_POINT('Origin',(0.,0.,-1.05327725593024));
#45979=CARTESIAN_POINT('',(-0.0739757877607653,-4.88044159986755E-5,-0.393277255930238));
#45980=CARTESIAN_POINT('',(-0.0739218355690636,6.44039839332328E-5,-0.385372744069761));
#45981=CARTESIAN_POINT('',(-0.0739,6.54188504088864E-16,-1.05327725593024));
#45982=CARTESIAN_POINT('Ctrl Pts',(-0.0739757877607652,-4.88044159986777E-5,
-0.393277255930238));
#45983=CARTESIAN_POINT('Ctrl Pts',(-0.0739989879633844,-0.00308282705743824,
-0.393015114154581));
#45984=CARTESIAN_POINT('Ctrl Pts',(-0.0724555604706598,-0.0305051292578985,
-0.390643752040301));
#45985=CARTESIAN_POINT('Ctrl Pts',(-0.0382065020487046,-0.0784279438032996,
-0.386163169587396));
#45986=CARTESIAN_POINT('Ctrl Pts',(0.0448998284991146,-0.0747976240850022,
-0.379835508571524));
#45987=CARTESIAN_POINT('Ctrl Pts',(0.0871819848609725,-0.00315922201061306,
-0.373507847555652));
#45988=CARTESIAN_POINT('Ctrl Pts',(0.0501958532401191,0.0713516326758373,
-0.36718018653978));
#45989=CARTESIAN_POINT('Ctrl Pts',(-0.0324297457147349,0.0809875963397409,
-0.360852525523908));
#45990=CARTESIAN_POINT('Ctrl Pts',(-0.0713485905353685,0.0341145348533431,
-0.356218215320728));
#45991=CARTESIAN_POINT('Ctrl Pts',(-0.0739698118614845,0.00488546118876761,
-0.353693125456171));
#45992=CARTESIAN_POINT('Ctrl Pts',(-0.0739260676437687,6.37850448278517E-5,
-0.353277255930238));
#45993=CARTESIAN_POINT('Ctrl Pts',(-0.0739218355690636,6.44039839332311E-5,
-0.385372744069761));
#45994=CARTESIAN_POINT('Ctrl Pts',(-0.0737444054695453,-0.019429892336047,
-0.383691609020032));
#45995=CARTESIAN_POINT('Ctrl Pts',(-0.0558593356375793,-0.0636705354435064,
-0.379901253631678));
#45996=CARTESIAN_POINT('Ctrl Pts',(0.0186435017497599,-0.0852238155437934,
-0.374001677904702));
#45997=CARTESIAN_POINT('Ctrl Pts',(0.0816012266274847,-0.0308531798397786,
-0.367674016888829));
#45998=CARTESIAN_POINT('Ctrl Pts',(0.0703648442895387,0.0515700259981008,
-0.361346355872959));
#45999=CARTESIAN_POINT('Ctrl Pts',(-0.0048492135956714,0.0871043283702904,
-0.355018694857085));
#46000=CARTESIAN_POINT('Ctrl Pts',(-0.0644295159300822,0.0503629031102395,
-0.349694157589354));
#46001=CARTESIAN_POINT('Ctrl Pts',(-0.0737666640630444,0.0128782962199111,
-0.346478840660245));
#46002=CARTESIAN_POINT('Ctrl Pts',(-0.0737818159558278,-9.6630455918784E-6,
-0.345372744069761));
#46003=CARTESIAN_POINT('Origin',(0.,0.,-1.05327725593024));
#46004=CARTESIAN_POINT('',(-0.0737864256067439,-2.11896062283324E-5,-0.433277255930238));
#46005=CARTESIAN_POINT('',(-0.0739792630123745,-4.70781898877851E-5,-0.425372744069761));
#46006=CARTESIAN_POINT('',(-0.0739,6.54188504088864E-16,-1.05327725593024));
#46007=CARTESIAN_POINT('Ctrl Pts',(-0.0737864256067439,-2.11896062283414E-5,
-0.433277255930238));
#46008=CARTESIAN_POINT('Ctrl Pts',(-0.0738147678314805,-0.0109739073698394,
-0.432337102852992));
#46009=CARTESIAN_POINT('Ctrl Pts',(-0.0664051981588223,-0.0464624370744622,
-0.429287729437122));
#46010=CARTESIAN_POINT('Ctrl Pts',(-0.0116389293761198,-0.0864593227534712,
-0.424129135682628));
#46011=CARTESIAN_POINT('Ctrl Pts',(0.0661211938172418,-0.0569092865549545,
-0.417801474666756));
#46012=CARTESIAN_POINT('Ctrl Pts',(0.0837620866257479,0.0243842574648459,
-0.411473813650883));
#46013=CARTESIAN_POINT('Ctrl Pts',(0.0252441581448469,0.0835069556837582,
-0.405146152635012));
#46014=CARTESIAN_POINT('Ctrl Pts',(-0.0528513042080767,0.0673989656330345,
-0.399080633394796));
#46015=CARTESIAN_POINT('Ctrl Pts',(-0.0738123166894069,0.0213292386926207,
-0.395124334493205));
#46016=CARTESIAN_POINT('Ctrl Pts',(-0.0739757877607652,-4.88044159986777E-5,
-0.393277255930238));
#46017=CARTESIAN_POINT('Ctrl Pts',(-0.0739792630123745,-4.70781898877872E-5,
-0.425372744069761));
#46018=CARTESIAN_POINT('Ctrl Pts',(-0.0740007916035247,-0.00293935953098124,
-0.425122818057066));
#46019=CARTESIAN_POINT('Ctrl Pts',(-0.0725373395423451,-0.0302187231335646,
-0.422763671705748));
#46020=CARTESIAN_POINT('Ctrl Pts',(-0.0386573396255769,-0.078206706786622,
-0.418295305015806));
#46021=CARTESIAN_POINT('Ctrl Pts',(0.0444685104211786,-0.0750548497717326,
-0.411967643999933));
#46022=CARTESIAN_POINT('Ctrl Pts',(0.0871623526873201,-0.00366103364462123,
-0.405639982984062));
#46023=CARTESIAN_POINT('Ctrl Pts',(0.0506057570896398,0.0710614962037825,
-0.399312321968189));
#46024=CARTESIAN_POINT('Ctrl Pts',(-0.0319630018346919,0.081172935188099,
-0.392984660952318));
#46025=CARTESIAN_POINT('Ctrl Pts',(-0.0712543236721827,0.03440172595574,
-0.388338134986175));
#46026=CARTESIAN_POINT('Ctrl Pts',(-0.0739670164814616,0.00502844388857318,
-0.385800829358656));
#46027=CARTESIAN_POINT('Ctrl Pts',(-0.0739218355690636,6.44039839332311E-5,
-0.385372744069761));
#46028=CARTESIAN_POINT('Origin',(0.,0.,-1.05327725593024));
#46029=CARTESIAN_POINT('',(-0.0738999238216348,6.62105036960088E-5,-0.473277255930238));
#46030=CARTESIAN_POINT('',(-0.0737877145894119,-2.33604236806045E-5,-0.465372744069761));
#46031=CARTESIAN_POINT('',(-0.0739,6.54188504088864E-16,-1.05327725593024));
#46032=CARTESIAN_POINT('Ctrl Pts',(-0.0738999238216348,6.6210503696003E-5,
-0.473277255930238));
#46033=CARTESIAN_POINT('Ctrl Pts',(-0.0737295153222194,-0.0187121711198471,
-0.471659091551403));
#46034=CARTESIAN_POINT('Ctrl Pts',(-0.0569357917229669,-0.0622387138293177,
-0.467931706833943));
#46035=CARTESIAN_POINT('Ctrl Pts',(0.0161067143487094,-0.0857394478691125,
-0.46209510177786));
#46036=CARTESIAN_POINT('Ctrl Pts',(0.0806498933532556,-0.0332606955748025,
-0.455767440761988));
#46037=CARTESIAN_POINT('Ctrl Pts',(0.0718639438423683,0.049459607190435,
-0.449439779746115));
#46038=CARTESIAN_POINT('Ctrl Pts',(-0.00226270426759789,0.0872098580288294,
-0.443112118730244));
#46039=CARTESIAN_POINT('Ctrl Pts',(-0.0636240999221545,0.0518389223721709,
-0.437724610791618));
#46040=CARTESIAN_POINT('Ctrl Pts',(-0.0737511824449055,0.0135983624331623,
-0.434446323191616));
#46041=CARTESIAN_POINT('Ctrl Pts',(-0.0737864256067439,-2.11896062283414E-5,
-0.433277255930238));
#46042=CARTESIAN_POINT('Ctrl Pts',(-0.0737877145894119,-2.33604236806097E-5,
-0.465372744069761));
#46043=CARTESIAN_POINT('Ctrl Pts',(-0.0738185855908912,-0.0108332925492125,
-0.464444806755477));
#46044=CARTESIAN_POINT('Ctrl Pts',(-0.0665424168125231,-0.046174863428295,
-0.461407649102569));
#46045=CARTESIAN_POINT('Ctrl Pts',(-0.0121364403459336,-0.0863908890396749,
-0.456261271111038));
#46046=CARTESIAN_POINT('Ctrl Pts',(0.0657924981506585,-0.0572889699718141,
-0.449933610095165));
#46047=CARTESIAN_POINT('Ctrl Pts',(0.0839010655140964,0.0239016756511994,
-0.443605949079294));
#46048=CARTESIAN_POINT('Ctrl Pts',(0.0257244481133483,0.0833602522944807,
-0.437278288063421));
#46049=CARTESIAN_POINT('Ctrl Pts',(-0.0526199106140298,0.0676705517485118,
-0.431200553060244));
#46050=CARTESIAN_POINT('Ctrl Pts',(-0.0738191036638569,0.0214696988294836,
-0.42723203839569));
#46051=CARTESIAN_POINT('Ctrl Pts',(-0.0739792630123745,-4.70781898877872E-5,
-0.425372744069761));
#46052=CARTESIAN_POINT('Origin',(0.,0.,-1.05327725593024));
#46053=CARTESIAN_POINT('',(-0.0739954635921359,-3.70971844019372E-5,-0.513277255930238));
#46054=CARTESIAN_POINT('',(-0.0738956892271228,6.62928153061619E-5,-0.505372744069761));
#46055=CARTESIAN_POINT('',(-0.0739,6.54188504088864E-16,-1.05327725593024));
#46056=CARTESIAN_POINT('Ctrl Pts',(-0.0739954635921359,-3.70971844019397E-5,
-0.513277255930238));
#46057=CARTESIAN_POINT('Ctrl Pts',(-0.0740088040956365,-0.00219940070345826,
-0.513090300588437));
#46058=CARTESIAN_POINT('Ctrl Pts',(-0.0729448118129387,-0.0287433874190867,
-0.510794124908012));
#46059=CARTESIAN_POINT('Ctrl Pts',(-0.0409607047580388,-0.077025319432872,
-0.506388728888963));
#46060=CARTESIAN_POINT('Ctrl Pts',(0.0422220660331108,-0.0763411835637019,
-0.500061067873091));
#46061=CARTESIAN_POINT('Ctrl Pts',(0.0870153588274602,-0.00624551808415768,
-0.49373340685722));
#46062=CARTESIAN_POINT('Ctrl Pts',(0.0526918646680198,0.0695287463271004,
-0.487405745841347));
#46063=CARTESIAN_POINT('Ctrl Pts',(-0.0295405399103716,0.082085538737435,
-0.481078084825476));
#46064=CARTESIAN_POINT('Ctrl Pts',(-0.0707533164497064,0.0358829129709433,
-0.476368588188439));
#46065=CARTESIAN_POINT('Ctrl Pts',(-0.0739516368060083,0.00576478867784635,
-0.473768311890027));
#46066=CARTESIAN_POINT('Ctrl Pts',(-0.0738999238216348,6.6210503696003E-5,
-0.473277255930238));
#46067=CARTESIAN_POINT('Ctrl Pts',(-0.0738956892271229,6.62928153061619E-5,
-0.505372744069761));
#46068=CARTESIAN_POINT('Ctrl Pts',(-0.073727254762863,-0.0185730596526899,
-0.503766795453888));
#46069=CARTESIAN_POINT('Ctrl Pts',(-0.0571405360190808,-0.0619599952174389,
-0.50005162649939));
#46070=CARTESIAN_POINT('Ctrl Pts',(0.015612887132456,-0.0858307441930048,
-0.494227237206269));
#46071=CARTESIAN_POINT('Ctrl Pts',(0.0804570900696259,-0.0337244058637655,
-0.487899576190397));
#46072=CARTESIAN_POINT('Ctrl Pts',(0.0721474666049248,0.0490451012418884,
-0.481571915174525));
#46073=CARTESIAN_POINT('Ctrl Pts',(-0.00176064224849756,0.087221436769917,
-0.475244254158653));
#46074=CARTESIAN_POINT('Ctrl Pts',(-0.0634642249304729,0.052124916693094,
-0.469844530457065));
#46075=CARTESIAN_POINT('Ctrl Pts',(-0.0737484151783087,0.0137379024521563,
-0.466554027094101));
#46076=CARTESIAN_POINT('Ctrl Pts',(-0.0737877145894119,-2.33604236806097E-5,
-0.465372744069761));
#46077=CARTESIAN_POINT('Origin',(0.,0.,-1.05327725593024));
#46078=CARTESIAN_POINT('',(-0.0737963410028765,-3.40609569993907E-5,-0.553277255930238));
#46079=CARTESIAN_POINT('',(-0.073998223225288,-3.49682871188597E-5,-0.545372744069761));
#46080=CARTESIAN_POINT('',(-0.0739,6.54188504088864E-16,-1.05327725593024));
#46081=CARTESIAN_POINT('Ctrl Pts',(-0.0737963410028765,-3.40609569993884E-5,
-0.553277255930238));
#46082=CARTESIAN_POINT('Ctrl Pts',(-0.0738385873799593,-0.0101074743734211,
-0.552412289286847));
#46083=CARTESIAN_POINT('Ctrl Pts',(-0.0672323111377545,-0.0446918455824485,
-0.549438102304832));
#46084=CARTESIAN_POINT('Ctrl Pts',(-0.0146943044302958,-0.0859927705410227,
-0.544354694984196));
#46085=CARTESIAN_POINT('Ctrl Pts',(0.0640637777501068,-0.0592158048868383,
-0.538027033968322));
#46086=CARTESIAN_POINT('Ctrl Pts',(0.0845732895170916,0.0214018192747577,
-0.531699372952452));
#46087=CARTESIAN_POINT('Ctrl Pts',(0.0281864117401041,0.0825603134758373,
-0.525371711936578));
#46088=CARTESIAN_POINT('Ctrl Pts',(-0.0514051510485292,0.0690635833670669,
-0.519231006262509));
#46089=CARTESIAN_POINT('Ctrl Pts',(-0.0738582972364053,0.0221955939339471,
-0.515199520927061));
#46090=CARTESIAN_POINT('Ctrl Pts',(-0.0739954635921359,-3.70971844019397E-5,
-0.513277255930238));
#46091=CARTESIAN_POINT('Ctrl Pts',(-0.073998223225288,-3.49682871188433E-5,
-0.545372744069761));
#46092=CARTESIAN_POINT('Ctrl Pts',(-0.0740101004843667,-0.00205578627884039,
-0.545198004490922));
#46093=CARTESIAN_POINT('Ctrl Pts',(-0.0730211466423457,-0.0284573927901487,
-0.542914044573459));
#46094=CARTESIAN_POINT('Ctrl Pts',(-0.0414034224289421,-0.076788251083785,
-0.538520864317373));
#46095=CARTESIAN_POINT('Ctrl Pts',(0.0417819068541502,-0.0765829690790775,
-0.532193203301501));
#46096=CARTESIAN_POINT('Ctrl Pts',(0.0869779631209978,-0.00674631934155149,
-0.525865542285629));
#46097=CARTESIAN_POINT('Ctrl Pts',(0.0530912336515535,0.0692242717743709,
-0.519537881269757));
#46098=CARTESIAN_POINT('Ctrl Pts',(-0.0290675236360216,0.0822542276299836,
-0.513210220253885));
#46099=CARTESIAN_POINT('Ctrl Pts',(-0.070653170669016,0.0361703843477604,
-0.508488507853886));
#46100=CARTESIAN_POINT('Ctrl Pts',(-0.0739484731718648,0.00590748781669472,
-0.505876015792512));
#46101=CARTESIAN_POINT('Ctrl Pts',(-0.0738956892271229,6.62928153061619E-5,
-0.505372744069761));
#46102=CARTESIAN_POINT('Origin',(0.,0.,-1.05327725593024));
#46103=CARTESIAN_POINT('',(-0.0738742530246062,6.53564756795162E-5,-0.593277255930239));
#46104=CARTESIAN_POINT('',(-0.073798384598233,-3.60235004422046E-5,-0.585372744069761));
#46105=CARTESIAN_POINT('',(-0.0739,6.54188504088864E-16,-1.05327725593024));
#46106=CARTESIAN_POINT('Ctrl Pts',(-0.0738742530246063,6.53564756795157E-5,
-0.593277255930239));
#46107=CARTESIAN_POINT('Ctrl Pts',(-0.0737186635600633,-0.0178563908955508,
-0.591734277985259));
#46108=CARTESIAN_POINT('Ctrl Pts',(-0.0581751526568177,-0.0605186698232157,
-0.588082079701655));
#46109=CARTESIAN_POINT('Ctrl Pts',(0.013059426400348,-0.0862561913725913,
-0.582320661079426));
#46110=CARTESIAN_POINT('Ctrl Pts',(0.0794210715600979,-0.0360967112110921,
-0.575993000063554));
#46111=CARTESIAN_POINT('Ctrl Pts',(0.0735708671919806,0.046882903799052,
-0.569665339047683));
#46112=CARTESIAN_POINT('Ctrl Pts',(0.000827981990642192,0.087235277347151,
-0.56333767803181));
#46113=CARTESIAN_POINT('Ctrl Pts',(-0.0626211499353113,0.0535971856145833,
-0.55787498365933));
#46114=CARTESIAN_POINT('Ctrl Pts',(-0.0737355696295557,0.0144565346778415,
-0.554521509625472));
#46115=CARTESIAN_POINT('Ctrl Pts',(-0.0737963410028765,-3.40609569993884E-5,
-0.553277255930238));
#46116=CARTESIAN_POINT('Ctrl Pts',(-0.073798384598233,-3.60235004422177E-5,
-0.585372744069761));
#46117=CARTESIAN_POINT('Ctrl Pts',(-0.0738425071873687,-0.00996648243522716,
-0.584519993189332));
#46118=CARTESIAN_POINT('Ctrl Pts',(-0.0673627861806156,-0.0444040547321228,
-0.58155802197028));
#46119=CARTESIAN_POINT('Ctrl Pts',(-0.0151890790080958,-0.0859067562664407,
-0.576486830412606));
#46120=CARTESIAN_POINT('Ctrl Pts',(0.0637218387120179,-0.0595836065079599,
-0.570159169396731));
#46121=CARTESIAN_POINT('Ctrl Pts',(0.0846950865125139,0.0209146172322998,
-0.563831508380862));
#46122=CARTESIAN_POINT('Ctrl Pts',(0.0286612035496907,0.0823966886738722,
-0.557503847364987));
#46123=CARTESIAN_POINT('Ctrl Pts',(-0.0511652173028116,0.0693324148388138,
-0.551350925927956));
#46124=CARTESIAN_POINT('Ctrl Pts',(-0.0738667342442603,0.0223368008907248,
-0.547307224829546));
#46125=CARTESIAN_POINT('Ctrl Pts',(-0.073998223225288,-3.49682871188433E-5,
-0.545372744069761));
#46126=CARTESIAN_POINT('Origin',(0.,0.,-1.05327725593024));
#46127=CARTESIAN_POINT('',(-0.0740100950880502,-2.31680927942999E-5,-0.633277255930238));
#46128=CARTESIAN_POINT('',(-0.0738702015529844,6.49156969421381E-5,-0.625372744069761));
#46129=CARTESIAN_POINT('',(-0.0739,6.54188504088864E-16,-1.05327725593024));
#46130=CARTESIAN_POINT('Ctrl Pts',(-0.0740100950880502,-2.31680927943018E-5,
-0.633277255930238));
#46131=CARTESIAN_POINT('Ctrl Pts',(-0.0740154327349471,-0.00131519596391571,
-0.633165487022293));
#46132=CARTESIAN_POINT('Ctrl Pts',(-0.0734008815262698,-0.0269842396990781,
-0.630944497775723));
#46133=CARTESIAN_POINT('Ctrl Pts',(-0.0436634932506345,-0.0755260122418957,
-0.62661428819053));
#46134=CARTESIAN_POINT('Ctrl Pts',(0.0394913060792223,-0.0777889189548767,
-0.620286627174658));
#46135=CARTESIAN_POINT('Ctrl Pts',(0.0867395103929965,-0.00932397473154213,
-0.613958966158786));
#46136=CARTESIAN_POINT('Ctrl Pts',(0.0551217368298506,0.0676185869186267,
-0.607631305142914));
#46137=CARTESIAN_POINT('Ctrl Pts',(-0.0266142545750163,0.0830804466852906,
-0.601303644127043));
#46138=CARTESIAN_POINT('Ctrl Pts',(-0.0701214900469694,0.0376528645843343,
-0.59651896105615));
#46139=CARTESIAN_POINT('Ctrl Pts',(-0.0739313512813346,0.00664228336098339,
-0.593843498323883));
#46140=CARTESIAN_POINT('Ctrl Pts',(-0.0738742530246063,6.53564756795157E-5,
-0.593277255930239));
#46141=CARTESIAN_POINT('Ctrl Pts',(-0.0738702015529844,6.49156969421468E-5,
-0.625372744069761));
#46142=CARTESIAN_POINT('Ctrl Pts',(-0.0737175639680371,-0.0177174244228303,
-0.623841981887743));
#46143=CARTESIAN_POINT('Ctrl Pts',(-0.0583718441882899,-0.0602382191459097,
-0.620201999367102));
#46144=CARTESIAN_POINT('Ctrl Pts',(0.012562675089579,-0.0863299373793905,
-0.614452796507836));
#46145=CARTESIAN_POINT('Ctrl Pts',(0.0792119631042182,-0.0365533007334742,
-0.608125135491964));
#46146=CARTESIAN_POINT('Ctrl Pts',(0.0738395288211365,0.0464586146673402,
-0.601797474476092));
#46147=CARTESIAN_POINT('Ctrl Pts',(0.00133013907144687,0.0872290640978479,
-0.59546981346022));
#46148=CARTESIAN_POINT('Ctrl Pts',(-0.062453895076773,0.053882371915127,
-0.589994903324777));
#46149=CARTESIAN_POINT('Ctrl Pts',(-0.0737333730140319,0.0145958210907477,
-0.586629213527957));
#46150=CARTESIAN_POINT('Ctrl Pts',(-0.073798384598233,-3.60235004422177E-5,
-0.585372744069761));
#46151=CARTESIAN_POINT('Origin',(0.,0.,-1.05327725593024));
#46152=CARTESIAN_POINT('',(-0.0738107316200561,-4.54136549985855E-5,-0.673277255930238));
#46153=CARTESIAN_POINT('',(-0.0740118889580303,-2.07425011237994E-5,-0.665372744069761));
#46154=CARTESIAN_POINT('',(-0.0739,6.54188504088864E-16,-1.05327725593024));
#46155=CARTESIAN_POINT('Ctrl Pts',(-0.0738107316200561,-4.54136549985842E-5,
-0.673277255930238));
#46156=CARTESIAN_POINT('Ctrl Pts',(-0.073862779055793,-0.00923870797648464,
-0.672487475720703));
#46157=CARTESIAN_POINT('Ctrl Pts',(-0.0680183112542861,-0.0429202091247773,
-0.669588475172544));
#46158=CARTESIAN_POINT('Ctrl Pts',(-0.0177312350715336,-0.0854182794889314,
-0.664580254285763));
#46159=CARTESIAN_POINT('Ctrl Pts',(0.0619259482971724,-0.0614479950487169,
-0.65825259326989));
#46160=CARTESIAN_POINT('Ctrl Pts',(0.0852783353131607,0.0183925173434011,
-0.651924932254018));
#46161=CARTESIAN_POINT('Ctrl Pts',(0.0310932855172931,0.0815100408768839,
-0.645597271238146));
#46162=CARTESIAN_POINT('Ctrl Pts',(-0.049906181360674,0.0707105530622803,
-0.63938137913022));
#46163=CARTESIAN_POINT('Ctrl Pts',(-0.0739147046022107,0.0230670004262463,
-0.635274707360917));
#46164=CARTESIAN_POINT('Ctrl Pts',(-0.0740100950880502,-2.31680927943018E-5,
-0.633277255930238));
#46165=CARTESIAN_POINT('Ctrl Pts',(-0.0740118889580303,-2.07425011238048E-5,
-0.665372744069761));
#46166=CARTESIAN_POINT('Ctrl Pts',(-0.0740161983599743,-0.00117148387544626,
-0.665273190924778));
#46167=CARTESIAN_POINT('Ctrl Pts',(-0.0734718979508283,-0.0266986788458054,
-0.663064417441171));
#46168=CARTESIAN_POINT('Ctrl Pts',(-0.044097535312672,-0.0752734101305599,
-0.65874642361894));
#46169=CARTESIAN_POINT('Ctrl Pts',(0.0390428582906939,-0.0780149608077107,
-0.652418762603067));
#46170=CARTESIAN_POINT('Ctrl Pts',(0.0866843980931254,-0.00982313700242362,
-0.646091101587197));
#46171=CARTESIAN_POINT('Ctrl Pts',(0.0555100696561328,0.0673001564642097,
-0.639763440571324));
#46172=CARTESIAN_POINT('Ctrl Pts',(-0.0261355596403159,0.0832322738823306,
-0.633435779555452));
#46173=CARTESIAN_POINT('Ctrl Pts',(-0.0700153218516501,0.0379405554487119,
-0.628638880721598));
#46174=CARTESIAN_POINT('Ctrl Pts',(-0.0739278816139727,0.00678466603221187,
-0.625951202226367));
#46175=CARTESIAN_POINT('Ctrl Pts',(-0.0738702015529844,6.49156969421468E-5,
-0.625372744069761));
#46176=CARTESIAN_POINT('Origin',(0.,0.,-1.05327725593024));
#46177=CARTESIAN_POINT('',(-0.0738501444728052,6.13634501804807E-5,-0.713277255930238));
#46178=CARTESIAN_POINT('',(-0.0738134589801114,-4.70777110323853E-5,-0.705372744069761));
#46179=CARTESIAN_POINT('',(-0.0739,6.54188504088864E-16,-1.05327725593024));
#46180=CARTESIAN_POINT('Ctrl Pts',(-0.0738501444728051,6.13634501804728E-5,
-0.713277255930238));
#46181=CARTESIAN_POINT('Ctrl Pts',(-0.0737146405834979,-0.0170012191686346,
-0.711809464419114));
#46182=CARTESIAN_POINT('Ctrl Pts',(-0.0593652872484897,-0.0587885221188445,
-0.708232452569367));
#46183=CARTESIAN_POINT('Ctrl Pts',(0.00999574615152227,-0.0866646653884117,
-0.702546220380994));
#46184=CARTESIAN_POINT('Ctrl Pts',(0.0780925597784293,-0.0388874179557339,
-0.696218559365122));
#46185=CARTESIAN_POINT('Ctrl Pts',(0.0751854437781816,0.0442473525975172,
-0.68989089834925));
#46186=CARTESIAN_POINT('Ctrl Pts',(0.00391762895901338,0.0871511982209692,
-0.683563237333377));
#46187=CARTESIAN_POINT('Ctrl Pts',(-0.0615723981039191,0.0553500429250213,
-0.678025356527042));
#46188=CARTESIAN_POINT('Ctrl Pts',(-0.0737237789786778,0.0153132915896411,
-0.674596696059328));
#46189=CARTESIAN_POINT('Ctrl Pts',(-0.0738107316200561,-4.54136549985842E-5,
-0.673277255930238));
#46190=CARTESIAN_POINT('Ctrl Pts',(-0.0738134589801114,-4.70777110323862E-5,
-0.705372744069761));
#46191=CARTESIAN_POINT('Ctrl Pts',(-0.0738667027928598,-0.00909733596711184,
-0.704595179623188));
#46192=CARTESIAN_POINT('Ctrl Pts',(-0.068142195106051,-0.0426323122661008,
-0.701708394837992));
#46193=CARTESIAN_POINT('Ctrl Pts',(-0.0182226522121619,-0.0853147926193951,
-0.696712389714172));
#46194=CARTESIAN_POINT('Ctrl Pts',(0.0615711950922978,-0.0618034532064518,
-0.690384728698299));
#46195=CARTESIAN_POINT('Ctrl Pts',(0.0853827975350567,0.0179013066121811,
-0.684057067682429));
#46196=CARTESIAN_POINT('Ctrl Pts',(0.0315619832053435,0.0813297000454412,
-0.677729406666555));
#46197=CARTESIAN_POINT('Ctrl Pts',(-0.0496576109998276,0.0709763587008032,
-0.671501298795667));
#46198=CARTESIAN_POINT('Ctrl Pts',(-0.0739248955866761,0.0232091332474935,
-0.667382411263402));
#46199=CARTESIAN_POINT('Ctrl Pts',(-0.0740118889580303,-2.07425011238048E-5,
-0.665372744069761));
#46200=CARTESIAN_POINT('Origin',(0.,0.,-1.05327725593024));
#46201=CARTESIAN_POINT('',(-0.0740181195037208,-7.75676069538861E-6,-0.753277255930239));
#46202=CARTESIAN_POINT('',(-0.0738464406987289,6.04347504972284E-5,-0.745372744069761));
#46203=CARTESIAN_POINT('',(-0.0739,6.54188504088864E-16,-1.05327725593024));
#46204=CARTESIAN_POINT('Ctrl Pts',(-0.0740181195037208,-7.75676069538801E-6,
-0.753277255930239));
#46205=CARTESIAN_POINT('Ctrl Pts',(-0.0740187541717008,-0.000430520586765759,
-0.753240673456149));
#46206=CARTESIAN_POINT('Ctrl Pts',(-0.07382453043895,-0.0252278019321763,
-0.751094870643435));
#46207=CARTESIAN_POINT('Ctrl Pts',(-0.0463114749636612,-0.0739319041732507,
-0.746839847492097));
#46208=CARTESIAN_POINT('Ctrl Pts',(0.0367109763098753,-0.0791390130490189,
-0.740512186476226));
#46209=CARTESIAN_POINT('Ctrl Pts',(0.0863547858049027,-0.0123907278484321,
-0.734184525460353));
#46210=CARTESIAN_POINT('Ctrl Pts',(0.0574824197298575,0.0656235520983735,
-0.727856864444481));
#46211=CARTESIAN_POINT('Ctrl Pts',(-0.0236545628063002,0.0839710713665869,
-0.72152920342861));
#46212=CARTESIAN_POINT('Ctrl Pts',(-0.069452220378256,0.0394239899284276,
-0.716669333923862));
#46213=CARTESIAN_POINT('Ctrl Pts',(-0.073909360035902,0.00751775782251194,
-0.713918684757738));
#46214=CARTESIAN_POINT('Ctrl Pts',(-0.0738501444728051,6.13634501804728E-5,
-0.713277255930238));
#46215=CARTESIAN_POINT('Ctrl Pts',(-0.0738464406987288,6.04347504972241E-5,
-0.745372744069761));
#46216=CARTESIAN_POINT('Ctrl Pts',(-0.0737145788249443,-0.0168622901615721,
-0.743917168321599));
#46217=CARTESIAN_POINT('Ctrl Pts',(-0.0595540578546233,-0.0585065533281464,
-0.740352372234814));
#46218=CARTESIAN_POINT('Ctrl Pts',(0.00949669427259201,-0.0867207685115116,
-0.734678355809403));
#46219=CARTESIAN_POINT('Ctrl Pts',(0.0778674086249794,-0.0393363135965772,
-0.728350694793532));
#46220=CARTESIAN_POINT('Ctrl Pts',(0.0754389070476233,0.0438138128538845,
-0.722023033777659));
#46221=CARTESIAN_POINT('Ctrl Pts',(0.00441925078978631,0.0871272007801963,
-0.715695372761787));
#46222=CARTESIAN_POINT('Ctrl Pts',(-0.0613976166205516,0.0556342510285772,
-0.710145276192489));
#46223=CARTESIAN_POINT('Ctrl Pts',(-0.0737222736934459,0.0154523831817844,
-0.706704399961813));
#46224=CARTESIAN_POINT('Ctrl Pts',(-0.0738134589801114,-4.70777110323862E-5,
-0.705372744069761));
#46225=CARTESIAN_POINT('Origin',(0.,0.,-1.05327725593024));
#46226=CARTESIAN_POINT('',(-0.0738290934588786,-5.47168357983042E-5,-0.793277255930239));
#46227=CARTESIAN_POINT('',(-0.0740186890690066,-5.17471746349502E-6,-0.785372744069761));
#46228=CARTESIAN_POINT('',(-0.0739,6.54188504088864E-16,-1.05327725593024));
#46229=CARTESIAN_POINT('Ctrl Pts',(-0.0738290934588786,-5.47168357983097E-5,
-0.793277255930239));
#46230=CARTESIAN_POINT('Ctrl Pts',(-0.0738867553000471,-0.0083676131166434,
-0.79256266215456));
#46231=CARTESIAN_POINT('Ctrl Pts',(-0.0687641349176097,-0.0411481838791359,
-0.789738848040257));
#46232=CARTESIAN_POINT('Ctrl Pts',(-0.0207459093066268,-0.0847365707051847,
-0.784805813587329));
#46233=CARTESIAN_POINT('Ctrl Pts',(0.0597103888730514,-0.0636030551758837,
-0.778478152571458));
#46234=CARTESIAN_POINT('Ctrl Pts',(0.0858763390381331,0.0153601289709793,
-0.772150491555585));
#46235=CARTESIAN_POINT('Ctrl Pts',(0.0339611307424576,0.0803574561980857,
-0.765822830539714));
#46236=CARTESIAN_POINT('Ctrl Pts',(-0.0483538236456822,0.0723381788220632,
-0.75953175199793));
#46237=CARTESIAN_POINT('Ctrl Pts',(-0.0739821613866291,0.0239445957105796,
-0.755349893794773));
#46238=CARTESIAN_POINT('Ctrl Pts',(-0.0740181195037208,-7.75676069538801E-6,
-0.753277255930239));
#46239=CARTESIAN_POINT('Ctrl Pts',(-0.0740186890690066,-5.17471746348515E-6,
-0.785372744069761));
#46240=CARTESIAN_POINT('Ctrl Pts',(-0.0740189752447098,-0.000286761730465124,
-0.785348377358633));
#46241=CARTESIAN_POINT('Ctrl Pts',(-0.0738903489069693,-0.0249426889494393,
-0.783214790308882));
#46242=CARTESIAN_POINT('Ctrl Pts',(-0.0467362966021223,-0.0736640853684918,
-0.778971982920508));
#46243=CARTESIAN_POINT('Ctrl Pts',(0.0362548028063699,-0.0793490275094065,
-0.772644321904634));
#46244=CARTESIAN_POINT('Ctrl Pts',(0.0862820260894591,-0.0128876245803302,
-0.766316660888764));
#46245=CARTESIAN_POINT('Ctrl Pts',(0.0578592289600791,0.0652915654389009,
-0.759988999872889));
#46246=CARTESIAN_POINT('Ctrl Pts',(-0.0231707900729891,0.0841058462933171,
-0.753661338857021));
#46247=CARTESIAN_POINT('Ctrl Pts',(-0.0693398833707779,0.0397118294936949,
-0.748789253589309));
#46248=CARTESIAN_POINT('Ctrl Pts',(-0.0739056549310326,0.00765979713931138,
-0.746026388660223));
#46249=CARTESIAN_POINT('Ctrl Pts',(-0.0738464406987288,6.04347504972241E-5,
-0.745372744069761));
#46250=CARTESIAN_POINT('Origin',(0.,0.,-1.05327725593024));
#46251=CARTESIAN_POINT('',(-0.0738285525876018,5.44975647950647E-5,-0.833277255930239));
#46252=CARTESIAN_POINT('',(-0.0738324075238535,-5.60022767805285E-5,-0.825372744069761));
#46253=CARTESIAN_POINT('',(-0.0739,6.54188504088864E-16,-1.05327725593024));
#46254=CARTESIAN_POINT('Ctrl Pts',(-0.0738285525876017,5.44975647950637E-5,
-0.833277255930239));
#46255=CARTESIAN_POINT('Ctrl Pts',(-0.0737166860120861,-0.0161460284618373,
-0.83188465085297));
#46256=CARTESIAN_POINT('Ctrl Pts',(-0.0605070205977865,-0.0570495580085797,
-0.828382825437078));
#46257=CARTESIAN_POINT('Ctrl Pts',(0.00691951974818428,-0.0869643572919913,
-0.82277177968256));
#46258=CARTESIAN_POINT('Ctrl Pts',(0.0766660252567158,-0.0416293128401549,
-0.81644411866669));
#46259=CARTESIAN_POINT('Ctrl Pts',(0.0767056471347569,0.0415562617250705,
-0.810116457650816));
#46260=CARTESIAN_POINT('Ctrl Pts',(0.00700235840066891,0.0869577262010798,
-0.803788796634946));
#46261=CARTESIAN_POINT('Ctrl Pts',(-0.0604769485808272,0.0570964171803072,
-0.798175729394752));
#46262=CARTESIAN_POINT('Ctrl Pts',(-0.073716558564091,0.0161690264472331,
-0.794671882493184));
#46263=CARTESIAN_POINT('Ctrl Pts',(-0.0738290934588786,-5.47168357983097E-5,
-0.793277255930239));
#46264=CARTESIAN_POINT('Ctrl Pts',(-0.0738324075238535,-5.60022767805354E-5,
-0.825372744069761));
#46265=CARTESIAN_POINT('Ctrl Pts',(-0.0738905913104309,-0.00822586691819469,
-0.824670366057044));
#46266=CARTESIAN_POINT('Ctrl Pts',(-0.0688815793035972,-0.0408602812647409,
-0.821858767705704));
#46267=CARTESIAN_POINT('Ctrl Pts',(-0.0212333521088858,-0.0846157411642612,
-0.816937949015739));
#46268=CARTESIAN_POINT('Ctrl Pts',(0.0593432667534829,-0.0639457236824982,
-0.810610287999866));
#46269=CARTESIAN_POINT('Ctrl Pts',(0.0859633353842028,0.014865526115561,
-0.804282626983996));
#46270=CARTESIAN_POINT('Ctrl Pts',(0.0344231459854351,0.0801606257062834,
-0.797954965968122));
#46271=CARTESIAN_POINT('Ctrl Pts',(-0.0480965289443807,0.072600677106953,
-0.79165167166338));
#46272=CARTESIAN_POINT('Ctrl Pts',(-0.0739942034316283,0.0240878472108019,
-0.787457597697257));
#46273=CARTESIAN_POINT('Ctrl Pts',(-0.0740186890690066,-5.17471746348515E-6,
-0.785372744069761));
#46274=CARTESIAN_POINT('Origin',(0.,0.,-1.05327725593024));
#46275=CARTESIAN_POINT('',(-0.0740179768487384,8.17838895347943E-6,-0.873277255930239));
#46276=CARTESIAN_POINT('',(-0.0738253349991919,5.31336276900878E-5,-0.865372744069761));
#46277=CARTESIAN_POINT('',(-0.0739,6.54188504088864E-16,-1.05327725593024));
#46278=CARTESIAN_POINT('Ctrl Pts',(-0.0740179768487384,8.17838895347957E-6,
-0.873277255930238));
#46279=CARTESIAN_POINT('Ctrl Pts',(-0.0739801514683282,-0.0239209166759214,
-0.871206639551381));
#46280=CARTESIAN_POINT('Ctrl Pts',(-0.0483963153428398,-0.0722946776724089,
-0.8670268028339));
#46281=CARTESIAN_POINT('Ctrl Pts',(0.0338845940526951,-0.0803897756396443,
-0.860737745777792));
#46282=CARTESIAN_POINT('Ctrl Pts',(0.0858616535090988,-0.0154419256785799,
-0.854410084761921));
#46283=CARTESIAN_POINT('Ctrl Pts',(0.0597709578444863,0.0635461448157645,
-0.848082423746049));
#46284=CARTESIAN_POINT('Ctrl Pts',(-0.0206651836539401,0.0847562955128429,
-0.841754762730177));
#46285=CARTESIAN_POINT('Ctrl Pts',(-0.0687445992449014,0.0411958268432829,
-0.836819706791573));
#46286=CARTESIAN_POINT('Ctrl Pts',(-0.0738861175760961,0.00839106360363198,
-0.833993871191594));
#46287=CARTESIAN_POINT('Ctrl Pts',(-0.0738285525876017,5.44975647950637E-5,
-0.833277255930239));
#46288=CARTESIAN_POINT('Ctrl Pts',(-0.0738253349991919,5.31336276900912E-5,
-0.865372744069761));
#46289=CARTESIAN_POINT('Ctrl Pts',(-0.0737175361431159,-0.0160070434472833,
-0.863992354755455));
#46290=CARTESIAN_POINT('Ctrl Pts',(-0.0606880120450771,-0.0567662717423334,
-0.860502745102525));
#46291=CARTESIAN_POINT('Ctrl Pts',(0.00641879698876544,-0.0870027483201755,
-0.85490391511097));
#46292=CARTESIAN_POINT('Ctrl Pts',(0.076425112291304,-0.0420699505040234,
-0.8485762540951));
#46293=CARTESIAN_POINT('Ctrl Pts',(0.0769435948053001,0.0411140152158757,
-0.842248593079225));
#46294=CARTESIAN_POINT('Ctrl Pts',(0.0075028148617241,0.0869159748679489,
-0.835920932063356));
#46295=CARTESIAN_POINT('Ctrl Pts',(-0.0602944965619087,0.0573794653213463,
-0.830295649060199));
#46296=CARTESIAN_POINT('Ctrl Pts',(-0.0737158671251557,0.0163079942697733,
-0.826779586395668));
#46297=CARTESIAN_POINT('Ctrl Pts',(-0.0738324075238535,-5.60022767805354E-5,
-0.825372744069761));
#46298=CARTESIAN_POINT('Origin',(0.,0.,-1.05327725593024));
#46299=CARTESIAN_POINT('',(-0.0738511720378038,-6.144379322435E-5,-0.913277255930239));
#46300=CARTESIAN_POINT('',(-0.0740169999568149,1.06868542633972E-5,-0.905372744069761));
#46301=CARTESIAN_POINT('',(-0.0739,6.54188504088864E-16,-1.05327725593024));
#46302=CARTESIAN_POINT('Ctrl Pts',(-0.0738511720378038,-6.14437932243417E-5,
-0.913277255930239));
#46303=CARTESIAN_POINT('Ctrl Pts',(-0.0739097105108123,-0.00749428940729366,
-0.912637848588415));
#46304=CARTESIAN_POINT('Ctrl Pts',(-0.0694677457128137,-0.0393768397509905,
-0.909889220907968));
#46305=CARTESIAN_POINT('Ctrl Pts',(-0.0237369667204929,-0.0839481073924034,
-0.905031372888896));
#46306=CARTESIAN_POINT('Ctrl Pts',(0.0574211581950477,-0.0656784871371439,
-0.898703711873025));
#46307=CARTESIAN_POINT('Ctrl Pts',(0.0863658764533893,0.0123085695241889,
-0.892376050857153));
#46308=CARTESIAN_POINT('Ctrl Pts',(0.0367867028056418,0.0791039486621042,
-0.88604838984128));
#46309=CARTESIAN_POINT('Ctrl Pts',(-0.0462412134555447,0.0739760173765286,
-0.879720728825409));
#46310=CARTESIAN_POINT('Ctrl Pts',(-0.0738135527330108,0.0252749890993244,
-0.875463684188394));
#46311=CARTESIAN_POINT('Ctrl Pts',(-0.074018682053951,0.000454305364743116,
-0.873315859890004));
#46312=CARTESIAN_POINT('Ctrl Pts',(-0.0740179768487384,8.17838895347957E-6,
-0.873277255930238));
#46313=CARTESIAN_POINT('Ctrl Pts',(-0.0740169999568149,1.06868542633994E-5,
-0.905372744069761));
#46314=CARTESIAN_POINT('Ctrl Pts',(-0.0739682091453213,-0.0237779860315713,
-0.903314343453865));
#46315=CARTESIAN_POINT('Ctrl Pts',(-0.0486522352802609,-0.0720314229341465,
-0.899146722499347));
#46316=CARTESIAN_POINT('Ctrl Pts',(0.0334214198190593,-0.0805835554203335,
-0.892869881206202));
#46317=CARTESIAN_POINT('Ctrl Pts',(0.0857712573590327,-0.0159359034660176,
-0.88654222019033));
#46318=CARTESIAN_POINT('Ctrl Pts',(0.0601358128673054,0.0632010030064432,
-0.880214559174458));
#46319=CARTESIAN_POINT('Ctrl Pts',(-0.0201769626930229,0.084873857253752,
-0.873886898158586));
#46320=CARTESIAN_POINT('Ctrl Pts',(-0.0686259403155307,0.0414837324433979,
-0.868939626457021));
#46321=CARTESIAN_POINT('Ctrl Pts',(-0.0738822516602237,0.00853273803129299,
-0.866101575094079));
#46322=CARTESIAN_POINT('Ctrl Pts',(-0.0738253349991919,5.31336276900912E-5,
-0.865372744069761));
#46323=CARTESIAN_POINT('Origin',(0.,0.,-1.05327725593024));
#46324=CARTESIAN_POINT('',(-0.0739,6.54188504088864E-16,-0.949325));
#46325=CARTESIAN_POINT('',(-0.0738572813634733,-6.14771210490569E-5,-0.945372744069761));
#46326=CARTESIAN_POINT('',(-0.0739,6.54188504088864E-16,-1.05327725593024));
#46327=CARTESIAN_POINT('',(-0.0601104350279399,-0.0429877377952343,-0.949325));
#46328=CARTESIAN_POINT('Origin',(0.,0.,-0.949325));
#46329=CARTESIAN_POINT('Ctrl Pts',(-0.0601104350279403,-0.0429877377952337,
-0.949325));
#46330=CARTESIAN_POINT('Ctrl Pts',(-0.0458679287777906,-0.0629032599997909,
-0.947215779661376));
#46331=CARTESIAN_POINT('Ctrl Pts',(0.00371043826886423,-0.0871365202941097,
-0.942997338984126));
#46332=CARTESIAN_POINT('Ctrl Pts',(0.0752041131369929,-0.0443285976848148,
-0.936669677968258));
#46333=CARTESIAN_POINT('Ctrl Pts',(0.0780980364899326,0.0388180903923549,
-0.930342016952383));
#46334=CARTESIAN_POINT('Ctrl Pts',(0.0100948570851079,0.0866524255516566,
-0.924014355936512));
#46335=CARTESIAN_POINT('Ctrl Pts',(-0.0593400932047787,0.0588361590846621,
-0.918326102262464));
#46336=CARTESIAN_POINT('Ctrl Pts',(-0.0737166089778999,0.0170245237460521,
-0.914747068927039));
#46337=CARTESIAN_POINT('Ctrl Pts',(-0.0738511720378038,-6.14437932243417E-5,
-0.913277255930239));
#46338=CARTESIAN_POINT('Ctrl Pts',(-0.0738572813634733,-6.14771210490526E-5,
-0.945372744069761));
#46339=CARTESIAN_POINT('Ctrl Pts',(-0.0739120474282235,-0.0073527222198075,
-0.9447455524909));
#46340=CARTESIAN_POINT('Ctrl Pts',(-0.0695624069951655,-0.0390950973922719,
-0.942009140573414));
#46341=CARTESIAN_POINT('Ctrl Pts',(-0.0242332971309306,-0.0838051103417385,
-0.937163508317307));
#46342=CARTESIAN_POINT('Ctrl Pts',(0.0570492242990965,-0.06601055836573,
-0.930835847301434));
#46343=CARTESIAN_POINT('Ctrl Pts',(0.0864315571449822,0.0118125778999351,
-0.924508186285562));
#46344=CARTESIAN_POINT('Ctrl Pts',(0.0372434277651266,0.0788901466696481,
-0.91818052526969));
#46345=CARTESIAN_POINT('Ctrl Pts',(-0.0458156426390635,0.0742413616113632,
-0.911852864253818));
#46346=CARTESIAN_POINT('Ctrl Pts',(-0.0737467241149971,0.0255601749070422,
-0.907583603853842));
#46347=CARTESIAN_POINT('Ctrl Pts',(-0.0740182045500766,0.000598003895852526,
-0.905423563792489));
#46348=CARTESIAN_POINT('Ctrl Pts',(-0.0740169999568149,1.06868542633994E-5,
-0.905372744069761));
#46349=CARTESIAN_POINT('Origin',(2.39206768658147E-17,-5.43753587379397E-18,
-0.013325));
#46350=CARTESIAN_POINT('',(-0.0452560140322625,0.0854280329804665,-0.013325));
#46351=CARTESIAN_POINT('Ctrl Pts',(0.0740154662741574,-0.000526981588892629,
-0.013325));
#46352=CARTESIAN_POINT('Ctrl Pts',(0.0743274162787444,0.00138720916901943,
-0.0133249999999999));
#46353=CARTESIAN_POINT('Ctrl Pts',(0.0745584091685309,0.00331039779856178,
-0.0133250000000001));
#46354=CARTESIAN_POINT('Ctrl Pts',(0.0747064997395148,0.00523801887942489,
-0.0133250000000002));
#46355=CARTESIAN_POINT('Ctrl Pts',(0.0750471992924708,0.0096727349869759,
-0.0133250000000002));
#46356=CARTESIAN_POINT('Ctrl Pts',(0.0749501667319329,0.0141305889760572,
-0.0133250000000002));
#46357=CARTESIAN_POINT('Ctrl Pts',(0.0744523966822522,0.0185654001727163,
-0.0133250000000004));
#46358=CARTESIAN_POINT('Ctrl Pts',(0.0741100333998832,0.0216156369616686,
-0.0133250000000006));
#46359=CARTESIAN_POINT('Ctrl Pts',(0.0735783232628857,0.0246476071870298,
-0.0133249999999998));
#46360=CARTESIAN_POINT('Ctrl Pts',(0.0728709746069023,0.0276395260463149,
-0.0133249999999999));
#46361=CARTESIAN_POINT('Ctrl Pts',(0.0719811966983897,0.0314030778429219,
-0.0133250000000001));
#46362=CARTESIAN_POINT('Ctrl Pts',(0.0708133325873436,0.0351067594379044,
-0.0133250000000001));
#46363=CARTESIAN_POINT('Ctrl Pts',(0.069386882975893,0.0387224916969436,
-0.0133250000000001));
#46364=CARTESIAN_POINT('Ctrl Pts',(0.0684028077464189,0.0412169033634814,
-0.0133250000000002));
#46365=CARTESIAN_POINT('Ctrl Pts',(0.0672972189702868,0.0436644443409473,
-0.0133250000000002));
#46366=CARTESIAN_POINT('Ctrl Pts',(0.0660807270923872,0.0460490974145337,
-0.0133250000000002));
#46367=CARTESIAN_POINT('Ctrl Pts',(0.0630085800683589,0.0520713364252927,
-0.0133250000000003));
#46368=CARTESIAN_POINT('Ctrl Pts',(0.0592273612473775,0.0577071685296467,
-0.0133250000000001));
#46369=CARTESIAN_POINT('Ctrl Pts',(0.054825249512648,0.0628151653134337,
-0.0133250000000001));
#46370=CARTESIAN_POINT('Ctrl Pts',(0.0527049155254095,0.0652754979537713,
-0.0133250000000001));
#46371=CARTESIAN_POINT('Ctrl Pts',(0.0504362001885655,0.0676156486678103,
-0.0133250000000002));
#46372=CARTESIAN_POINT('Ctrl Pts',(0.0480475571159952,0.0697999749756303,
-0.0133250000000002));
#46373=CARTESIAN_POINT('Ctrl Pts',(0.0460015562349771,0.071670967591292,
-0.0133250000000001));
#46374=CARTESIAN_POINT('Ctrl Pts',(0.0438653825571326,0.0734306648289896,
-0.0133250000000002));
#46375=CARTESIAN_POINT('Ctrl Pts',(0.0416450739245558,0.0750698920282756,
-0.0133250000000002));
#46376=CARTESIAN_POINT('Ctrl Pts',(0.0374507997065208,0.0781664743135446,
-0.0133250000000002));
#46377=CARTESIAN_POINT('Ctrl Pts',(0.0329571089215552,0.0808340896140399,
-0.0133250000000002));
#46378=CARTESIAN_POINT('Ctrl Pts',(0.0282314170935856,0.0830783479911864,
-0.0133250000000001));
#46379=CARTESIAN_POINT('Ctrl Pts',(0.0254273460850914,0.0844100175286878,
-0.0133250000000001));
#46380=CARTESIAN_POINT('Ctrl Pts',(0.0225383922404567,0.0855928024630465,
-0.0133250000000001));
#46381=CARTESIAN_POINT('Ctrl Pts',(0.0196009575542751,0.0866189242160582,
-0.0133250000000001));
#46382=CARTESIAN_POINT('Ctrl Pts',(0.0144103595069212,0.0884321340867615,
-0.0133250000000002));
#46383=CARTESIAN_POINT('Ctrl Pts',(0.00905575240102509,0.0897644221558753,
-0.0133250000000002));
#46384=CARTESIAN_POINT('Ctrl Pts',(0.00361197019240061,0.0906224587811647,
-0.0133250000000002));
#46385=CARTESIAN_POINT('Ctrl Pts',(-0.000441340334494331,0.0912613324084449,
-0.0133250000000001));
#46386=CARTESIAN_POINT('Ctrl Pts',(-0.00454446622826156,0.0916370240537867,
-0.0133250000000001));
#46387=CARTESIAN_POINT('Ctrl Pts',(-0.00866962335769465,0.0917466885842836,
-0.0133250000000001));
#46388=CARTESIAN_POINT('Ctrl Pts',(-0.0114737278358596,0.0918212338176926,
-0.0133250000000001));
#46389=CARTESIAN_POINT('Ctrl Pts',(-0.014279644527722,0.0917723286717455,
-0.013325));
#46390=CARTESIAN_POINT('Ctrl Pts',(-0.0170720954237708,0.091600917740833,
-0.013325));
#46391=CARTESIAN_POINT('Ctrl Pts',(-0.0245642157420065,0.0911410237745421,
-0.013325));
#46392=CARTESIAN_POINT('Ctrl Pts',(-0.0319725491600437,0.0898033415291956,
-0.0133249999999999));
#46393=CARTESIAN_POINT('Ctrl Pts',(-0.039131992857135,0.0875766958826527,
-0.0133250000000001));
#46394=CARTESIAN_POINT('Ctrl Pts',(-0.041195285566919,0.0869349949455183,
-0.0133250000000001));
#46395=CARTESIAN_POINT('Ctrl Pts',(-0.0432379503387495,0.0862191367302635,
-0.013325));
#46396=CARTESIAN_POINT('Ctrl Pts',(-0.0452560140322624,0.0854280329804665,
-0.013325));
#46397=CARTESIAN_POINT('',(-0.096675,-1.1839272930757E-17,-0.013325));
#46398=CARTESIAN_POINT('Origin',(0.,0.,-0.013325));
#46399=CARTESIAN_POINT('',(-0.0953105349179715,0.0166374124980891,-0.0133249999999999));
#46400=CARTESIAN_POINT('Origin',(0.,0.,-0.013325));
#46401=CARTESIAN_POINT('Ctrl Pts',(-0.0953893049619548,0.0166325119362263,
-0.0133249999999998));
#46402=CARTESIAN_POINT('Ctrl Pts',(-0.0955491516473957,0.0141405248991806,
-0.0133249999999998));
#46403=CARTESIAN_POINT('Ctrl Pts',(-0.0956055203501725,0.0116461842161637,
-0.0133249999999999));
#46404=CARTESIAN_POINT('Ctrl Pts',(-0.0955546587076807,0.00915419853455082,
-0.0133249999999998));
#46405=CARTESIAN_POINT('Ctrl Pts',(-0.0954492895571674,0.00399159659135037,
-0.0133249999999998));
#46406=CARTESIAN_POINT('Ctrl Pts',(-0.0948843160835839,-0.00116127963385684,
-0.013325));
#46407=CARTESIAN_POINT('Ctrl Pts',(-0.0938852470810883,-0.00625275390846729,
-0.0133250000000003));
#46408=CARTESIAN_POINT('Ctrl Pts',(-0.093293720913368,-0.00926730070972282,
-0.0133250000000004));
#46409=CARTESIAN_POINT('Ctrl Pts',(-0.092549661853774,-0.0122589890978512,
-0.0133250000000002));
#46410=CARTESIAN_POINT('Ctrl Pts',(-0.0916618445562462,-0.0152047979384899,
-0.0133250000000002));
#46411=CARTESIAN_POINT('Ctrl Pts',(-0.0899959881019879,-0.020732167909602,
-0.0133250000000002));
#46412=CARTESIAN_POINT('Ctrl Pts',(-0.0878227127820439,-0.0261107468918155,
-0.0133250000000002));
#46413=CARTESIAN_POINT('Ctrl Pts',(-0.085173648547477,-0.0312627955199005,
-0.0133250000000003));
#46414=CARTESIAN_POINT('Ctrl Pts',(-0.0838153418310689,-0.0339045065677011,
-0.0133250000000004));
#46415=CARTESIAN_POINT('Ctrl Pts',(-0.0823348229585785,-0.0364799319891756,
-0.0133250000000005));
#46416=CARTESIAN_POINT('Ctrl Pts',(-0.0807412291085146,-0.0389724889468894,
-0.0133250000000004));
#46417=CARTESIAN_POINT('Ctrl Pts',(-0.0769763666135518,-0.0448611501049876,
-0.0133250000000003));
#46418=CARTESIAN_POINT('Ctrl Pts',(-0.072575731259438,-0.0503026910650738,
-0.013325));
#46419=CARTESIAN_POINT('Ctrl Pts',(-0.067591694538167,-0.0551448578224046,
-0.0133250000000001));
#46420=CARTESIAN_POINT('Ctrl Pts',(-0.0650390110357168,-0.0576248795174292,
-0.0133250000000001));
#46421=CARTESIAN_POINT('Ctrl Pts',(-0.0623280400111939,-0.0599498046813196,
-0.0133250000000003));
#46422=CARTESIAN_POINT('Ctrl Pts',(-0.0594904268278414,-0.0620765235258152,
-0.0133250000000003));
#46423=CARTESIAN_POINT('Ctrl Pts',(-0.0573688668117999,-0.0636665787498022,
-0.0133250000000003));
#46424=CARTESIAN_POINT('Ctrl Pts',(-0.0551746319546616,-0.0651481417695435,
-0.0133250000000003));
#46425=CARTESIAN_POINT('Ctrl Pts',(-0.0529107688590407,-0.0665124204372184,
-0.0133250000000003));
#46426=CARTESIAN_POINT('Ctrl Pts',(-0.0488178690201689,-0.0689789370520721,
-0.0133250000000003));
#46427=CARTESIAN_POINT('Ctrl Pts',(-0.044497278097604,-0.0710627972144308,
-0.0133250000000002));
#46428=CARTESIAN_POINT('Ctrl Pts',(-0.040004671478209,-0.0727554835895005,
-0.0133250000000002));
#46429=CARTESIAN_POINT('Ctrl Pts',(-0.0368908382283995,-0.0739286873802436,
-0.0133250000000002));
#46430=CARTESIAN_POINT('Ctrl Pts',(-0.0336895004235565,-0.0749142680218583,
-0.0133249999999998));
#46431=CARTESIAN_POINT('Ctrl Pts',(-0.0304486889041091,-0.0757008149597433,
-0.013325));
#46432=CARTESIAN_POINT('Ctrl Pts',(-0.0259717963066162,-0.0767873595312704,
-0.0133250000000001));
#46433=CARTESIAN_POINT('Ctrl Pts',(-0.0214104423515735,-0.0774991875316017,
-0.0133250000000001));
#46434=CARTESIAN_POINT('Ctrl Pts',(-0.0168162976082181,-0.0778292284117383,
-0.013325));
#46435=CARTESIAN_POINT('Ctrl Pts',(-0.0135048506864013,-0.0780671209723031,
-0.0133249999999999));
#46436=CARTESIAN_POINT('Ctrl Pts',(-0.0101763407192596,-0.078106396707891,
-0.0133250000000004));
#46437=CARTESIAN_POINT('Ctrl Pts',(-0.00685168166603567,-0.0779406634282734,
-0.0133250000000005));
#46438=CARTESIAN_POINT('Ctrl Pts',(-0.0044924871884174,-0.0778230582748511,
-0.0133250000000006));
#46439=CARTESIAN_POINT('Ctrl Pts',(-0.00213599500253028,-0.0776018117801322,
-0.013325));
#46440=CARTESIAN_POINT('Ctrl Pts',(0.000197121312828762,-0.0772768152441007,
-0.013325));
#46441=CARTESIAN_POINT('Ctrl Pts',(0.00625486133427826,-0.0764329891089909,
-0.0133250000000001));
#46442=CARTESIAN_POINT('Ctrl Pts',(0.0121811594338303,-0.0748919729606164,
-0.0133250000000003));
#46443=CARTESIAN_POINT('Ctrl Pts',(0.017838523980557,-0.0726157902902942,
-0.0133250000000001));
#46444=CARTESIAN_POINT('Ctrl Pts',(0.0197116627554222,-0.0718621520929956,
-0.0133250000000001));
#46445=CARTESIAN_POINT('Ctrl Pts',(0.0215550621983123,-0.0710275991192391,
-0.0133250000000002));
#46446=CARTESIAN_POINT('Ctrl Pts',(0.0233628051714133,-0.070109837644389,
-0.0133250000000002));
#46447=CARTESIAN_POINT('Ctrl Pts',(0.0663714283216842,0.0324968229607071,
-0.962474152380794));
#46448=CARTESIAN_POINT('Ctrl Pts',(0.0556047253532112,0.0544867096396884,
-0.96036493204217));
#46449=CARTESIAN_POINT('Ctrl Pts',(0.0106964331164646,0.0865570854208283,
-0.95614649136492));
#46450=CARTESIAN_POINT('Ctrl Pts',(-0.0668730934586114,0.0561130448027703,
-0.949818830349052));
#46451=CARTESIAN_POINT('Ctrl Pts',(-0.0834262416657708,-0.0254206125080873,
-0.943491169333177));
#46452=CARTESIAN_POINT('Ctrl Pts',(-0.0242332971309306,-0.0838051103417385,
-0.937163508317307));
#46453=CARTESIAN_POINT('Ctrl Pts',(0.0570492242990965,-0.06601055836573,
-0.930835847301434));
#46454=CARTESIAN_POINT('Ctrl Pts',(0.0864315571449822,0.0118125778999351,
-0.924508186285562));
#46455=CARTESIAN_POINT('Ctrl Pts',(0.0372434277651266,0.0788901466696481,
-0.91818052526969));
#46456=CARTESIAN_POINT('Ctrl Pts',(-0.0458156426390635,0.0742413616113632,
-0.911852864253818));
#46457=CARTESIAN_POINT('Ctrl Pts',(-0.0872135427032971,0.00208880626078628,
-0.905525203237946));
#46458=CARTESIAN_POINT('Ctrl Pts',(-0.0493167351776861,-0.0719621815782819,
-0.899197542222075));
#46459=CARTESIAN_POINT('Ctrl Pts',(0.0334214198190593,-0.0805835554203335,
-0.892869881206202));
#46460=CARTESIAN_POINT('Ctrl Pts',(0.0857712573590327,-0.0159359034660176,
-0.88654222019033));
#46461=CARTESIAN_POINT('Ctrl Pts',(0.0601358128673054,0.0632010030064432,
-0.880214559174458));
#46462=CARTESIAN_POINT('Ctrl Pts',(-0.0201769626930229,0.084873857253752,
-0.873886898158586));
#46463=CARTESIAN_POINT('Ctrl Pts',(-0.0821441893694497,0.029377006100539,
-0.867559237142714));
#46464=CARTESIAN_POINT('Ctrl Pts',(-0.0694236808259852,-0.0528302204192478,
-0.861231576126843));
#46465=CARTESIAN_POINT('Ctrl Pts',(0.00641879698876544,-0.0870027483201755,
-0.85490391511097));
#46466=CARTESIAN_POINT('Ctrl Pts',(0.076425112291304,-0.0420699505040234,
-0.8485762540951));
#46467=CARTESIAN_POINT('Ctrl Pts',(0.0769435948053001,0.0411140152158757,
-0.842248593079225));
#46468=CARTESIAN_POINT('Ctrl Pts',(0.0075028148617241,0.0869159748679489,
-0.835920932063356));
#46469=CARTESIAN_POINT('Ctrl Pts',(-0.0687597312600683,0.0536915095569343,
-0.829593271047482));
#46470=CARTESIAN_POINT('Ctrl Pts',(-0.0825040163400733,-0.0283507707839517,
-0.823265610031611));
#46471=CARTESIAN_POINT('Ctrl Pts',(-0.0212333521088858,-0.0846157411642612,
-0.816937949015739));
#46472=CARTESIAN_POINT('Ctrl Pts',(0.0593432667534829,-0.0639457236824982,
-0.810610287999866));
#46473=CARTESIAN_POINT('Ctrl Pts',(0.0859633353842028,0.014865526115561,
-0.804282626983996));
#46474=CARTESIAN_POINT('Ctrl Pts',(0.0344231459854351,0.0801606257062834,
-0.797954965968122));
#46475=CARTESIAN_POINT('Ctrl Pts',(-0.0484155261201637,0.0725714525340945,
-0.791627304952252));
#46476=CARTESIAN_POINT('Ctrl Pts',(-0.0872334539001633,-0.00100170583074655,
-0.785299643936378));
#46477=CARTESIAN_POINT('Ctrl Pts',(-0.0467362966021223,-0.0736640853684918,
-0.778971982920508));
#46478=CARTESIAN_POINT('Ctrl Pts',(0.0362548028063699,-0.0793490275094065,
-0.772644321904634));
#46479=CARTESIAN_POINT('Ctrl Pts',(0.0862820260894591,-0.0128876245803302,
-0.766316660888764));
#46480=CARTESIAN_POINT('Ctrl Pts',(0.0578592289600791,0.0652915654389009,
-0.759988999872889));
#46481=CARTESIAN_POINT('Ctrl Pts',(-0.0231707900729891,0.0841058462933171,
-0.753661338857021));
#46482=CARTESIAN_POINT('Ctrl Pts',(-0.0831332816440542,0.0264487499976755,
-0.747333677841146));
#46483=CARTESIAN_POINT('Ctrl Pts',(-0.0675086789221911,-0.0552562861900129,
-0.741006016825276));
#46484=CARTESIAN_POINT('Ctrl Pts',(0.00949669427259201,-0.0867207685115116,
-0.734678355809403));
#46485=CARTESIAN_POINT('Ctrl Pts',(0.0778674086249794,-0.0393363135965772,
-0.728350694793532));
#46486=CARTESIAN_POINT('Ctrl Pts',(0.0754389070476233,0.0438138128538845,
-0.722023033777659));
#46487=CARTESIAN_POINT('Ctrl Pts',(0.00441925078978631,0.0871272007801963,
-0.715695372761787));
#46488=CARTESIAN_POINT('Ctrl Pts',(-0.070618511328248,0.0512221119353569,
-0.709367711745916));
#46489=CARTESIAN_POINT('Ctrl Pts',(-0.0814479567647437,-0.0312555472225994,
-0.703040050730043));
#46490=CARTESIAN_POINT('Ctrl Pts',(-0.0182226522121619,-0.0853147926193951,
-0.696712389714172));
#46491=CARTESIAN_POINT('Ctrl Pts',(0.0615711950922978,-0.0618034532064518,
-0.690384728698299));
#46492=CARTESIAN_POINT('Ctrl Pts',(0.0853827975350567,0.0179013066121811,
-0.684057067682429));
#46493=CARTESIAN_POINT('Ctrl Pts',(0.0315619832053435,0.0813297000454412,
-0.677729406666555));
#46494=CARTESIAN_POINT('Ctrl Pts',(-0.0509558650129233,0.0708108657913499,
-0.671401745650684));
#46495=CARTESIAN_POINT('Ctrl Pts',(-0.087143222032879,-0.00409117917771768,
-0.665074084634812));
#46496=CARTESIAN_POINT('Ctrl Pts',(-0.044097535312672,-0.0752734101305599,
-0.65874642361894));
#46497=CARTESIAN_POINT('Ctrl Pts',(0.0390428582906939,-0.0780149608077107,
-0.652418762603067));
#46498=CARTESIAN_POINT('Ctrl Pts',(0.0866843980931254,-0.00982313700242362,
-0.646091101587197));
#46499=CARTESIAN_POINT('Ctrl Pts',(0.0555100696561328,0.0673001564642097,
-0.639763440571324));
#46500=CARTESIAN_POINT('Ctrl Pts',(-0.0261355596403159,0.0832322738823306,
-0.633435779555452));
#46501=CARTESIAN_POINT('Ctrl Pts',(-0.0840180104376559,0.0234872905085658,
-0.62710811853958));
#46502=CARTESIAN_POINT('Ctrl Pts',(-0.0655089468902942,-0.0576129913358129,
-0.620780457523708));
#46503=CARTESIAN_POINT('Ctrl Pts',(0.012562675089579,-0.0863299373793905,
-0.614452796507836));
#46504=CARTESIAN_POINT('Ctrl Pts',(0.0792119631042182,-0.0365533007334742,
-0.608125135491964));
#46505=CARTESIAN_POINT('Ctrl Pts',(0.0738395288211365,0.0464586146673402,
-0.601797474476092));
#46506=CARTESIAN_POINT('Ctrl Pts',(0.00133013907144687,0.0872290640978479,
-0.59546981346022));
#46507=CARTESIAN_POINT('Ctrl Pts',(-0.0723886501561355,0.0486884197926824,
-0.589142152444349));
#46508=CARTESIAN_POINT('Ctrl Pts',(-0.0802896631951301,-0.0341210913856576,
-0.582814491428475));
#46509=CARTESIAN_POINT('Ctrl Pts',(-0.0151890790080958,-0.0859067562664407,
-0.576486830412606));
#46510=CARTESIAN_POINT('Ctrl Pts',(0.0637218387120179,-0.0595836065079599,
-0.570159169396731));
#46511=CARTESIAN_POINT('Ctrl Pts',(0.0846950865125139,0.0209146172322998,
-0.563831508380862));
#46512=CARTESIAN_POINT('Ctrl Pts',(0.0286612035496907,0.0823966886738722,
-0.557503847364987));
#46513=CARTESIAN_POINT('Ctrl Pts',(-0.053432243674384,0.0689613966597043,
-0.551176186349117));
#46514=CARTESIAN_POINT('Ctrl Pts',(-0.0869436072730663,-0.00717551724147037,
-0.544848525333244));
#46515=CARTESIAN_POINT('Ctrl Pts',(-0.0414034224289421,-0.076788251083785,
-0.538520864317373));
#46516=CARTESIAN_POINT('Ctrl Pts',(0.0417819068541502,-0.0765829690790775,
-0.532193203301501));
#46517=CARTESIAN_POINT('Ctrl Pts',(0.0869779631209978,-0.00674631934155149,
-0.525865542285629));
#46518=CARTESIAN_POINT('Ctrl Pts',(0.0530912336515535,0.0692242717743709,
-0.519537881269757));
#46519=CARTESIAN_POINT('Ctrl Pts',(-0.0290675236360216,0.0822542276299836,
-0.513210220253885));
#46520=CARTESIAN_POINT('Ctrl Pts',(-0.0847972791269669,0.0204963495774027,
-0.506882559238013));
#46521=CARTESIAN_POINT('Ctrl Pts',(-0.0634269874842546,-0.0598973801764987,
-0.500554898222141));
#46522=CARTESIAN_POINT('Ctrl Pts',(0.015612887132456,-0.0858307441930048,
-0.494227237206269));
#46523=CARTESIAN_POINT('Ctrl Pts',(0.0804570900696259,-0.0337244058637655,
-0.487899576190397));
#46524=CARTESIAN_POINT('Ctrl Pts',(0.0721474666049248,0.0490451012418884,
-0.481571915174525));
#46525=CARTESIAN_POINT('Ctrl Pts',(-0.00176064224849756,0.087221436769917,
-0.475244254158653));
#46526=CARTESIAN_POINT('Ctrl Pts',(-0.0740679261492535,0.04609361354119,
-0.468916593142781));
#46527=CARTESIAN_POINT('Ctrl Pts',(-0.0790305893735705,-0.0369438064714765,
-0.462588932126909));
#46528=CARTESIAN_POINT('Ctrl Pts',(-0.0121364403459336,-0.0863908890396749,
-0.456261271111038));
#46529=CARTESIAN_POINT('Ctrl Pts',(0.0657924981506585,-0.0572889699718141,
-0.449933610095165));
#46530=CARTESIAN_POINT('Ctrl Pts',(0.0839010655140964,0.0239016756511994,
-0.443605949079294));
#46531=CARTESIAN_POINT('Ctrl Pts',(0.0257244481133483,0.0833602522944807,
-0.437278288063421));
#46532=CARTESIAN_POINT('Ctrl Pts',(-0.0558415537398982,0.0670253666103355,
-0.43095062704755));
#46533=CARTESIAN_POINT('Ctrl Pts',(-0.0866348601754494,-0.0102508485363977,
-0.424622966031677));
#46534=CARTESIAN_POINT('Ctrl Pts',(-0.0386573396255769,-0.078206706786622,
-0.418295305015806));
#46535=CARTESIAN_POINT('Ctrl Pts',(0.0444685104211786,-0.0750548497717326,
-0.411967643999933));
#46536=CARTESIAN_POINT('Ctrl Pts',(0.0871623526873201,-0.00366103364462123,
-0.405639982984062));
#46537=CARTESIAN_POINT('Ctrl Pts',(0.0506057570896398,0.0710614962037825,
-0.399312321968189));
#46538=CARTESIAN_POINT('Ctrl Pts',(-0.0319630018346919,0.081172935188099,
-0.392984660952318));
#46539=CARTESIAN_POINT('Ctrl Pts',(-0.085470109567385,0.0174796814580538,
-0.386656999936446));
#46540=CARTESIAN_POINT('Ctrl Pts',(-0.0612654139968446,-0.0621065853282167,
-0.380329338920573));
#46541=CARTESIAN_POINT('Ctrl Pts',(0.0186435017497599,-0.0852238155437934,
-0.374001677904702));
#46542=CARTESIAN_POINT('Ctrl Pts',(0.0816012266274847,-0.0308531798397786,
-0.367674016888829));
#46543=CARTESIAN_POINT('Ctrl Pts',(0.0703648442895387,0.0515700259981008,
-0.361346355872959));
#46544=CARTESIAN_POINT('Ctrl Pts',(-0.0048492135956714,0.0871043283702904,
-0.355018694857085));
#46545=CARTESIAN_POINT('Ctrl Pts',(-0.0756542314664302,0.043440950203232,
-0.348691033841215));
#46546=CARTESIAN_POINT('Ctrl Pts',(-0.0776723156999812,-0.039720149384642,
-0.342363372825342));
#46547=CARTESIAN_POINT('Ctrl Pts',(-0.00906856792307098,-0.086766583251621,
-0.33603571180947));
#46548=CARTESIAN_POINT('Ctrl Pts',(0.0677805742992985,-0.0549224238448479,
-0.329708050793598));
#46549=CARTESIAN_POINT('Ctrl Pts',(0.0830017312015545,0.0268587324883495,
-0.323380389777726));
#46550=CARTESIAN_POINT('Ctrl Pts',(0.0227554031361251,0.0842191814342093,
-0.317052728761854));
#46551=CARTESIAN_POINT('Ctrl Pts',(-0.0581807710234661,0.0650052057642372,
-0.310725067745983));
#46552=CARTESIAN_POINT('Ctrl Pts',(-0.0862173682819487,-0.0133133128811225,
-0.30439740673011));
#46553=CARTESIAN_POINT('Ctrl Pts',(-0.0358627338085138,-0.0795269967816936,
-0.298069745714238));
#46554=CARTESIAN_POINT('Ctrl Pts',(0.0470992967446723,-0.0734325209937202,
-0.291742084698366));
#46555=CARTESIAN_POINT('Ctrl Pts',(0.0872373353447779,-0.000571152587860333,
-0.285414423682494));
#46556=CARTESIAN_POINT('Ctrl Pts',(0.0480567597612106,0.0728095236530848,
-0.279086762666623));
#46557=CARTESIAN_POINT('Ctrl Pts',(-0.0348183598080465,0.0799897538039288,
-0.27275910165075));
#46558=CARTESIAN_POINT('Ctrl Pts',(-0.0860356572165558,0.0144410726973928,
-0.266431440634879));
#46559=CARTESIAN_POINT('Ctrl Pts',(-0.0590269396530525,-0.0642378337783162,
-0.260103779619007));
#46560=CARTESIAN_POINT('Ctrl Pts',(0.0216507148888523,-0.0845099132536343,
-0.253776118603134));
#46561=CARTESIAN_POINT('Ctrl Pts',(0.0826429366480972,-0.0279432266482656,
-0.247448457587263));
#46562=CARTESIAN_POINT('Ctrl Pts',(0.0684938994372912,0.0540302196294675,
-0.241120796571391));
#46563=CARTESIAN_POINT('Ctrl Pts',(-0.00793169816963801,0.0868778858943854,
-0.234793135555519));
#46564=CARTESIAN_POINT('Ctrl Pts',(-0.077145574964127,0.0407337594238917,
-0.228465474539647));
#46565=CARTESIAN_POINT('Ctrl Pts',(-0.0762165470906266,-0.0424466352365409,
-0.222137813523775));
#46566=CARTESIAN_POINT('Ctrl Pts',(-0.00598931255869429,-0.0870333673276597,
-0.215810152507903));
#46567=CARTESIAN_POINT('Ctrl Pts',(0.0696835717087142,-0.0524869386356467,
-0.209482491492031));
#46568=CARTESIAN_POINT('Ctrl Pts',(0.0819982124259003,0.0297820760219009,
-0.203154830476159));
#46569=CARTESIAN_POINT('Ctrl Pts',(0.0197577953896086,0.0849723979572207,
-0.196827169460287));
#46570=CARTESIAN_POINT('Ctrl Pts',(-0.0604469593233129,0.062903449845688,
-0.190499508444415));
#46571=CARTESIAN_POINT('Ctrl Pts',(-0.085691655625816,-0.0163590662480221,
-0.184171847428543));
#46572=CARTESIAN_POINT('Ctrl Pts',(-0.0330231128016351,-0.0807474638242463,
-0.177844186412671));
#46573=CARTESIAN_POINT('Ctrl Pts',(0.0496709636615209,-0.0717180191165734,
-0.171516525396799));
#46574=CARTESIAN_POINT('Ctrl Pts',(0.0872028169333057,0.00251944540519899,
-0.165188864380927));
#46575=CARTESIAN_POINT('Ctrl Pts',(0.0454474412670434,0.0744661599442045,
-0.158861203365055));
#46576=CARTESIAN_POINT('Ctrl Pts',(-0.0376300136353005,0.078706168691497,
-0.152533542349183));
#46577=CARTESIAN_POINT('Ctrl Pts',(-0.0864932119131863,0.0113843372402568,
-0.146205881333311));
#46578=CARTESIAN_POINT('Ctrl Pts',(-0.0567143747377854,-0.0662884500965085,
-0.139878220317439));
#46579=CARTESIAN_POINT('Ctrl Pts',(0.0246307528823777,-0.083689933929838,
-0.133550559301567));
#46580=CARTESIAN_POINT('Ctrl Pts',(0.0835809106498128,-0.0249981979169972,
-0.127222898285695));
#46581=CARTESIAN_POINT('Ctrl Pts',(0.0665369841126368,0.0564225922414199,
-0.120895237269823));
#46582=CARTESIAN_POINT('Ctrl Pts',(-0.0110042337120753,0.0865423970628537,
-0.114567576253952));
#46583=CARTESIAN_POINT('Ctrl Pts',(-0.0785400716048779,0.0379754326755566,
-0.108239915238079));
#46584=CARTESIAN_POINT('Ctrl Pts',(-0.0746651356672856,-0.0451198291711274,
-0.101912254222208));
#46585=CARTESIAN_POINT('Ctrl Pts',(-0.00290249226713311,-0.0871909301984517,
-0.0955845932063355));
#46586=CARTESIAN_POINT('Ctrl Pts',(0.0714990124011491,-0.0499855262439841,
-0.0892569321904637));
#46587=CARTESIAN_POINT('Ctrl Pts',(0.0808919382230671,0.032667951227759,
-0.0829292711745915));
#46588=CARTESIAN_POINT('Ctrl Pts',(0.0167350661775352,0.0856191188118938,
-0.0766016101587197));
#46589=CARTESIAN_POINT('Ctrl Pts',(-0.0626366646621712,0.0607224289900663,
-0.0702739491428476));
#46590=CARTESIAN_POINT('Ctrl Pts',(-0.0850595379996997,-0.0193837013910442,
-0.0639462881269757));
#46591=CARTESIAN_POINT('Ctrl Pts',(-0.0301398485007547,-0.0818676840127184,
-0.0576186271111039));
#46592=CARTESIAN_POINT('Ctrl Pts',(0.0521761247033908,-0.0699113944796167,
-0.0512909660952318));
#46593=CARTESIAN_POINT('Ctrl Pts',(0.0870667295313287,0.00560289368117736,
-0.04496330507936));
#46594=CARTESIAN_POINT('Ctrl Pts',(0.0427661024466595,0.0760368969037317,
-0.0386356440634878));
#46595=CARTESIAN_POINT('Ctrl Pts',(-0.0403659317628278,0.0773093583706435,
-0.032307983047616));
#46596=CARTESIAN_POINT('Ctrl Pts',(-0.0868971070713012,0.00834129536707174,
-0.025980322031744));
#46597=CARTESIAN_POINT('Ctrl Pts',(-0.0542193581796284,-0.0683140096653152,
-0.0196526610158722));
#46598=CARTESIAN_POINT('Ctrl Pts',(0.00013432532901024,-0.0778502984302035,
-0.015434220338624));
#46599=CARTESIAN_POINT('Ctrl Pts',(0.0233628051714152,-0.0701098376443883,
-0.013325));
#46600=CARTESIAN_POINT('Ctrl Pts',(0.0731896930038058,0.0358351862576404,
-0.958091101587196));
#46601=CARTESIAN_POINT('Ctrl Pts',(0.0613169383433753,0.0600840700909465,
-0.955981881248572));
#46602=CARTESIAN_POINT('Ctrl Pts',(0.0117952660629124,0.0954490007138341,
-0.951763440571324));
#46603=CARTESIAN_POINT('Ctrl Pts',(-0.0737428936549124,0.0618774768974165,
-0.945435779555452));
#46604=CARTESIAN_POINT('Ctrl Pts',(-0.0919965287832173,-0.02803204439745,
-0.93910811853958));
#46605=CARTESIAN_POINT('Ctrl Pts',(-0.0267227574022744,-0.0924143182264165,
-0.932780457523708));
#46606=CARTESIAN_POINT('Ctrl Pts',(0.0629098290957223,-0.0727917512695617,
-0.926452796507837));
#46607=CARTESIAN_POINT('Ctrl Pts',(0.0953105770546664,0.0130260711866786,
-0.920125135491964));
#46608=CARTESIAN_POINT('Ctrl Pts',(0.0410694046137993,0.086994445679126,
-0.913797474476093));
#46609=CARTESIAN_POINT('Ctrl Pts',(-0.0505222338032704,0.0818680959852864,
-0.907469813460219));
#46610=CARTESIAN_POINT('Ctrl Pts',(-0.0961728951393259,0.00230338705731037,
-0.901142152444349));
#46611=CARTESIAN_POINT('Ctrl Pts',(-0.0543829897725069,-0.0793547782649999,
-0.894814491428476));
#46612=CARTESIAN_POINT('Ctrl Pts',(0.0368547659461639,-0.0888618164699416,
-0.888486830412605));
#46613=CARTESIAN_POINT('Ctrl Pts',(0.0945824453894882,-0.0175729815058846,
-0.882159169396731));
#46614=CARTESIAN_POINT('Ctrl Pts',(0.0663134995522529,0.0696935733423554,
-0.875831508380861));
#46615=CARTESIAN_POINT('Ctrl Pts',(-0.0222497201370175,0.093592856346915,
-0.869503847364988));
#46616=CARTESIAN_POINT('Ctrl Pts',(-0.0905827726481562,0.0323948740028382,
-0.863176186349117));
#46617=CARTESIAN_POINT('Ctrl Pts',(-0.0765555000899085,-0.0582574115335841,
-0.856848525333245));
#46618=CARTESIAN_POINT('Ctrl Pts',(0.00707819302583869,-0.0959404460783713,
-0.850520864317372));
#46619=CARTESIAN_POINT('Ctrl Pts',(0.0842761809987215,-0.0463917507869694,
-0.844193203301502));
#46620=CARTESIAN_POINT('Ctrl Pts',(0.0848479266577615,0.0453376133058242,
-0.837865542285628));
#46621=CARTESIAN_POINT('Ctrl Pts',(0.00827357087649971,0.0958447584837249,
-0.831537881269757));
#46622=CARTESIAN_POINT('Ctrl Pts',(-0.0758233437068345,0.0592071799681169,
-0.825210220253884));
#46623=CARTESIAN_POINT('Ctrl Pts',(-0.0909795642523203,-0.0312632146477519,
-0.818882559238014));
#46624=CARTESIAN_POINT('Ctrl Pts',(-0.0234146312892188,-0.093308224272137,
-0.812554898222141));
#46625=CARTESIAN_POINT('Ctrl Pts',(0.0654395360376984,-0.0705147983639095,
-0.806227237206269));
#46626=CARTESIAN_POINT('Ctrl Pts',(0.0947942553813848,0.0163926454537744,
-0.799899576190397));
#46627=CARTESIAN_POINT('Ctrl Pts',(0.0379593983526802,0.0883954396461148,
-0.793571915174525));
#46628=CARTESIAN_POINT('Ctrl Pts',(-0.0533892004881688,0.0800266389637921,
-0.787244254158654));
#46629=CARTESIAN_POINT('Ctrl Pts',(-0.0961948517918018,-0.00110460998183024,
-0.780916593142781));
#46630=CARTESIAN_POINT('Ctrl Pts',(-0.0515374655471529,-0.0812315167815159,
-0.774588932126909));
#46631=CARTESIAN_POINT('Ctrl Pts',(0.039979219287719,-0.0875004668487241,
-0.768261271111037));
#46632=CARTESIAN_POINT('Ctrl Pts',(0.0951456848363578,-0.0142115562439161,
-0.761933610095165));
#46633=CARTESIAN_POINT('Ctrl Pts',(0.0638030446550082,0.0719988969809441,
-0.755605949079294));
#46634=CARTESIAN_POINT('Ctrl Pts',(-0.0255511001492739,0.0927459484553843,
-0.74927828806342));
#46635=CARTESIAN_POINT('Ctrl Pts',(-0.0916734732969335,0.0291658013337019,
-0.74295062704755));
#46636=CARTESIAN_POINT('Ctrl Pts',(-0.0744437721222492,-0.0609327044037141,
-0.736622966031678));
#46637=CARTESIAN_POINT('Ctrl Pts',(0.0104722793517905,-0.0956294987904907,
-0.730295305015805));
#46638=CARTESIAN_POINT('Ctrl Pts',(0.0858666428669004,-0.0433772903316337,
-0.723967643999934));
#46639=CARTESIAN_POINT('Ctrl Pts',(0.0831886639624164,0.0483147582203582,
-0.717639982984062));
#46640=CARTESIAN_POINT('Ctrl Pts',(0.00487323561945417,0.0960776834043234,
-0.71131232196819));
#46641=CARTESIAN_POINT('Ctrl Pts',(-0.0778730742308229,0.0564841038132446,
-0.704984660952317));
#46642=CARTESIAN_POINT('Ctrl Pts',(-0.0898150168248115,-0.0344663956122913,
-0.698656999936446));
#46643=CARTESIAN_POINT('Ctrl Pts',(-0.0200946454648996,-0.0940790885233498,
-0.692329338920573));
#46644=CARTESIAN_POINT('Ctrl Pts',(0.0678963370328801,-0.0681524547706237,
-0.686001677904703));
#46645=CARTESIAN_POINT('Ctrl Pts',(0.0941540795100721,0.0197402883807532,
-0.679674016888829));
#46646=CARTESIAN_POINT('Ctrl Pts',(0.03480431143043,0.0896846117212867,
-0.673346355872958));
#46647=CARTESIAN_POINT('Ctrl Pts',(-0.0561905056338947,0.0780851890588194,
-0.667018694857086));
#46648=CARTESIAN_POINT('Ctrl Pts',(-0.0960953505028781,-0.00451146156730964,
-0.660691033841214));
#46649=CARTESIAN_POINT('Ctrl Pts',(-0.0486276271789151,-0.0830061657269673,
-0.654363372825342));
#46650=CARTESIAN_POINT('Ctrl Pts',(0.0430536886811791,-0.0860293529249665,
-0.648035711809471));
#46651=CARTESIAN_POINT('Ctrl Pts',(0.0955893920785604,-0.0108322571883965,
-0.641708050793598));
#46652=CARTESIAN_POINT('Ctrl Pts',(0.0612125587694319,0.0742138283788349,
-0.635380389777726));
#46653=CARTESIAN_POINT('Ctrl Pts',(-0.0288204372713859,0.091782634900238,
-0.629052728761854));
#46654=CARTESIAN_POINT('Ctrl Pts',(-0.0926490893177534,0.0259001143305441,
-0.622725067745983));
#46655=CARTESIAN_POINT('Ctrl Pts',(-0.0722386097925335,-0.063531511307275,
-0.61639740673011));
#46656=CARTESIAN_POINT('Ctrl Pts',(0.0138532250452181,-0.0951985180010217,
-0.610069745714238));
#46657=CARTESIAN_POINT('Ctrl Pts',(0.0873493219661874,-0.0403083815823909,
-0.603742084698366));
#46658=CARTESIAN_POINT('Ctrl Pts',(0.0814249833493339,0.0512312576490662,
-0.597414423682494));
#46659=CARTESIAN_POINT('Ctrl Pts',(0.00146678281232274,0.0961900110298664,
-0.591086762666623));
#46660=CARTESIAN_POINT('Ctrl Pts',(-0.0798250574962617,0.0536901282310149,
-0.58475910165075));
#46661=CARTESIAN_POINT('Ctrl Pts',(-0.0885377330159198,-0.0376263140122176,
-0.578431440634879));
#46662=CARTESIAN_POINT('Ctrl Pts',(-0.0167494365832395,-0.0947318639523595,
-0.572103779619006));
#46663=CARTESIAN_POINT('Ctrl Pts',(0.0702679139337871,-0.0657045656338903,
-0.565776118603135));
#46664=CARTESIAN_POINT('Ctrl Pts',(0.0933957206817628,0.0230631531252437,
-0.559448457587262));
#46665=CARTESIAN_POINT('Ctrl Pts',(0.031605537834058,0.0908612109316414,
-0.553120796571392));
#46666=CARTESIAN_POINT('Ctrl Pts',(-0.0589212799832885,0.0760457259737537,
-0.546793135555518));
#46667=CARTESIAN_POINT('Ctrl Pts',(-0.095875229535782,-0.00791265032750778,
-0.540465474539648));
#46668=CARTESIAN_POINT('Ctrl Pts',(-0.0456567510072874,-0.0846766246446023,
-0.534137813523774));
#46669=CARTESIAN_POINT('Ctrl Pts',(0.046074116726064,-0.0844502542427039,
-0.527810152507903));
#46670=CARTESIAN_POINT('Ctrl Pts',(0.0959131147226248,-0.00743936139389169,
-0.521482491492031));
#46671=CARTESIAN_POINT('Ctrl Pts',(0.058545238371509,0.0763356059631905,
-0.515154830476159));
#46672=CARTESIAN_POINT('Ctrl Pts',(-0.0320535987411656,0.0907041150195771,
-0.508827169460288));
#46673=CARTESIAN_POINT('Ctrl Pts',(-0.0935084114324098,0.0226019172888386,
-0.502499508444415));
#46674=CARTESIAN_POINT('Ctrl Pts',(-0.0699427729599149,-0.0660505729303092,
-0.496171847428543));
#46675=CARTESIAN_POINT('Ctrl Pts',(0.0172167820555128,-0.0946480432412487,
-0.489844186412671));
#46676=CARTESIAN_POINT('Ctrl Pts',(0.0887223594712305,-0.0371888774178803,
-0.483516525396799));
#46677=CARTESIAN_POINT('Ctrl Pts',(0.0795590974210148,0.0540834511777658,
-0.477188864380928));
#46678=CARTESIAN_POINT('Ctrl Pts',(-0.00194151111277164,0.0961816001548283,
-0.470861203365055));
#46679=CARTESIAN_POINT('Ctrl Pts',(-0.081676843686688,0.0508287603540027,
-0.464533542349184));
#46680=CARTESIAN_POINT('Ctrl Pts',(-0.0871493159093535,-0.0407390035503574,
-0.458205881333311));
#46681=CARTESIAN_POINT('Ctrl Pts',(-0.0133832036696982,-0.0952657311591092,
-0.45187822031744));
#46682=CARTESIAN_POINT('Ctrl Pts',(0.0725512899656393,-0.0631742035807814,
-0.445550559301567));
#46683=CARTESIAN_POINT('Ctrl Pts',(0.0925201307693222,0.0263570688084213,
-0.439222898285696));
#46684=CARTESIAN_POINT('Ctrl Pts',(0.0283670927041534,0.0919237603955488,
-0.432895237269823));
#46685=CARTESIAN_POINT('Ctrl Pts',(-0.0615780958527814,0.0739108096619836,
-0.426567576253952));
#46686=CARTESIAN_POINT('Ctrl Pts',(-0.0955347651844519,-0.0113039070633101,
-0.420239915238079));
#46687=CARTESIAN_POINT('Ctrl Pts',(-0.0426285661026744,-0.0862407967598531,
-0.413912254222208));
#46688=CARTESIAN_POINT('Ctrl Pts',(0.0490367121570486,-0.0827651529000646,
-0.407584593206335));
#46689=CARTESIAN_POINT('Ctrl Pts',(0.096116446428654,-0.00403712765118974,
-0.401256932190464));
#46690=CARTESIAN_POINT('Ctrl Pts',(0.0558044315042385,0.0783615664610724,
-0.394929271174592));
#46691=CARTESIAN_POINT('Ctrl Pts',(-0.0352465262676424,0.0895117425805614,
-0.388601610158719));
#46692=CARTESIAN_POINT('Ctrl Pts',(-0.0942503610125686,0.0192753501328719,
-0.382273949142848));
#46693=CARTESIAN_POINT('Ctrl Pts',(-0.0675591433778916,-0.0684867273257366,
-0.375946288126975));
#46694=CARTESIAN_POINT('Ctrl Pts',(0.0205587284180089,-0.0939787654716684,
-0.369618627111104));
#46695=CARTESIAN_POINT('Ctrl Pts',(0.0899840319339393,-0.0340226934656285,
-0.363290966095232));
#46696=CARTESIAN_POINT('Ctrl Pts',(0.0775933482529769,0.0568677587094528,
-0.356963305079361));
#46697=CARTESIAN_POINT('Ctrl Pts',(-0.005347368036995,0.0960524613366115,
-0.350635644063487));
#46698=CARTESIAN_POINT('Ctrl Pts',(-0.0834261084246978,0.0479035917949261,
-0.344307983047617));
#46699=CARTESIAN_POINT('Ctrl Pts',(-0.0856515082577939,-0.043800557152956,
-0.337980322031744));
#46700=CARTESIAN_POINT('Ctrl Pts',(-0.0100001720477796,-0.0956800200290485,
-0.331652661015872));
#46701=CARTESIAN_POINT('Ctrl Pts',(0.0747435990158817,-0.0605645447427567,
-0.325325));
#46702=CARTESIAN_POINT('Ctrl Pts',(0.0915284088204783,0.0296179008799696,
-0.318997338984128));
#46703=CARTESIAN_POINT('Ctrl Pts',(0.0250930409639339,0.0928709263920988,
-0.312669677968256));
#46704=CARTESIAN_POINT('Ctrl Pts',(-0.0641576183850333,0.0716831198881908,
-0.306342016952384));
#46705=CARTESIAN_POINT('Ctrl Pts',(-0.0950743848025683,-0.0146809750411026,
-0.300014355936512));
#46706=CARTESIAN_POINT('Ctrl Pts',(-0.0395468734679134,-0.0876967187108911,
-0.293686694920641));
#46707=CARTESIAN_POINT('Ctrl Pts',(0.0519377562997463,-0.0809761640502468,
-0.287359033904768));
#46708=CARTESIAN_POINT('Ctrl Pts',(0.0961991319730023,-0.00062982647233715,
-0.281031372888897));
#46709=CARTESIAN_POINT('Ctrl Pts',(0.0529935784511589,0.0802891668700402,
-0.274703711873025));
#46710=CARTESIAN_POINT('Ctrl Pts',(-0.0383952120616697,0.0882070142589782,
-0.268376050857152));
#46711=CARTESIAN_POINT('Ctrl Pts',(-0.0948740067569576,0.0159245883973617,
-0.26204838984128));
#46712=CARTESIAN_POINT('Ctrl Pts',(-0.0650907129981055,-0.0708369166123314,
-0.255720728825409));
#46713=CARTESIAN_POINT('Ctrl Pts',(0.0238748692938754,-0.093191524775292,
-0.249393067809537));
#46714=CARTESIAN_POINT('Ctrl Pts',(0.0911327556925737,-0.0308138039460294,
-0.243065406793665));
#46715=CARTESIAN_POINT('Ctrl Pts',(0.075530203269877,0.0595806853582052,
-0.236737745777793));
#46716=CARTESIAN_POINT('Ctrl Pts',(-0.00874651290041614,0.0958027566713121,
-0.230410084761921));
#46717=CARTESIAN_POINT('Ctrl Pts',(-0.0850706560187414,0.0449182942496883,
-0.224082423746049));
#46718=CARTESIAN_POINT('Ctrl Pts',(-0.0840461901217001,-0.0468071319325816,
-0.217754762730177));
#46719=CARTESIAN_POINT('Ctrl Pts',(-0.00660458812713927,-0.0959742105432099,
-0.211427101714305));
#46720=CARTESIAN_POINT('Ctrl Pts',(0.0768420892805049,-0.0578788647855197,
-0.205099440698433));
#46721=CARTESIAN_POINT('Ctrl Pts',(0.0904217996518807,0.0328415563168887,
-0.198771779682561));
#46722=CARTESIAN_POINT('Ctrl Pts',(0.0217874922321812,0.0937015200297318,
-0.192444118666689));
#46723=CARTESIAN_POINT('Ctrl Pts',(-0.0666566097454531,0.0693654528688523,
-0.186116457650817));
#46724=CARTESIAN_POINT('Ctrl Pts',(-0.0944946662567494,-0.0180396153404836,
-0.179788796634945));
#46725=CARTESIAN_POINT('Ctrl Pts',(-0.0364155412818212,-0.0890425630060109,
-0.173461135619073));
#46726=CARTESIAN_POINT('Ctrl Pts',(0.0547736077634206,-0.079085533259018,
-0.167133474603201));
#46727=CARTESIAN_POINT('Ctrl Pts',(0.0961610675226428,0.00277826529290049,
-0.160805813587329));
#46728=CARTESIAN_POINT('Ctrl Pts',(0.0501162075045576,0.0821159876064926,
-0.154478152571457));
#46729=CARTESIAN_POINT('Ctrl Pts',(-0.0414957040301764,0.0867915678432734,
-0.148150491555585));
#46730=CARTESIAN_POINT('Ctrl Pts',(-0.0953785655501859,0.0125538378295524,
-0.141822830539713));
#46731=CARTESIAN_POINT('Ctrl Pts',(-0.0625405808029773,-0.0730981905157598,
-0.135495169523841));
#46732=CARTESIAN_POINT('Ctrl Pts',(0.0271610433510118,-0.0922873098669243,
-0.129167508507969));
#46733=CARTESIAN_POINT('Ctrl Pts',(0.0921670867438566,-0.0275662356146048,
-0.122839847492097));
#46734=CARTESIAN_POINT('Ctrl Pts',(0.0733722561611948,0.0622188238079439,
-0.116512186476225));
#46735=CARTESIAN_POINT('Ctrl Pts',(-0.0121346866791143,0.0954328034368117,
-0.110184525460353));
#46736=CARTESIAN_POINT('Ctrl Pts',(-0.0866084077835025,0.0418766075929485,
-0.103856864444482));
#46737=CARTESIAN_POINT('Ctrl Pts',(-0.0823354038893083,-0.0497549401741605,
-0.0975292034286096));
#46738=CARTESIAN_POINT('Ctrl Pts',(-0.00320066214256808,-0.0961479596764388,
-0.0912015424127376));
#46739=CARTESIAN_POINT('Ctrl Pts',(0.0788440282217904,-0.0551204850180334,
-0.0848738813968658));
#46740=CARTESIAN_POINT('Ctrl Pts',(0.089201879102771,0.0360238943455408,
-0.0785462203809937));
#46741=CARTESIAN_POINT('Ctrl Pts',(0.018454241334023,0.0944146778147846,
-0.0722185593651218));
#46742=CARTESIAN_POINT('Ctrl Pts',(-0.069071261133443,0.0669603781116214,
-0.0658908983492497));
#46743=CARTESIAN_POINT('Ctrl Pts',(-0.0937976118740486,-0.0213749679638049,
-0.0595632373333777));
#46744=CARTESIAN_POINT('Ctrl Pts',(-0.0332360823735769,-0.0902778621967042,
-0.053235576317506));
#46745=CARTESIAN_POINT('Ctrl Pts',(0.0575361212758751,-0.0770933160370063,
-0.0469079153016338));
#46746=CARTESIAN_POINT('Ctrl Pts',(0.0960110000097951,0.0061784728583936,
-0.0405802542857622));
#46747=CARTESIAN_POINT('Ctrl Pts',(0.0471594176619174,0.0838480846663952,
-0.0342525932698898));
#46748=CARTESIAN_POINT('Ctrl Pts',(-0.0445126800528523,0.0852512647165678,
-0.0279249322540182));
#46749=CARTESIAN_POINT('Ctrl Pts',(-0.0958239524188379,0.00919818757268762,
-0.021597271238146));
#46750=CARTESIAN_POINT('Ctrl Pts',(-0.0597892539060201,-0.0753318336171761,
-0.0152696102222743));
#46751=CARTESIAN_POINT('Ctrl Pts',(0.000148124424040622,-0.085847774960415,
-0.0110511695450261));
#46752=CARTESIAN_POINT('Ctrl Pts',(0.0257628407500305,-0.0773121450523764,
-0.00894194920640212));
#46753=CARTESIAN_POINT('Ctrl Pts',(0.0800079576859273,0.0391735495545737,
-0.953708050793598));
#46754=CARTESIAN_POINT('Ctrl Pts',(0.0670291513335393,0.0656814305422046,
-0.951598830454974));
#46755=CARTESIAN_POINT('Ctrl Pts',(0.0128940990093602,0.10434091600684,
-0.947380389777726));
#46756=CARTESIAN_POINT('Ctrl Pts',(-0.0806126938512132,0.0676419089920627,
-0.941052728761855));
#46757=CARTESIAN_POINT('Ctrl Pts',(-0.100566815900664,-0.0306434762868126,
-0.934725067745981));
#46758=CARTESIAN_POINT('Ctrl Pts',(-0.0292122176736183,-0.101023526111094,
-0.928397406730112));
#46759=CARTESIAN_POINT('Ctrl Pts',(0.0687704338923482,-0.0795729441733933,
-0.922069745714236));
#46760=CARTESIAN_POINT('Ctrl Pts',(0.10418959696435,0.0142395644734221,
-0.915742084698368));
#46761=CARTESIAN_POINT('Ctrl Pts',(0.0448953814624721,0.0950987446886038,
-0.909414423682493));
#46762=CARTESIAN_POINT('Ctrl Pts',(-0.0552288249674775,0.0894948303592097,
-0.903086762666623));
#46763=CARTESIAN_POINT('Ctrl Pts',(-0.105132247575355,0.00251796785383443,
-0.89675910165075));
#46764=CARTESIAN_POINT('Ctrl Pts',(-0.0594492443673278,-0.086747374951718,
-0.890431440634879));
#46765=CARTESIAN_POINT('Ctrl Pts',(0.0402881120732685,-0.0971400775195495,
-0.884103779619007));
#46766=CARTESIAN_POINT('Ctrl Pts',(0.103393633419944,-0.0192100595457518,
-0.877776118603135));
#46767=CARTESIAN_POINT('Ctrl Pts',(0.0724911862372003,0.0761861436782678,
-0.871448457587262));
#46768=CARTESIAN_POINT('Ctrl Pts',(-0.0243224775810121,0.102311855440078,
-0.86512079657139));
#46769=CARTESIAN_POINT('Ctrl Pts',(-0.0990213559268627,0.0354127419051376,
-0.85879313555552));
#46770=CARTESIAN_POINT('Ctrl Pts',(-0.0836873193538318,-0.0636846026479206,
-0.852465474539646));
#46771=CARTESIAN_POINT('Ctrl Pts',(0.00773758906291201,-0.104878143836567,
-0.846137813523777));
#46772=CARTESIAN_POINT('Ctrl Pts',(0.092127249706139,-0.0507135510699152,
-0.839810152507902));
#46773=CARTESIAN_POINT('Ctrl Pts',(0.0927522585102229,0.0495612113957726,
-0.833482491492031));
#46774=CARTESIAN_POINT('Ctrl Pts',(0.00904432689127528,0.104773542099501,
-0.827154830476159));
#46775=CARTESIAN_POINT('Ctrl Pts',(-0.0828869561536006,0.0647228503792993,
-0.820827169460287));
#46776=CARTESIAN_POINT('Ctrl Pts',(-0.0994551121645673,-0.034175658511552,
-0.814499508444414));
#46777=CARTESIAN_POINT('Ctrl Pts',(-0.025595910469552,-0.102000707380013,
-0.808171847428544));
#46778=CARTESIAN_POINT('Ctrl Pts',(0.0715358053219139,-0.0770838730453207,
-0.801844186412671));
#46779=CARTESIAN_POINT('Ctrl Pts',(0.103625175378567,0.0179197647919879,
-0.795516525396799));
#46780=CARTESIAN_POINT('Ctrl Pts',(0.0414956507199254,0.0966302535859462,
-0.789188864380927));
#46781=CARTESIAN_POINT('Ctrl Pts',(-0.058362874856174,0.0874818253934899,
-0.782861203365056));
#46782=CARTESIAN_POINT('Ctrl Pts',(-0.10515624968344,-0.00120751413291408,
-0.776533542349183));
#46783=CARTESIAN_POINT('Ctrl Pts',(-0.0563386344921838,-0.0887989481945397,
-0.770205881333312));
#46784=CARTESIAN_POINT('Ctrl Pts',(0.0437036357690681,-0.0956519061880418,
-0.763878220317438));
#46785=CARTESIAN_POINT('Ctrl Pts',(0.104009343583256,-0.0155354879075021,
-0.757550559301568));
#46786=CARTESIAN_POINT('Ctrl Pts',(0.0697468603499374,0.0787062285229874,
-0.751222898285696));
#46787=CARTESIAN_POINT('Ctrl Pts',(-0.0279314102255587,0.101386050617451,
-0.744895237269823));
#46788=CARTESIAN_POINT('Ctrl Pts',(-0.100213664949813,0.0318828526697282,
-0.738567576253952));
#46789=CARTESIAN_POINT('Ctrl Pts',(-0.0813788653223073,-0.0666091226174153,
-0.732239915238079));
#46790=CARTESIAN_POINT('Ctrl Pts',(0.0114478644309889,-0.10453822906947,
-0.725912254222208));
#46791=CARTESIAN_POINT('Ctrl Pts',(0.0938658771088217,-0.0474182670666902,
-0.719584593206335));
#46792=CARTESIAN_POINT('Ctrl Pts',(0.0909384208772093,0.052815703586832,
-0.713256932190464));
#46793=CARTESIAN_POINT('Ctrl Pts',(0.00532722044912209,0.105028166028451,
-0.706929271174591));
#46794=CARTESIAN_POINT('Ctrl Pts',(-0.0851276371333977,0.0617460956911325,
-0.70060161015872));
#46795=CARTESIAN_POINT('Ctrl Pts',(-0.0981820768848795,-0.0376772440019834,
-0.694273949142847));
#46796=CARTESIAN_POINT('Ctrl Pts',(-0.0219666387176374,-0.102843384427304,
-0.687946288126977));
#46797=CARTESIAN_POINT('Ctrl Pts',(0.0742214789734623,-0.0745014563347958,
-0.681618627111103));
#46798=CARTESIAN_POINT('Ctrl Pts',(0.102925361485087,0.0215792701493254,
-0.675290966095233));
#46799=CARTESIAN_POINT('Ctrl Pts',(0.0380466396555165,0.098039523397132,
-0.668963305079359));
#46800=CARTESIAN_POINT('Ctrl Pts',(-0.0614251462548661,0.0853595123262889,
-0.662635644063488));
#46801=CARTESIAN_POINT('Ctrl Pts',(-0.105047478972877,-0.00493174395690157,
-0.656307983047617));
#46802=CARTESIAN_POINT('Ctrl Pts',(-0.0531577190451583,-0.0907389213233747,
-0.649980322031743));
#46803=CARTESIAN_POINT('Ctrl Pts',(0.0470645190716644,-0.0940437450422222,
-0.643652661015872));
#46804=CARTESIAN_POINT('Ctrl Pts',(0.104494386063995,-0.0118413773743694,
-0.637325));
#46805=CARTESIAN_POINT('Ctrl Pts',(0.066915047882731,0.08112750029346,-0.630997338984128));
#46806=CARTESIAN_POINT('Ctrl Pts',(-0.0315053149024559,0.100332995918145,
-0.624669677968256));
#46807=CARTESIAN_POINT('Ctrl Pts',(-0.101280168197851,0.0283129381525223,
-0.618342016952384));
#46808=CARTESIAN_POINT('Ctrl Pts',(-0.0789682726947726,-0.0694500312787372,
-0.612014355936513));
#46809=CARTESIAN_POINT('Ctrl Pts',(0.015143775000857,-0.104067098622653,
-0.60568669492064));
#46810=CARTESIAN_POINT('Ctrl Pts',(0.0954866808281567,-0.0440634624313079,
-0.599359033904768));
#46811=CARTESIAN_POINT('Ctrl Pts',(0.0890104378775313,0.0560039006307925,
-0.593031372888897));
#46812=CARTESIAN_POINT('Ctrl Pts',(0.00160342655319863,0.105150957961885,
-0.586703711873024));
#46813=CARTESIAN_POINT('Ctrl Pts',(-0.0872614648363879,0.0586918366693476,
-0.580376050857153));
#46814=CARTESIAN_POINT('Ctrl Pts',(-0.0967858028367096,-0.0411315366387778,
-0.57404838984128));
#46815=CARTESIAN_POINT('Ctrl Pts',(-0.0183097941583832,-0.103556971638278,
-0.56772072882541));
#46816=CARTESIAN_POINT('Ctrl Pts',(0.0768139891555562,-0.0718255247598207,
-0.561393067809536));
#46817=CARTESIAN_POINT('Ctrl Pts',(0.102096354851012,0.0252116890181875,
-0.555065406793666));
#46818=CARTESIAN_POINT('Ctrl Pts',(0.034549872118425,0.0993257331894107,
-0.548737745777792));
#46819=CARTESIAN_POINT('Ctrl Pts',(-0.064410316292193,0.0831300552878031,
-0.542410084761922));
#46820=CARTESIAN_POINT('Ctrl Pts',(-0.104806851798498,-0.00864978341354531,
-0.536082423746048));
#46821=CARTESIAN_POINT('Ctrl Pts',(-0.0499100795856327,-0.0925649982054197,
-0.529754762730178));
#46822=CARTESIAN_POINT('Ctrl Pts',(0.0503663265979779,-0.0923175394063303,
-0.523427101714305));
#46823=CARTESIAN_POINT('Ctrl Pts',(0.104848266324252,-0.00813240344623186,
-0.517099440698433));
#46824=CARTESIAN_POINT('Ctrl Pts',(0.0639992430914645,0.0834469401520101,
-0.51077177968256));
#46825=CARTESIAN_POINT('Ctrl Pts',(-0.0350396738463096,0.0991540024091705,
-0.50444411866669));
#46826=CARTESIAN_POINT('Ctrl Pts',(-0.102219543737853,0.0247074850002744,
-0.498116457650817));
#46827=CARTESIAN_POINT('Ctrl Pts',(-0.0764585584355753,-0.0722037656841195,
-0.491788796634945));
#46828=CARTESIAN_POINT('Ctrl Pts',(0.0188206769785697,-0.103465342289493,
-0.485461135619074));
#46829=CARTESIAN_POINT('Ctrl Pts',(0.096987628872835,-0.040653348971995,
-0.479133474603201));
#46830=CARTESIAN_POINT('Ctrl Pts',(0.0869707282371049,0.0591218011136432,
-0.472805813587329));
#46831=CARTESIAN_POINT('Ctrl Pts',(-0.00212237997704562,0.10514176353974,
-0.466478152571458));
#46832=CARTESIAN_POINT('Ctrl Pts',(-0.0892857612241227,0.0555639071668154,
-0.460150491555585));
#46833=CARTESIAN_POINT('Ctrl Pts',(-0.0952680424451362,-0.0445342006292383,
-0.453822830539714));
#46834=CARTESIAN_POINT('Ctrl Pts',(-0.0146299669934629,-0.104140573278544,
-0.447495169523841));
#46835=CARTESIAN_POINT('Ctrl Pts',(0.0793100817806202,-0.0690594371897487,
-0.441167508507969));
#46836=CARTESIAN_POINT('Ctrl Pts',(0.101139196024548,0.028812461965643,
-0.434839847492098));
#46837=CARTESIAN_POINT('Ctrl Pts',(0.0310097372949585,0.100487268496617,
-0.428512186476226));
#46838=CARTESIAN_POINT('Ctrl Pts',(-0.0673146379656645,0.0807962527136316,
-0.422184525460353));
#46839=CARTESIAN_POINT('Ctrl Pts',(-0.104434670193454,-0.0123569655902224,
-0.415856864444482));
#46840=CARTESIAN_POINT('Ctrl Pts',(-0.0465997925797717,-0.0942748867330842,
-0.409529203428609));
#46841=CARTESIAN_POINT('Ctrl Pts',(0.0536049138929184,-0.0904754560283965,
-0.403201542412738));
#46842=CARTESIAN_POINT('Ctrl Pts',(0.105070540169988,-0.00441322165775816,
-0.396873881396865));
#46843=CARTESIAN_POINT('Ctrl Pts',(0.0610031059188372,0.0856616367183621,
-0.390546220380995));
#46844=CARTESIAN_POINT('Ctrl Pts',(-0.0385300507005929,0.0978505499730241,
-0.384218559365121));
#46845=CARTESIAN_POINT('Ctrl Pts',(-0.103030612457752,0.0210710188076898,
-0.37789089834925));
#46846=CARTESIAN_POINT('Ctrl Pts',(-0.0738528727589387,-0.0748668693232562,
-0.371563237333377));
#46847=CARTESIAN_POINT('Ctrl Pts',(0.022473955086258,-0.102733715399544,
-0.365235576317507));
#46848=CARTESIAN_POINT('Ctrl Pts',(0.0983668372403937,-0.0371922070914784,
-0.358907915301634));
#46849=CARTESIAN_POINT('Ctrl Pts',(0.084821852216415,0.0621654914208049,
-0.352580254285762));
#46850=CARTESIAN_POINT('Ctrl Pts',(-0.00584552247831859,0.105000594302933,
-0.34625259326989));
#46851=CARTESIAN_POINT('Ctrl Pts',(-0.0911979853829655,0.0523662333866202,
-0.339924932254018));
#46852=CARTESIAN_POINT('Ctrl Pts',(-0.0936307008156065,-0.0478809649212701,
-0.333597271238147));
#46853=CARTESIAN_POINT('Ctrl Pts',(-0.0109317761724884,-0.104593456806476,
-0.327269610222274));
#46854=CARTESIAN_POINT('Ctrl Pts',(0.0817066237324652,-0.0662066656406656,
-0.320941949206403));
#46855=CARTESIAN_POINT('Ctrl Pts',(0.100055086439402,0.0323770692715896,
-0.31461428819053));
#46856=CARTESIAN_POINT('Ctrl Pts',(0.0274306787917429,0.101522671349988,
-0.308286627174658));
#46857=CARTESIAN_POINT('Ctrl Pts',(-0.0701344657466005,0.0783610340121442,
-0.301958966158786));
#46858=CARTESIAN_POINT('Ctrl Pts',(-0.103931401323188,-0.0160486372010826,
-0.295631305142914));
#46859=CARTESIAN_POINT('Ctrl Pts',(-0.0432310131273129,-0.0958664406400886,
-0.289303644127042));
#46860=CARTESIAN_POINT('Ctrl Pts',(0.0567762158548203,-0.0885198071067735,
-0.28297598311117));
#46861=CARTESIAN_POINT('Ctrl Pts',(0.105160928601227,-0.00068850035681389,
-0.276648322095299));
#46862=CARTESIAN_POINT('Ctrl Pts',(0.0579303971411072,0.0877688100869956,
-0.270320661079426));
#46863=CARTESIAN_POINT('Ctrl Pts',(-0.0419720643152929,0.0964242747140277,
-0.263993000063555));
#46864=CARTESIAN_POINT('Ctrl Pts',(-0.103712356297359,0.0174081040973306,
-0.257665339047682));
#46865=CARTESIAN_POINT('Ctrl Pts',(-0.0711544863431584,-0.0774359994463466,
-0.251337678031811));
#46866=CARTESIAN_POINT('Ctrl Pts',(0.0260990236988984,-0.10187313629695,
-0.245010017015938));
#46867=CARTESIAN_POINT('Ctrl Pts',(0.0996225747370502,-0.0336843812437931,
-0.238682356000067));
#46868=CARTESIAN_POINT('Ctrl Pts',(0.0825665071024629,0.0651311510869428,
-0.232354694984194));
#46869=CARTESIAN_POINT('Ctrl Pts',(-0.00956132763119429,0.104727627448239,
-0.226027033968323));
#46870=CARTESIAN_POINT('Ctrl Pts',(-0.0929957370733558,0.049102829075485,
-0.219699372952451));
#46871=CARTESIAN_POINT('Ctrl Pts',(-0.0918758331527737,-0.0511676286286223,
-0.213371711936579));
#46872=CARTESIAN_POINT('Ctrl Pts',(-0.00721986369558417,-0.10491505375876,
-0.207044050920707));
#46873=CARTESIAN_POINT('Ctrl Pts',(0.0840006068522954,-0.0632707909353925,
-0.200716389904835));
#46874=CARTESIAN_POINT('Ctrl Pts',(0.0988453868778612,0.0359010366118765,
-0.194388728888963));
#46875=CARTESIAN_POINT('Ctrl Pts',(0.0238171890747536,0.102430642102243,
-0.188061067873091));
#46876=CARTESIAN_POINT('Ctrl Pts',(-0.0728662601675932,0.0758274558920166,
-0.181733406857219));
#46877=CARTESIAN_POINT('Ctrl Pts',(-0.103297676887683,-0.0197201644329452,
-0.175405745841347));
#46878=CARTESIAN_POINT('Ctrl Pts',(-0.0398079697620071,-0.0973376621877754,
-0.169078084825476));
#46879=CARTESIAN_POINT('Ctrl Pts',(0.0598762518653202,-0.0864530474014625,
-0.162750423809603));
#46880=CARTESIAN_POINT('Ctrl Pts',(0.10511931811198,0.00303708518060201,
-0.156422762793732));
#46881=CARTESIAN_POINT('Ctrl Pts',(0.0547849737420719,0.0897658152687806,
-0.150095101777859));
#46882=CARTESIAN_POINT('Ctrl Pts',(-0.0453613944250523,0.0948769669950499,
-0.143767440761988));
#46883=CARTESIAN_POINT('Ctrl Pts',(-0.104263919187185,0.013723338418848,
-0.137439779746115));
#46884=CARTESIAN_POINT('Ctrl Pts',(-0.0683667868681693,-0.079907930935011,
-0.131112118730244));
#46885=CARTESIAN_POINT('Ctrl Pts',(0.0296913338196458,-0.100884685804011,
-0.124784457714371));
#46886=CARTESIAN_POINT('Ctrl Pts',(0.1007532628379,-0.0301342733122123,
-0.1184567966985));
#46887=CARTESIAN_POINT('Ctrl Pts',(0.0802075282097526,0.0680150553744678,
-0.112129135682628));
#46888=CARTESIAN_POINT('Ctrl Pts',(-0.0132651396461531,0.10432320981077,
-0.105801474666756));
#46889=CARTESIAN_POINT('Ctrl Pts',(-0.0946767439621274,0.0457777825103404,
-0.0994738136508837));
#46890=CARTESIAN_POINT('Ctrl Pts',(-0.0900056721113309,-0.0543900511771936,
-0.0931461526350116));
#46891=CARTESIAN_POINT('Ctrl Pts',(-0.00349883201800313,-0.105104989154426,
-0.0868184916191398));
#46892=CARTESIAN_POINT('Ctrl Pts',(0.0861890440424318,-0.0602554437920826,
-0.0804908306032677));
#46893=CARTESIAN_POINT('Ctrl Pts',(0.0975118199824748,0.0393798374633225,
-0.0741631695873958));
#46894=CARTESIAN_POINT('Ctrl Pts',(0.0201734164905109,0.103210236817675,
-0.0678355085715238));
#46895=CARTESIAN_POINT('Ctrl Pts',(-0.0755058576047149,0.0731983272331764,
-0.0615078475556519));
#46896=CARTESIAN_POINT('Ctrl Pts',(-0.102535685748398,-0.0233662345365656,
-0.0551801865397799));
#46897=CARTESIAN_POINT('Ctrl Pts',(-0.036332316246399,-0.0986880403806901,
-0.048852525523908));
#46898=CARTESIAN_POINT('Ctrl Pts',(0.0628961178483592,-0.0842752375943958,
-0.0425248645080358));
#46899=CARTESIAN_POINT('Ctrl Pts',(0.104955270488262,0.00675405203560971,
-0.0361972034921642));
#46900=CARTESIAN_POINT('Ctrl Pts',(0.0515527328771752,0.0916592724290588,
-0.0298695424762917));
#46901=CARTESIAN_POINT('Ctrl Pts',(-0.0486594283428768,0.0931931710624919,
-0.0235418814604202));
#46902=CARTESIAN_POINT('Ctrl Pts',(-0.104750797766374,0.0100550797783035,
-0.017214220444548));
#46903=CARTESIAN_POINT('Ctrl Pts',(-0.0653591496324117,-0.082349657569037,
-0.0108865594286763));
#46904=CARTESIAN_POINT('Ctrl Pts',(0.000161923519070843,-0.0938452514906264,
-0.00666811875142807));
#46905=CARTESIAN_POINT('Ctrl Pts',(0.0281628763286457,-0.0845144524603643,
-0.0045588984128041));
#46906=CARTESIAN_POINT('Ctrl Pts',(0.0868262223680489,0.042511912851507,
-0.949325));
#46907=CARTESIAN_POINT('Ctrl Pts',(0.0727413643237034,0.0712787909934627,
-0.947215779661376));
#46908=CARTESIAN_POINT('Ctrl Pts',(0.0139929319558079,0.113232831299845,
-0.942997338984128));
#46909=CARTESIAN_POINT('Ctrl Pts',(-0.0874824940475139,0.0734063410867091,
-0.936669677968257));
#46910=CARTESIAN_POINT('Ctrl Pts',(-0.109137103018111,-0.0332549081761753,
-0.930342016952384));
#46911=CARTESIAN_POINT('Ctrl Pts',(-0.0317016779449621,-0.109632733995772,
-0.924014355936513));
#46912=CARTESIAN_POINT('Ctrl Pts',(0.0746310386889739,-0.0863541370772251,
-0.91768669492064));
#46913=CARTESIAN_POINT('Ctrl Pts',(0.113068616874035,0.0154530577601656,
-0.91135903390477));
#46914=CARTESIAN_POINT('Ctrl Pts',(0.0487213583111448,0.103203043698082,
-0.905031372888895));
#46915=CARTESIAN_POINT('Ctrl Pts',(-0.0599354161316844,0.0971215647331329,
-0.898703711873025));
#46916=CARTESIAN_POINT('Ctrl Pts',(-0.114091600011384,0.00273254865035857,
-0.892376050857152));
#46917=CARTESIAN_POINT('Ctrl Pts',(-0.0645154989621486,-0.094139971638436,
-0.88604838984128));
#46918=CARTESIAN_POINT('Ctrl Pts',(0.0437214582003731,-0.105418338569157,
-0.879720728825409));
#46919=CARTESIAN_POINT('Ctrl Pts',(0.112204821450399,-0.0208471375856189,
-0.873393067809536));
#46920=CARTESIAN_POINT('Ctrl Pts',(0.0786688729221479,0.0826787140141801,
-0.867065406793666));
#46921=CARTESIAN_POINT('Ctrl Pts',(-0.0263952350250068,0.111030854533241,
-0.860737745777791));
#46922=CARTESIAN_POINT('Ctrl Pts',(-0.107459939205569,0.0384306098074368,
-0.854410084761922));
#46923=CARTESIAN_POINT('Ctrl Pts',(-0.0908191386177551,-0.069111793762257,
-0.848082423746048));
#46924=CARTESIAN_POINT('Ctrl Pts',(0.00839698509998528,-0.113815841594763,
-0.841754762730177));
#46925=CARTESIAN_POINT('Ctrl Pts',(0.0999783184135565,-0.0550353513528612,
-0.835427101714305));
#46926=CARTESIAN_POINT('Ctrl Pts',(0.100656590362684,0.0537848094857212,
-0.829099440698433));
#46927=CARTESIAN_POINT('Ctrl Pts',(0.00981508290605088,0.113702325715277,
-0.822771779682561));
#46928=CARTESIAN_POINT('Ctrl Pts',(-0.0899505686003668,0.0702385207904819,
-0.816444118666689));
#46929=CARTESIAN_POINT('Ctrl Pts',(-0.107930660076814,-0.0370881023753524,
-0.810116457650817));
#46930=CARTESIAN_POINT('Ctrl Pts',(-0.0277771896498851,-0.110693190487889,
-0.803788796634946));
#46931=CARTESIAN_POINT('Ctrl Pts',(0.0776320746061295,-0.083652947726732,
-0.797461135619073));
#46932=CARTESIAN_POINT('Ctrl Pts',(0.112456095375748,0.0194468841302012,
-0.791133474603202));
#46933=CARTESIAN_POINT('Ctrl Pts',(0.0450319030871707,0.104865067525778,
-0.784805813587328));
#46934=CARTESIAN_POINT('Ctrl Pts',(-0.0633365492241791,0.0949370118231875,
-0.778478152571458));
#46935=CARTESIAN_POINT('Ctrl Pts',(-0.114117647575078,-0.00131041828399773,
-0.772150491555585));
#46936=CARTESIAN_POINT('Ctrl Pts',(-0.0611398034372145,-0.0963663796075638,
-0.765822830539714));
#46937=CARTESIAN_POINT('Ctrl Pts',(0.0474280522504172,-0.103803345527359,
-0.759495169523841));
#46938=CARTESIAN_POINT('Ctrl Pts',(0.112873002330155,-0.0168594195710881,
-0.753167508507969));
#46939=CARTESIAN_POINT('Ctrl Pts',(0.0756906760448665,0.0854135600650306,
-0.746839847492098));
#46940=CARTESIAN_POINT('Ctrl Pts',(-0.0303117203018435,0.110026152779519,
-0.740512186476226));
#46941=CARTESIAN_POINT('Ctrl Pts',(-0.108753856602692,0.0345999040057546,
-0.734184525460354));
#46942=CARTESIAN_POINT('Ctrl Pts',(-0.0883139585223654,-0.0722855408311166,
-0.727856864444481));
#46943=CARTESIAN_POINT('Ctrl Pts',(0.0124234495101874,-0.113446959348449,
-0.72152920342861));
#46944=CARTESIAN_POINT('Ctrl Pts',(0.101865111350743,-0.0514592438017468,
-0.715201542412737));
#46945=CARTESIAN_POINT('Ctrl Pts',(0.0986881777920024,0.0573166489533057,
-0.708873881396867));
#46946=CARTESIAN_POINT('Ctrl Pts',(0.00578120527878995,0.113978648652578,
-0.702546220380993));
#46947=CARTESIAN_POINT('Ctrl Pts',(-0.0923822000359727,0.0670080875690203,
-0.696218559365122));
#46948=CARTESIAN_POINT('Ctrl Pts',(-0.106549136944947,-0.0408880923916753,
-0.68989089834925));
#46949=CARTESIAN_POINT('Ctrl Pts',(-0.0238386319703752,-0.111607680331259,
-0.683563237333378));
#46950=CARTESIAN_POINT('Ctrl Pts',(0.0805466209140446,-0.0808504578989677,
-0.677235576317505));
#46951=CARTESIAN_POINT('Ctrl Pts',(0.111696643460103,0.0234182519178975,
-0.670907915301635));
#46952=CARTESIAN_POINT('Ctrl Pts',(0.041288967880603,0.106394435072978,
-0.664580254285761));
#46953=CARTESIAN_POINT('Ctrl Pts',(-0.0666597868758373,0.0926338355937582,
-0.658252593269891));
#46954=CARTESIAN_POINT('Ctrl Pts',(-0.113999607442876,-0.00535202634649346,
-0.651924932254018));
#46955=CARTESIAN_POINT('Ctrl Pts',(-0.0576878109114013,-0.0984716769197821,
-0.645597271238146));
#46956=CARTESIAN_POINT('Ctrl Pts',(0.0510753494621495,-0.102058137159478,
-0.639269610222274));
#46957=CARTESIAN_POINT('Ctrl Pts',(0.11339938004943,-0.0128504975603422,
-0.632941949206402));
#46958=CARTESIAN_POINT('Ctrl Pts',(0.0726175369960301,0.088041172208085,
-0.62661428819053));
#46959=CARTESIAN_POINT('Ctrl Pts',(-0.0341901925335258,0.108883356936053,
-0.620286627174659));
#46960=CARTESIAN_POINT('Ctrl Pts',(-0.109911247077948,0.0307257619745004,
-0.613958966158786));
#46961=CARTESIAN_POINT('Ctrl Pts',(-0.0856979355970119,-0.0753685512501992,
-0.607631305142914));
#46962=CARTESIAN_POINT('Ctrl Pts',(0.0164343249564961,-0.112935679244284,
-0.601303644127043));
#46963=CARTESIAN_POINT('Ctrl Pts',(0.103624039690126,-0.0478185432802246,
-0.594975983111169));
#46964=CARTESIAN_POINT('Ctrl Pts',(0.0965958924057288,0.0607765436125185,
-0.5886483220953));
#46965=CARTESIAN_POINT('Ctrl Pts',(0.00174007029407456,0.114111904893903,
-0.582320661079425));
#46966=CARTESIAN_POINT('Ctrl Pts',(-0.0946978721765143,0.06369354510768,
-0.575993000063556));
#46967=CARTESIAN_POINT('Ctrl Pts',(-0.105033872657499,-0.0446367592653377,
-0.569665339047682));
#46968=CARTESIAN_POINT('Ctrl Pts',(-0.019870151733527,-0.112382079324197,
-0.563337678031811));
#46969=CARTESIAN_POINT('Ctrl Pts',(0.0833600643773254,-0.0779464838857511,
-0.557010017015939));
#46970=CARTESIAN_POINT('Ctrl Pts',(0.110796989020261,0.0273602249111314,
-0.550682356000067));
#46971=CARTESIAN_POINT('Ctrl Pts',(0.0374942064027922,0.10779025544718,
-0.544354694984195));
#46972=CARTESIAN_POINT('Ctrl Pts',(-0.0698993526010974,0.0902143846018526,
-0.538027033968322));
#46973=CARTESIAN_POINT('Ctrl Pts',(-0.113738474061213,-0.00938691649958287,
-0.531699372952451));
#46974=CARTESIAN_POINT('Ctrl Pts',(-0.054163408163978,-0.100453371766237,
-0.525371711936579));
#46975=CARTESIAN_POINT('Ctrl Pts',(0.0546585364698917,-0.100184824569957,
-0.519044050920707));
#46976=CARTESIAN_POINT('Ctrl Pts',(0.113783417925879,-0.00882544549857192,
-0.512716389904835));
#46977=CARTESIAN_POINT('Ctrl Pts',(0.0694532478114199,0.0905582743408296,
-0.506388728888963));
#46978=CARTESIAN_POINT('Ctrl Pts',(-0.0380257489514535,0.107603889798764,
-0.500061067873091));
#46979=CARTESIAN_POINT('Ctrl Pts',(-0.110930676043295,0.0268130527117103,
-0.493733406857219));
#46980=CARTESIAN_POINT('Ctrl Pts',(-0.0829743439112356,-0.07835695843793,
-0.487405745841347));
#46981=CARTESIAN_POINT('Ctrl Pts',(0.0204245719016267,-0.112282641337737,
-0.481078084825475));
#46982=CARTESIAN_POINT('Ctrl Pts',(0.105252898274439,-0.0441178205261098,
-0.474750423809603));
#46983=CARTESIAN_POINT('Ctrl Pts',(0.0943823590531949,0.0641601510495206,
-0.468422762793731));
#46984=CARTESIAN_POINT('Ctrl Pts',(-0.00230324884131971,0.114101926924651,
-0.46209510177786));
#46985=CARTESIAN_POINT('Ctrl Pts',(-0.0968946787615573,0.0602990539796282,
-0.455767440761987));
#46986=CARTESIAN_POINT('Ctrl Pts',(-0.103386768980919,-0.0483293977081192,
-0.449439779746116));
#46987=CARTESIAN_POINT('Ctrl Pts',(-0.0158767303172275,-0.113015415397978,
-0.443112118730243));
#46988=CARTESIAN_POINT('Ctrl Pts',(0.0860688735956011,-0.074944670798716,
-0.436784457714372));
#46989=CARTESIAN_POINT('Ctrl Pts',(0.109758261279774,0.0312678551228649,
-0.4304567966985));
#46990=CARTESIAN_POINT('Ctrl Pts',(0.0336523818857637,0.109050776597685,
-0.424129135682628));
#46991=CARTESIAN_POINT('Ctrl Pts',(-0.0730511800785477,0.0876816957652797,
-0.417801474666755));
#46992=CARTESIAN_POINT('Ctrl Pts',(-0.113334575202457,-0.0134100241171348,
-0.411473813650884));
#46993=CARTESIAN_POINT('Ctrl Pts',(-0.0505710190568692,-0.102308976706315,
-0.405146152635012));
#46994=CARTESIAN_POINT('Ctrl Pts',(0.0581731156287884,-0.0981857591567285,
-0.39881849161914));
#46995=CARTESIAN_POINT('Ctrl Pts',(0.114024633911322,-0.00478931566432666,
-0.392490830603268));
#46996=CARTESIAN_POINT('Ctrl Pts',(0.066201780333436,0.0929617069756521,
-0.386163169587396));
#46997=CARTESIAN_POINT('Ctrl Pts',(-0.0418135751335435,0.106189357365487,
-0.379835508571524));
#46998=CARTESIAN_POINT('Ctrl Pts',(-0.111810863902936,0.0228666874825079,
-0.373507847555652));
#46999=CARTESIAN_POINT('Ctrl Pts',(-0.0801466021399856,-0.0812470113207761,
-0.36718018653978));
#47000=CARTESIAN_POINT('Ctrl Pts',(0.0243891817545069,-0.111488665327419,
-0.360852525523909));
#47001=CARTESIAN_POINT('Ctrl Pts',(0.106749642546848,-0.0403617207173284,
-0.354524864508036));
#47002=CARTESIAN_POINT('Ctrl Pts',(0.0920503561798531,0.0674632241321569,
-0.348197203492164));
#47003=CARTESIAN_POINT('Ctrl Pts',(-0.00634367691964216,0.113948727269254,
-0.341869542476292));
#47004=CARTESIAN_POINT('Ctrl Pts',(-0.0989698623412332,0.0568288749783143,
-0.335541881460421));
#47005=CARTESIAN_POINT('Ctrl Pts',(-0.101609893373419,-0.0519613726895842,
-0.329214220444548));
#47006=CARTESIAN_POINT('Ctrl Pts',(-0.011863380297197,-0.113506893583903,
-0.322886559428676));
#47007=CARTESIAN_POINT('Ctrl Pts',(0.0886696484490485,-0.0718487865385744,
-0.316558898412804));
#47008=CARTESIAN_POINT('Ctrl Pts',(0.108581764058326,0.0351362376632097,
-0.310231237396933));
#47009=CARTESIAN_POINT('Ctrl Pts',(0.0297683166195517,0.110174416307878,
-0.303903576381061));
#47010=CARTESIAN_POINT('Ctrl Pts',(-0.0761113131081678,0.0850389481360976,
-0.297575915365188));
#47011=CARTESIAN_POINT('Ctrl Pts',(-0.112788417843808,-0.0174162993610626,
-0.291248254349317));
#47012=CARTESIAN_POINT('Ctrl Pts',(-0.0469151527867125,-0.104036162569286,
-0.284920593333444));
#47013=CARTESIAN_POINT('Ctrl Pts',(0.0616146754098945,-0.0960634501633001,
-0.278592932317573));
#47014=CARTESIAN_POINT('Ctrl Pts',(0.114122725229451,-0.000747174241290758,
-0.2722652713017));
#47015=CARTESIAN_POINT('Ctrl Pts',(0.0628672158310556,0.0952484533039511,
-0.265937610285829));
#47016=CARTESIAN_POINT('Ctrl Pts',(-0.0455489165689162,0.104641535169077,
-0.259609949269957));
#47017=CARTESIAN_POINT('Ctrl Pts',(-0.112550705837761,0.0188916197972995,
-0.253282288254085));
#47018=CARTESIAN_POINT('Ctrl Pts',(-0.0772182596882115,-0.0840350822803618,
-0.246954627238213));
#47019=CARTESIAN_POINT('Ctrl Pts',(0.0283231781039216,-0.110554747818607,
-0.240626966222341));
#47020=CARTESIAN_POINT('Ctrl Pts',(0.108112393781527,-0.0365549585415569,
-0.234299305206469));
#47021=CARTESIAN_POINT('Ctrl Pts',(0.0896028109350489,0.0706816168156805,
-0.227971644190597));
#47022=CARTESIAN_POINT('Ctrl Pts',(-0.0103761423619725,0.113652498225165,
-0.221643983174725));
#47023=CARTESIAN_POINT('Ctrl Pts',(-0.10092081812797,0.0532873639012817,
-0.215316322158853));
#47024=CARTESIAN_POINT('Ctrl Pts',(-0.0997054761838474,-0.0555281253246631,
-0.208988661142981));
#47025=CARTESIAN_POINT('Ctrl Pts',(-0.00783513926402908,-0.11385589697431,
-0.202661000127109));
#47026=CARTESIAN_POINT('Ctrl Pts',(0.091159124424086,-0.0686627170852657,
-0.196333339111237));
#47027=CARTESIAN_POINT('Ctrl Pts',(0.107268974103842,0.0389605169068645,
-0.190005678095365));
#47028=CARTESIAN_POINT('Ctrl Pts',(0.0258468859173261,0.111159764174754,
-0.183678017079493));
#47029=CARTESIAN_POINT('Ctrl Pts',(-0.0790759105897333,0.082289458915181,
-0.177350356063621));
#47030=CARTESIAN_POINT('Ctrl Pts',(-0.112100687518616,-0.0214007135254068,
-0.171022695047749));
#47031=CARTESIAN_POINT('Ctrl Pts',(-0.043200398242193,-0.10563276136954,
-0.164695034031877));
#47032=CARTESIAN_POINT('Ctrl Pts',(0.0649788959672199,-0.093820561543907,
-0.158367373016006));
#47033=CARTESIAN_POINT('Ctrl Pts',(0.114077568701317,0.00329590506830352,
-0.152039712000133));
#47034=CARTESIAN_POINT('Ctrl Pts',(0.0594537399795861,0.0974156429310687,
-0.145712050984262));
#47035=CARTESIAN_POINT('Ctrl Pts',(-0.0492270848199282,0.102962366146826,
-0.139384389968389));
#47036=CARTESIAN_POINT('Ctrl Pts',(-0.113149272824185,0.0148928390081436,
-0.133056728952518));
#47037=CARTESIAN_POINT('Ctrl Pts',(-0.0741929929333612,-0.0867176713542623,
-0.126729067936645));
#47038=CARTESIAN_POINT('Ctrl Pts',(0.0322216242882799,-0.109482061741097,
-0.120401406920774));
#47039=CARTESIAN_POINT('Ctrl Pts',(0.109339438931944,-0.0327023110098198,
-0.114073745904902));
#47040=CARTESIAN_POINT('Ctrl Pts',(0.0870428002583105,0.0738112869409917,
-0.10774608488903));
#47041=CARTESIAN_POINT('Ctrl Pts',(-0.0143955926131921,0.113213616184728,
-0.101418423873158));
#47042=CARTESIAN_POINT('Ctrl Pts',(-0.102745080140752,0.0496789574277323,
-0.0950907628572858));
#47043=CARTESIAN_POINT('Ctrl Pts',(-0.0976759403333535,-0.0590251621802268,
-0.0887631018414137));
#47044=CARTESIAN_POINT('Ctrl Pts',(-0.00379700189343816,-0.114062018632413,
-0.0824354408255419));
#47045=CARTESIAN_POINT('Ctrl Pts',(0.0935340598630732,-0.0653904025661319,
-0.0761077798096698));
#47046=CARTESIAN_POINT('Ctrl Pts',(0.105821760862179,0.0427357805811043,
-0.0697801187937979));
#47047=CARTESIAN_POINT('Ctrl Pts',(0.0218925916469987,0.112005795820566,
-0.0634524577779259));
#47048=CARTESIAN_POINT('Ctrl Pts',(-0.0819404540759867,0.0794362763547314,
-0.057124796762054));
#47049=CARTESIAN_POINT('Ctrl Pts',(-0.111273759622746,-0.0253575011093263,
-0.050797135746182));
#47050=CARTESIAN_POINT('Ctrl Pts',(-0.0394285501192212,-0.107098218564676,
-0.0444694747303101));
#47051=CARTESIAN_POINT('Ctrl Pts',(0.0682561144208434,-0.0914571591517854,
-0.0381418137144379));
#47052=CARTESIAN_POINT('Ctrl Pts',(0.113899540966728,0.00732963121282598,
-0.0318141526985663));
#47053=CARTESIAN_POINT('Ctrl Pts',(0.0559460480924329,0.0994704601917223,
-0.0254864916826938));
#47054=CARTESIAN_POINT('Ctrl Pts',(-0.0528061766329012,0.101135077408416,
-0.0191588306668223));
#47055=CARTESIAN_POINT('Ctrl Pts',(-0.113677643113911,0.0109119719839194,
-0.0128311696509501));
#47056=CARTESIAN_POINT('Ctrl Pts',(-0.0709290453588032,-0.0893674815208979,
-0.0065035086350784));
#47057=CARTESIAN_POINT('Ctrl Pts',(0.000175722614101231,-0.101842728020838,
-0.00228506795783016));
#47058=CARTESIAN_POINT('Ctrl Pts',(0.0305629119072609,-0.0917167598683523,
-0.000175847619206193));
#47059=CARTESIAN_POINT('Ctrl Pts',(-0.0966824608565994,-8.60709826375376E-5,
-0.0522235916889671));
#47060=CARTESIAN_POINT('Ctrl Pts',(-0.0967482118542818,-0.00730313201218682,
-0.0517481063747054));
#47061=CARTESIAN_POINT('Ctrl Pts',(-0.0960079295412608,-0.0145068569589153,
-0.0512726210604438));
#47062=CARTESIAN_POINT('Ctrl Pts',(-0.094410673781033,-0.0215153244412058,
-0.0507971357461822));
#47063=CARTESIAN_POINT('Ctrl Pts',(-0.0873253564549061,-0.0526044069277746,
-0.0486879154075581));
#47064=CARTESIAN_POINT('Ctrl Pts',(-0.0633769532870638,-0.0798513127462258,
-0.0465786950689341));
#47065=CARTESIAN_POINT('Ctrl Pts',(-0.0334553076131315,-0.0908679224199693,
-0.0444694747303101));
#47066=CARTESIAN_POINT('Ctrl Pts',(-0.00353366193920001,-0.101884532093712,
-0.0423602543916861));
#47067=CARTESIAN_POINT('Ctrl Pts',(0.0323612262408212,-0.096670845622749,
-0.040251034053062));
#47068=CARTESIAN_POINT('Ctrl Pts',(0.0579159080884793,-0.077599537326499,
-0.0381418137144381));
#47069=CARTESIAN_POINT('Ctrl Pts',(0.0834705899361389,-0.058528229030248,
-0.036032593375814));
#47070=CARTESIAN_POINT('Ctrl Pts',(0.0986850654514341,-0.0255992989087089,
-0.03392337303719));
#47071=CARTESIAN_POINT('Ctrl Pts',(0.0966333877300311,0.00622197098187709,
-0.0318141526985659));
#47072=CARTESIAN_POINT('Ctrl Pts',(0.0945817100086281,0.0380432408724604,
-0.029704932359942));
#47073=CARTESIAN_POINT('Ctrl Pts',(0.0752638790505303,0.0687568505320909,
-0.0275957120213179));
#47074=CARTESIAN_POINT('Ctrl Pts',(0.0474795927839263,0.0843910915646887,
-0.025486491682694));
#47075=CARTESIAN_POINT('Ctrl Pts',(0.0196953065173216,0.100025332597287,
-0.02337727134407));
#47076=CARTESIAN_POINT('Ctrl Pts',(-0.0165554350577898,0.100580205002852,
-0.0212680510054461));
#47077=CARTESIAN_POINT('Ctrl Pts',(-0.0448260502588471,0.0858204569682178,
-0.0191588306668222));
#47078=CARTESIAN_POINT('Ctrl Pts',(-0.0708903387085866,0.0722126055831592,
-0.0172142204445482));
#47079=CARTESIAN_POINT('Ctrl Pts',(-0.090171483783908,0.0455872578200469,
-0.015269610222274));
#47080=CARTESIAN_POINT('Ctrl Pts',(-0.0953893049619544,0.016632511936229,
-0.013325));
#47081=CARTESIAN_POINT('',(-0.060188439738649,0.0430776079607707,-0.949325000000001));
#47082=CARTESIAN_POINT('Ctrl Pts',(-0.060189526236291,0.0430788597277722,
-0.949325000000001));
#47083=CARTESIAN_POINT('Ctrl Pts',(-0.0593167659583275,0.0448108322152602,
-0.949325000000001));
#47084=CARTESIAN_POINT('Ctrl Pts',(-0.058373221122004,0.0465024987601996,
-0.949325000000001));
#47085=CARTESIAN_POINT('Ctrl Pts',(-0.0573600015023254,0.0481490225008083,
-0.949325000000001));
#47086=CARTESIAN_POINT('Ctrl Pts',(-0.0550289716257877,0.0519370423508429,
-0.949325000000001));
#47087=CARTESIAN_POINT('Ctrl Pts',(-0.0523302084036976,0.0554864887030456,
-0.949325000000001));
#47088=CARTESIAN_POINT('Ctrl Pts',(-0.0493207856021755,0.058781745439232,
-0.949325000000001));
#47089=CARTESIAN_POINT('Ctrl Pts',(-0.047250923751369,0.0610482020512428,
-0.949325000000001));
#47090=CARTESIAN_POINT('Ctrl Pts',(-0.0450386139126382,0.0631885855487683,
-0.949325000000001));
#47091=CARTESIAN_POINT('Ctrl Pts',(-0.0427077511546215,0.0651933292177597,
-0.949325));
#47092=CARTESIAN_POINT('Ctrl Pts',(-0.0397757434975351,0.0677151095189643,
-0.949325));
#47093=CARTESIAN_POINT('Ctrl Pts',(-0.0366539499723158,0.0700249987493579,
-0.949325));
#47094=CARTESIAN_POINT('Ctrl Pts',(-0.0333746515884088,0.0721117425950514,
-0.949325));
#47095=CARTESIAN_POINT('Ctrl Pts',(-0.0311123386830825,0.0735513394171613,
-0.949325));
#47096=CARTESIAN_POINT('Ctrl Pts',(-0.0287792691540412,0.0748815931761674,
-0.949325));
#47097=CARTESIAN_POINT('Ctrl Pts',(-0.0263934417288112,0.076095782333911,
-0.949325));
#47098=CARTESIAN_POINT('Ctrl Pts',(-0.0203682371240397,0.0791621139666756,
-0.949325));
#47099=CARTESIAN_POINT('Ctrl Pts',(-0.0139965057979827,0.0814990538506737,
-0.949325));
#47100=CARTESIAN_POINT('Ctrl Pts',(-0.00743271588570414,0.0830440140828357,
-0.949325));
#47101=CARTESIAN_POINT('Ctrl Pts',(-0.00427118281189676,0.0837881638708354,
-0.949325));
#47102=CARTESIAN_POINT('Ctrl Pts',(-0.00106024802673121,0.0843478681521641,
-0.949325));
#47103=CARTESIAN_POINT('Ctrl Pts',(0.00215611887931482,0.0847110161631254,
-0.949325));
#47104=CARTESIAN_POINT('Ctrl Pts',(0.00491111070927283,0.0850220720322127,
-0.949325));
#47105=CARTESIAN_POINT('Ctrl Pts',(0.00767363596591655,0.0851900857508143,
-0.949325));
#47106=CARTESIAN_POINT('Ctrl Pts',(0.0104334171757828,0.0852111838068372,
-0.949325));
#47107=CARTESIAN_POINT('Ctrl Pts',(0.0156467829036102,0.085251039097467,
-0.949325));
#47108=CARTESIAN_POINT('Ctrl Pts',(0.0208502407431678,0.0847678597630326,
-0.949325));
#47109=CARTESIAN_POINT('Ctrl Pts',(0.0259925480469261,0.0838058103808331,
-0.949325));
#47110=CARTESIAN_POINT('Ctrl Pts',(0.0290438237261958,0.0832349619836522,
-0.949325));
#47111=CARTESIAN_POINT('Ctrl Pts',(0.0320762587705588,0.0824937705719952,
-0.949325));
#47112=CARTESIAN_POINT('Ctrl Pts',(0.0350558312760954,0.0815973397057138,
-0.949325));
#47113=CARTESIAN_POINT('Ctrl Pts',(0.040320890222968,0.0800132999335661,
-0.949325));
#47114=CARTESIAN_POINT('Ctrl Pts',(0.0454359562981305,0.077943784060909,
-0.949325));
#47115=CARTESIAN_POINT('Ctrl Pts',(0.0503444084903423,0.0754381748870302,
-0.949325));
#47116=CARTESIAN_POINT('Ctrl Pts',(0.0539991272551031,0.0735725568660456,
-0.949325));
#47117=CARTESIAN_POINT('Ctrl Pts',(0.0575394528428315,0.0714647391106675,
-0.949325));
#47118=CARTESIAN_POINT('Ctrl Pts',(0.0609412351239781,0.0691287510149368,
-0.949325));
#47119=CARTESIAN_POINT('Ctrl Pts',(0.0632536174634446,0.067540848800351,
-0.949325));
#47120=CARTESIAN_POINT('Ctrl Pts',(0.0654949036874784,0.065852008116864,
-0.949325));
#47121=CARTESIAN_POINT('Ctrl Pts',(0.0676532889369962,0.0640719733065252,
-0.949325));
#47122=CARTESIAN_POINT('Ctrl Pts',(0.0734442214483512,0.0592961523742621,
-0.949325));
#47123=CARTESIAN_POINT('Ctrl Pts',(0.0786514181655312,0.053859434543402,
-0.949325));
#47124=CARTESIAN_POINT('Ctrl Pts',(0.0831347399305807,0.0478498241354048,
-0.949325));
#47125=CARTESIAN_POINT('Ctrl Pts',(0.0844267955137165,0.0461179050167157,
-0.949325));
#47126=CARTESIAN_POINT('Ctrl Pts',(0.0856585743201443,0.0443381162764104,
-0.949325));
#47127=CARTESIAN_POINT('Ctrl Pts',(0.0868262223680485,0.0425119128515078,
-0.949325));
#47128=CARTESIAN_POINT('Ctrl Pts',(-0.0601895262362904,0.043078859727773,
-0.949325000000001));
#47129=CARTESIAN_POINT('Ctrl Pts',(-0.0689869256062287,0.0306389221630466,
-0.948007581356588));
#47130=CARTESIAN_POINT('Ctrl Pts',(-0.0737422450059072,0.0152538149691926,
-0.946690162713175));
#47131=CARTESIAN_POINT('Ctrl Pts',(-0.0738572813634733,-6.14771210490517E-5,
-0.945372744069761));
#47132=CARTESIAN_POINT('Origin',(-2.39206768658147E-17,-5.43753587379397E-18,
-0.949325));
#47133=CARTESIAN_POINT('Ctrl Pts',(0.0869479092309518,-0.0426124462865232,
-0.949325));
#47134=CARTESIAN_POINT('Ctrl Pts',(0.0856124747599027,-0.044722461608285,
-0.949325));
#47135=CARTESIAN_POINT('Ctrl Pts',(0.0841919414744527,-0.0467735581943342,
-0.949325));
#47136=CARTESIAN_POINT('Ctrl Pts',(0.0826860413332504,-0.0487597210798102,
-0.949325));
#47137=CARTESIAN_POINT('Ctrl Pts',(0.0795662948336701,-0.0528744193523085,
-0.949325));
#47138=CARTESIAN_POINT('Ctrl Pts',(0.0760804375487611,-0.0567111004573341,
-0.949325));
#47139=CARTESIAN_POINT('Ctrl Pts',(0.0722794809423723,-0.0602429512049958,
-0.949325));
#47140=CARTESIAN_POINT('Ctrl Pts',(0.0700290204710016,-0.0623340801815892,
-0.949325));
#47141=CARTESIAN_POINT('Ctrl Pts',(0.0676685942007772,-0.0643170596610832,
-0.949325));
#47142=CARTESIAN_POINT('Ctrl Pts',(0.0652188324310721,-0.0661784227849254,
-0.949325));
#47143=CARTESIAN_POINT('Ctrl Pts',(0.0606222177764784,-0.0696709946416588,
-0.949325));
#47144=CARTESIAN_POINT('Ctrl Pts',(0.0557025495139305,-0.0727449380364621,
-0.949325));
#47145=CARTESIAN_POINT('Ctrl Pts',(0.0505311108350954,-0.0753559521252754,
-0.949325));
#47146=CARTESIAN_POINT('Ctrl Pts',(0.0478794628880133,-0.0766947459461787,
-0.949325));
#47147=CARTESIAN_POINT('Ctrl Pts',(0.0451679051661795,-0.0779080793618369,
-0.949325));
#47148=CARTESIAN_POINT('Ctrl Pts',(0.0424135767913811,-0.0789879073549741,
-0.949325));
#47149=CARTESIAN_POINT('Ctrl Pts',(0.0359064717582129,-0.0815390026540642,
-0.949325));
#47150=CARTESIAN_POINT('Ctrl Pts',(0.0291478261251087,-0.0833546720972159,
-0.949325));
#47151=CARTESIAN_POINT('Ctrl Pts',(0.0222695016912951,-0.0843425229564047,
-0.949325));
#47152=CARTESIAN_POINT('Ctrl Pts',(0.0187466195598109,-0.0848484720685605,
-0.949325));
#47153=CARTESIAN_POINT('Ctrl Pts',(0.0151868435066227,-0.0851359066764804,
-0.949325));
#47154=CARTESIAN_POINT('Ctrl Pts',(0.0116411143525298,-0.0851885509642709,
-0.949325));
#47155=CARTESIAN_POINT('Ctrl Pts',(0.00899012535258925,-0.0852279108312482,
-0.949325));
#47156=CARTESIAN_POINT('Ctrl Pts',(0.00634411118670679,-0.0851367815144602,
-0.949325));
#47157=CARTESIAN_POINT('Ctrl Pts',(0.00371070448365139,-0.0849098407765668,
-0.949325));
#47158=CARTESIAN_POINT('Ctrl Pts',(-0.00105029165046096,-0.0844995494324574,
-0.949325));
#47159=CARTESIAN_POINT('Ctrl Pts',(-0.00577057451462265,-0.0836458514358007,
-0.949325));
#47160=CARTESIAN_POINT('Ctrl Pts',(-0.0104000956501732,-0.0823745810341941,
-0.949325));
#47161=CARTESIAN_POINT('Ctrl Pts',(-0.0136088438978973,-0.0814934560637918,
-0.949325));
#47162=CARTESIAN_POINT('Ctrl Pts',(-0.0167781026383413,-0.0804091054703374,
-0.949325));
#47163=CARTESIAN_POINT('Ctrl Pts',(-0.0198623067016642,-0.0791405298678325,
-0.949325));
#47164=CARTESIAN_POINT('Ctrl Pts',(-0.0241228446148006,-0.0773881119541069,
-0.949325));
#47165=CARTESIAN_POINT('Ctrl Pts',(-0.0282314604779494,-0.0752828969338322,
-0.949325));
#47166=CARTESIAN_POINT('Ctrl Pts',(-0.0321421958340599,-0.0728495357347055,
-0.949325));
#47167=CARTESIAN_POINT('Ctrl Pts',(-0.0349610431368854,-0.0710955756662388,
-0.949325));
#47168=CARTESIAN_POINT('Ctrl Pts',(-0.0376769507073806,-0.0691709018220058,
-0.949325));
#47169=CARTESIAN_POINT('Ctrl Pts',(-0.0402692415138934,-0.0670826356986748,
-0.949325));
#47170=CARTESIAN_POINT('Ctrl Pts',(-0.0421087437862932,-0.0656007918138791,
-0.949325));
#47171=CARTESIAN_POINT('Ctrl Pts',(-0.0438851409941927,-0.0640366886918159,
-0.949325));
#47172=CARTESIAN_POINT('Ctrl Pts',(-0.0455816439518849,-0.062402390001981,
-0.949325));
#47173=CARTESIAN_POINT('Ctrl Pts',(-0.0499864700882501,-0.0581590719747581,
-0.949325));
#47174=CARTESIAN_POINT('Ctrl Pts',(-0.0538751594869068,-0.0534289751223524,
-0.949325));
#47175=CARTESIAN_POINT('Ctrl Pts',(-0.0571141568373989,-0.0482621911224861,
-0.949325));
#47176=CARTESIAN_POINT('Ctrl Pts',(-0.0581865816518023,-0.0465514804387378,
-0.949325));
#47177=CARTESIAN_POINT('Ctrl Pts',(-0.0591873861521787,-0.0447927885495833,
-0.949325));
#47178=CARTESIAN_POINT('Ctrl Pts',(-0.0601104350279403,-0.0429877377952337,
-0.949325));
#47179=CARTESIAN_POINT('Origin',(0.,0.,-0.949325));
#47180=CARTESIAN_POINT('Origin',(0.,0.,-1.05327725593024));
#47181=CARTESIAN_POINT('Ctrl Pts',(-0.0786356739692304,-0.0562359885162954,
-0.962474152380794));
#47182=CARTESIAN_POINT('Ctrl Pts',(-0.0600038161649918,-0.0822892105612963,
-0.96036493204217));
#47183=CARTESIAN_POINT('Ctrl Pts',(0.004853946138599,-0.113990840317091,
-0.956146491364922));
#47184=CARTESIAN_POINT('Ctrl Pts',(0.0983810235117565,-0.0579900836424825,
-0.949818830349049));
#47185=CARTESIAN_POINT('Ctrl Pts',(0.10216681566528,0.0507813110782263,
-0.943491169333179));
#47186=CARTESIAN_POINT('Ctrl Pts',(0.0132059581691852,0.113357553994674,
-0.937163508317305));
#47187=CARTESIAN_POINT('Ctrl Pts',(-0.0878384118263931,0.0728782692965182,
-0.930835847301434));
#47188=CARTESIAN_POINT('Ctrl Pts',(-0.10897753085853,-0.0338704598317053,
-0.924508186285562));
#47189=CARTESIAN_POINT('Ctrl Pts',(-0.0310523850839464,-0.109819800841145,
-0.918180525269691));
#47190=CARTESIAN_POINT('Ctrl Pts',(0.075117597679381,-0.0859197258996397,
-0.911852864253818));
#47191=CARTESIAN_POINT('Ctrl Pts',(0.112982694264295,0.0161019074255883,
-0.905525203237947));
#47192=CARTESIAN_POINT('Ctrl Pts',(0.0481238767758512,0.103482736629349,
-0.899197542222073));
#47193=CARTESIAN_POINT('Ctrl Pts',(-0.0604921422302409,0.0967744449238958,
-0.892869881206203));
#47194=CARTESIAN_POINT('Ctrl Pts',(-0.114106160426482,0.00207599406145328,
-0.88654222019033));
#47195=CARTESIAN_POINT('Ctrl Pts',(-0.0639721344284186,-0.094509934905488,
-0.880214559174458));
#47196=CARTESIAN_POINT('Ctrl Pts',(0.0443273765905862,-0.105164838429805,
-0.873886898158588));
#47197=CARTESIAN_POINT('Ctrl Pts',(0.112323076495157,-0.0202009223948133,
-0.867559237142713));
#47198=CARTESIAN_POINT('Ctrl Pts',(0.0781915744196983,0.0831302239521522,
-0.861231576126844));
#47199=CARTESIAN_POINT('Ctrl Pts',(-0.0270339192117008,0.110877061822789,
-0.85490391511097));
#47200=CARTESIAN_POINT('Ctrl Pts',(-0.107679402325512,0.0378113850182401,
-0.848576254095099));
#47201=CARTESIAN_POINT('Ctrl Pts',(-0.0904197845472554,-0.0696334542227982,
-0.842248593079227));
#47202=CARTESIAN_POINT('Ctrl Pts',(0.00905202397369058,-0.113765618960802,
-0.835920932063354));
#47203=CARTESIAN_POINT('Ctrl Pts',(0.100293477560122,-0.0544589150043569,
-0.829593271047484));
#47204=CARTESIAN_POINT('Ctrl Pts',(0.100345310375543,0.0543633505043467,
-0.823265610031609));
#47205=CARTESIAN_POINT('Ctrl Pts',(0.00916039240033352,0.113756944255607,
-0.81693794901574));
#47206=CARTESIAN_POINT('Ctrl Pts',(-0.090353408994793,0.06971955697025,
-0.810610287999865));
#47207=CARTESIAN_POINT('Ctrl Pts',(-0.107715375494224,-0.0377087926315068,
-0.804282626983996));
#47208=CARTESIAN_POINT('Ctrl Pts',(-0.0271395234400288,-0.110851258090984,
-0.797954965968122));
#47209=CARTESIAN_POINT('Ctrl Pts',(0.0781123388944825,-0.0832046733305623,
-0.791627304952251));
#47210=CARTESIAN_POINT('Ctrl Pts',(0.112342287909493,0.0200939170266501,
-0.785299643936378));
#47211=CARTESIAN_POINT('Ctrl Pts',(0.0444275008731675,0.105122558564952,
-0.778971982920508));
#47212=CARTESIAN_POINT('Ctrl Pts',(-0.0638820069123982,0.0945708430006401,
-0.772644321904634));
#47213=CARTESIAN_POINT('Ctrl Pts',(-0.114108215395601,-0.00196731608905759,
-0.766316660888764));
#47214=CARTESIAN_POINT('Ctrl Pts',(-0.0605840574034091,-0.0967167366163604,
-0.759988999872891));
#47215=CARTESIAN_POINT('Ctrl Pts',(0.0480248123783114,-0.103528607395316,
-0.753661338857019));
#47216=CARTESIAN_POINT('Ctrl Pts',(0.11296818562502,-0.0162093858558479,
-0.747333677841147));
#47217=CARTESIAN_POINT('Ctrl Pts',(0.0751977392068195,0.0858478606104231,
-0.741006016825276));
#47218=CARTESIAN_POINT('Ctrl Pts',(-0.0309445853761717,0.109849842007643,
-0.734678355809402));
#47219=CARTESIAN_POINT('Ctrl Pts',(-0.108951231366766,0.0339732885790987,
-0.728350694793533));
#47220=CARTESIAN_POINT('Ctrl Pts',(-0.0878963843456035,-0.0727927247201165,
-0.722023033777658));
#47221=CARTESIAN_POINT('Ctrl Pts',(0.0130763025601953,-0.113373565986802,
-0.715695372761788));
#47222=CARTESIAN_POINT('Ctrl Pts',(0.10215965110392,-0.0508720044772741,
-0.709367711745915));
#47223=CARTESIAN_POINT('Ctrl Pts',(0.0983566005041366,0.0578837998966845,
-0.703040050730044));
#47224=CARTESIAN_POINT('Ctrl Pts',(0.00512499025186194,0.114010041786363,
-0.696712389714171));
#47225=CARTESIAN_POINT('Ctrl Pts',(-0.0927664038289317,0.0664751793819131,
-0.6903847286983));
#47226=CARTESIAN_POINT('Ctrl Pts',(-0.106312000718267,-0.0415007669385643,
-0.684057067682427));
#47227=CARTESIAN_POINT('Ctrl Pts',(-0.0231957665837685,-0.11174306048163,
-0.677729406666556));
#47228=CARTESIAN_POINT('Ctrl Pts',(0.0810107043522212,-0.0803854522508077,
-0.671401745650683));
#47229=CARTESIAN_POINT('Ctrl Pts',(0.111559987366709,0.0240608472824536,
-0.665074084634812));
#47230=CARTESIAN_POINT('Ctrl Pts',(0.0406758237805722,0.106630354557141,
-0.658746423618939));
#47231=CARTESIAN_POINT('Ctrl Pts',(-0.067191931295414,0.0922485746339869,
-0.652418762603068));
#47232=CARTESIAN_POINT('Ctrl Pts',(-0.113966911659595,-0.00600817775902438,
-0.646091101587196));
#47233=CARTESIAN_POINT('Ctrl Pts',(-0.0571200028417465,-0.0988021276520335,
-0.639763440571324));
#47234=CARTESIAN_POINT('Ctrl Pts',(0.0516620029121628,-0.101762432205179,
-0.633435779555452));
#47235=CARTESIAN_POINT('Ctrl Pts',(0.113471477229269,-0.0121975000970476,
-0.62710811853958));
#47236=CARTESIAN_POINT('Ctrl Pts',(0.0721095251424329,0.088457738705795,
-0.620780457523708));
#47237=CARTESIAN_POINT('Ctrl Pts',(-0.0348164148990489,0.10868473861029,
-0.614452796507836));
#47238=CARTESIAN_POINT('Ctrl Pts',(-0.110086301145192,0.0300925481370394,
-0.608125135491964));
#47239=CARTESIAN_POINT('Ctrl Pts',(-0.0852626573341289,-0.0758606249482087,
-0.601797474476093));
#47240=CARTESIAN_POINT('Ctrl Pts',(0.0170841684337436,-0.112839205696147,
-0.59546981346022));
#47241=CARTESIAN_POINT('Ctrl Pts',(0.103897592599086,-0.0472212389219527,
-0.589142152444348));
#47242=CARTESIAN_POINT('Ctrl Pts',(0.0962444328252329,0.0613315930280561,
-0.582814491428477));
#47243=CARTESIAN_POINT('Ctrl Pts',(0.00108315506015306,0.114120032984247,
-0.576486830412604));
#47244=CARTESIAN_POINT('Ctrl Pts',(-0.0950629574431477,0.0631473615867847,
-0.570159169396732));
#47245=CARTESIAN_POINT('Ctrl Pts',(-0.104775182267608,-0.0452406491332671,
-0.563831508380861));
#47246=CARTESIAN_POINT('Ctrl Pts',(-0.0192228941921356,-0.112494602057556,
-0.557503847364987));
#47247=CARTESIAN_POINT('Ctrl Pts',(0.0838073844924436,-0.0774653306824775,
-0.551176186349117));
#47248=CARTESIAN_POINT('Ctrl Pts',(0.110637655806019,0.0279975761622086,
-0.544848525333244));
#47249=CARTESIAN_POINT('Ctrl Pts',(0.0368730900537828,0.108004307243255,
-0.538520864317373));
#47250=CARTESIAN_POINT('Ctrl Pts',(-0.070417515807047,0.0898105150902397,
-0.5321932033015));
#47251=CARTESIAN_POINT('Ctrl Pts',(-0.113682555710397,-0.0100414979142685,
-0.525865542285629));
#47252=CARTESIAN_POINT('Ctrl Pts',(-0.0535842507778536,-0.100763501436711,
-0.519537881269756));
#47253=CARTESIAN_POINT('Ctrl Pts',(0.055234346870785,-0.0998685239650997,
-0.513210220253885));
#47254=CARTESIAN_POINT('Ctrl Pts',(0.113832338493163,-0.00817030393485694,
-0.506882559238013));
#47255=CARTESIAN_POINT('Ctrl Pts',(0.0689307986032583,0.0909565839130236,
-0.50055489822214));
#47256=CARTESIAN_POINT('Ctrl Pts',(-0.0386445425688116,0.107383213226543,
-0.494227237206269));
#47257=CARTESIAN_POINT('Ctrl Pts',(-0.111083189684309,0.0261740352786816,
-0.487899576190397));
#47258=CARTESIAN_POINT('Ctrl Pts',(-0.0825219079271646,-0.078833304289941,
-0.481571915174525));
#47259=CARTESIAN_POINT('Ctrl Pts',(0.0210705901172056,-0.112163208697516,
-0.475244254158653));
#47260=CARTESIAN_POINT('Ctrl Pts',(0.105505120973288,-0.0435112008754263,
-0.468916593142781));
#47261=CARTESIAN_POINT('Ctrl Pts',(0.09401145833506,0.064702402234578,-0.46258893212691));
#47262=CARTESIAN_POINT('Ctrl Pts',(-0.00296003971678002,0.114086779769108,
-0.456261271111036));
#47263=CARTESIAN_POINT('Ctrl Pts',(-0.0972401872438056,0.0597402806990355,
-0.449933610095166));
#47264=CARTESIAN_POINT('Ctrl Pts',(-0.103106849138143,-0.0489237448895124,
-0.443605949079292));
#47265=CARTESIAN_POINT('Ctrl Pts',(-0.0152258930640914,-0.113104939474856,
-0.437278288063422));
#47266=CARTESIAN_POINT('Ctrl Pts',(0.0864988689077382,-0.0744479739878243,
-0.430950627047549));
#47267=CARTESIAN_POINT('Ctrl Pts',(0.109576450941058,0.0318991622518809,
-0.424622966031678));
#47268=CARTESIAN_POINT('Ctrl Pts',(0.0330240729181738,0.10924269202608,
-0.418295305015805));
#47269=CARTESIAN_POINT('Ctrl Pts',(-0.0735547116681115,0.0872597246421901,
-0.411967643999934));
#47270=CARTESIAN_POINT('Ctrl Pts',(-0.113255504473285,-0.0140622138979488,
-0.405639982984062));
#47271=CARTESIAN_POINT('Ctrl Pts',(-0.0499812393174355,-0.102598396037673,
-0.399312321968189));
#47272=CARTESIAN_POINT('Ctrl Pts',(0.0587373602185643,-0.0978492599244596,
-0.392984660952318));
#47273=CARTESIAN_POINT('Ctrl Pts',(0.114050316460549,-0.00413285233932352,
-0.386656999936446));
#47274=CARTESIAN_POINT('Ctrl Pts',(0.0656655495532949,0.093341259660847,
-0.380329338920574));
#47275=CARTESIAN_POINT('Ctrl Pts',(-0.0424241632878486,0.105946899541873,
-0.374001677904702));
#47276=CARTESIAN_POINT('Ctrl Pts',(-0.111940645681331,0.0222226685538999,
-0.36767401688883));
#47277=CARTESIAN_POINT('Ctrl Pts',(-0.0796775763361311,-0.0817070314135196,
-0.361346355872957));
#47278=CARTESIAN_POINT('Ctrl Pts',(0.0250305638209899,-0.111346423507957,
-0.355018694857086));
#47279=CARTESIAN_POINT('Ctrl Pts',(0.10698021844356,-0.0397465472082552,
-0.348691033841214));
#47280=CARTESIAN_POINT('Ctrl Pts',(0.0916604798817394,0.0679919964485462,
-0.342363372825342));
#47281=CARTESIAN_POINT('Ctrl Pts',(-0.00699951902728272,0.113910323880659,
-0.33603571180947));
#47282=CARTESIAN_POINT('Ctrl Pts',(-0.09929536035398,0.0562582133148854,
-0.329708050793598));
#47283=CARTESIAN_POINT('Ctrl Pts',(-0.10130909543547,-0.0525454311549234,
-0.323380389777726));
#47284=CARTESIAN_POINT('Ctrl Pts',(-0.0112097802686418,-0.113573306632935,
-0.317052728761854));
#47285=CARTESIAN_POINT('Ctrl Pts',(0.0890817792245178,-0.0713371695780267,
-0.310725067745982));
#47286=CARTESIAN_POINT('Ctrl Pts',(0.108377704804983,0.035760708248213,
-0.30439740673011));
#47287=CARTESIAN_POINT('Ctrl Pts',(0.0291336036920155,0.110343954474753,
-0.298069745714238));
#47288=CARTESIAN_POINT('Ctrl Pts',(-0.0765995810443127,0.0845994050631894,
-0.291742084698366));
#47289=CARTESIAN_POINT('Ctrl Pts',(-0.112686293986516,-0.0180652788739757,
-0.285414423682494));
#47290=CARTESIAN_POINT('Ctrl Pts',(-0.0463154909903957,-0.10430450827998,
-0.279086762666623));
#47291=CARTESIAN_POINT('Ctrl Pts',(0.0621666459440579,-0.0957071746802496,
-0.27275910165075));
#47292=CARTESIAN_POINT('Ctrl Pts',(0.114125137523673,-9.02131532161566E-5,
-0.266431440634879));
#47293=CARTESIAN_POINT('Ctrl Pts',(0.06231787656026,0.095608772684466,-0.260103779619006));
#47294=CARTESIAN_POINT('Ctrl Pts',(-0.0461505328448423,0.104377600429143,
-0.253776118603135));
#47295=CARTESIAN_POINT('Ctrl Pts',(-0.112657592850385,0.0182434077510212,
-0.247448457587262));
#47296=CARTESIAN_POINT('Ctrl Pts',(-0.0767332327896328,-0.0844781991928046,
-0.241120796571391));
#47297=CARTESIAN_POINT('Ctrl Pts',(0.0289591189531694,-0.110389875363005,
-0.234793135555518));
#47298=CARTESIAN_POINT('Ctrl Pts',(0.108321033455404,-0.0359320033450135,
-0.228465474539647));
#47299=CARTESIAN_POINT('Ctrl Pts',(0.0891944484327669,0.0711962465440421,
-0.222137813523774));
#47300=CARTESIAN_POINT('Ctrl Pts',(-0.0110302124830365,0.113590886807688,
-0.215810152507903));
#47301=CARTESIAN_POINT('Ctrl Pts',(-0.101225897103969,0.0527055301544334,
-0.209482491492031));
#47302=CARTESIAN_POINT('Ctrl Pts',(-0.099384177713727,-0.0561011619592128,
-0.203154830476159));
#47303=CARTESIAN_POINT('Ctrl Pts',(-0.00717959686625945,-0.113899115632717,
-0.196827169460287));
#47304=CARTESIAN_POINT('Ctrl Pts',(0.0915528733567521,-0.0681368221619972,
-0.190499508444415));
#47305=CARTESIAN_POINT('Ctrl Pts',(0.107042922065464,0.0395773671092362,
-0.184171847428543));
#47306=CARTESIAN_POINT('Ctrl Pts',(0.025206565740586,0.111306712270516,
-0.177844186412671));
#47307=CARTESIAN_POINT('Ctrl Pts',(-0.0795483020206782,0.0818328956179269,
-0.171516525396799));
#47308=CARTESIAN_POINT('Ctrl Pts',(-0.111975638670248,-0.0220456681799031,
-0.165188864380927));
#47309=CARTESIAN_POINT('Ctrl Pts',(-0.0425916071836757,-0.105879696603329,
-0.158861203365055));
#47310=CARTESIAN_POINT('Ctrl Pts',(0.0655178997864847,-0.0934449570602429,
-0.152533542349183));
#47311=CARTESIAN_POINT('Ctrl Pts',(0.11405670737362,0.00395253939170301,
-0.146205881333311));
#47312=CARTESIAN_POINT('Ctrl Pts',(0.0588919823963425,0.0977562765503247,
-0.139878220317439));
#47313=CARTESIAN_POINT('Ctrl Pts',(-0.0498189752833788,0.10267728612641,
-0.133550559301567));
#47314=CARTESIAN_POINT('Ctrl Pts',(-0.113233128592107,0.0142412468351748,
-0.127222898285695));
#47315=CARTESIAN_POINT('Ctrl Pts',(-0.0736925781380903,-0.0871433276491138,
-0.120895237269823));
#47316=CARTESIAN_POINT('Ctrl Pts',(0.0328513340057859,-0.109294767937933,
-0.114567576253951));
#47317=CARTESIAN_POINT('Ctrl Pts',(0.109525864708063,-0.0320723516270534,
-0.10823991523808));
#47318=CARTESIAN_POINT('Ctrl Pts',(0.0866164940802407,0.0743111196969755,
-0.101912254222207));
#47319=CARTESIAN_POINT('Ctrl Pts',(-0.0150471265603088,0.113128890038952,
-0.0955845932063355));
#47320=CARTESIAN_POINT('Ctrl Pts',(-0.103029249389535,0.0490866516361247,
-0.0892569321904636));
#47321=CARTESIAN_POINT('Ctrl Pts',(-0.0973347490159742,-0.0595864002598666,
-0.0829292711745916));
#47322=CARTESIAN_POINT('Ctrl Pts',(-0.0031399522792829,-0.114082097613606,
-0.0766016101587196));
#47323=CARTESIAN_POINT('Ctrl Pts',(0.0939081973359286,-0.0648506831041721,
-0.0702739491428478));
#47324=CARTESIAN_POINT('Ctrl Pts',(0.105575394673151,0.0433438440773199,
-0.0639462881269755));
#47325=CARTESIAN_POINT('Ctrl Pts',(0.0212448220591022,0.112130713062334,
-0.057618627111104));
#47326=CARTESIAN_POINT('Ctrl Pts',(-0.0823913570012463,0.0789618551753083,
-0.0512909660952317));
#47327=CARTESIAN_POINT('Ctrl Pts',(-0.111135465058482,-0.0259949443945141,
-0.0449633050793599));
#47328=CARTESIAN_POINT('Ctrl Pts',(-0.0387933145627912,-0.107328519621086,
-0.0386356440634877));
#47329=CARTESIAN_POINT('Ctrl Pts',(0.0687470363868423,-0.0910529777988239,
-0.0323079830476161));
#47330=CARTESIAN_POINT('Ctrl Pts',(0.113921978618372,0.0079660765599,-0.0259803220317439));
#47331=CARTESIAN_POINT('Ctrl Pts',(0.0552360881026894,0.0998320942404049,
-0.0196526610158721));
#47332=CARTESIAN_POINT('Ctrl Pts',(-0.0169523777846908,0.10042205443332,
-0.015434220338624));
#47333=CARTESIAN_POINT('Ctrl Pts',(-0.0452560140322625,0.0854280329804665,
-0.013325));
#47334=CARTESIAN_POINT('Ctrl Pts',(-0.0724605943221337,-0.0518199049426082,
-0.958091101587196));
#47335=CARTESIAN_POINT('Ctrl Pts',(-0.0552918537025914,-0.0758272270407944,
-0.955981881248572));
#47336=CARTESIAN_POINT('Ctrl Pts',(0.00447277684868737,-0.105039400309431,
-0.951763440571323));
#47337=CARTESIAN_POINT('Ctrl Pts',(0.0906553867201687,-0.0534362549899266,
-0.945435779555453));
#47338=CARTESIAN_POINT('Ctrl Pts',(0.0941438892734977,0.0467935708496025,
-0.939108118539579));
#47339=CARTESIAN_POINT('Ctrl Pts',(0.0121689244744929,0.104455844513668,
-0.932780457523709));
#47340=CARTESIAN_POINT('Ctrl Pts',(-0.0809406622208554,0.0671553054719232,
-0.926452796507834));
#47341=CARTESIAN_POINT('Ctrl Pts',(-0.100419774577854,-0.0312106900785216,
-0.920125135491966));
#47342=CARTESIAN_POINT('Ctrl Pts',(-0.0286139122961286,-0.101195903024898,
-0.91379747447609));
#47343=CARTESIAN_POINT('Ctrl Pts',(0.0692187845179366,-0.0791726463121411,
-0.907469813460221));
#47344=CARTESIAN_POINT('Ctrl Pts',(0.10411042166066,0.0148374614584551,
-0.901142152444347));
#47345=CARTESIAN_POINT('Ctrl Pts',(0.0443448187857815,0.095356473973601,
-0.894814491428477));
#47346=CARTESIAN_POINT('Ctrl Pts',(-0.0557418326386755,0.0891749690747734,
-0.888486830412603));
#47347=CARTESIAN_POINT('Ctrl Pts',(-0.105145664594354,0.0019129709953397,
-0.882159169396733));
#47348=CARTESIAN_POINT('Ctrl Pts',(-0.0589485490078265,-0.0870882858494668,
-0.87583150838086));
#47349=CARTESIAN_POINT('Ctrl Pts',(0.0408464490779558,-0.0969064841664184,
-0.869503847364989));
#47350=CARTESIAN_POINT('Ctrl Pts',(0.103502602166471,-0.0186145901560687,
-0.863176186349116));
#47351=CARTESIAN_POINT('Ctrl Pts',(0.0720513688946276,0.0766021975733563,
-0.856848525333245));
#47352=CARTESIAN_POINT('Ctrl Pts',(-0.0249110073591139,0.102170139719473,
-0.850520864317372));
#47353=CARTESIAN_POINT('Ctrl Pts',(-0.0992235851098809,0.0348421434225487,
-0.844193203301501));
#47354=CARTESIAN_POINT('Ctrl Pts',(-0.0833193256452169,-0.0641652983054661,
-0.837865542285629));
#47355=CARTESIAN_POINT('Ctrl Pts',(0.00834118923185522,-0.104831865071198,
-0.831537881269756));
#47356=CARTESIAN_POINT('Ctrl Pts',(0.0924176601256532,-0.0501823809496229,
-0.825210220253886));
#47357=CARTESIAN_POINT('Ctrl Pts',(0.0924654226286142,0.0500943209112546,
-0.818882559238012));
#47358=CARTESIAN_POINT('Ctrl Pts',(0.00844104773377868,0.104823871570765,
-0.812554898222141));
#47359=CARTESIAN_POINT('Ctrl Pts',(-0.083258162413097,0.0642446396010664,
-0.806227237206269));
#47360=CARTESIAN_POINT('Ctrl Pts',(-0.0992567333879196,-0.0347476073813297,
-0.799899576190397));
#47361=CARTESIAN_POINT('Ctrl Pts',(-0.0250083187288948,-0.102146362295717,
-0.793571915174525));
#47362=CARTESIAN_POINT('Ctrl Pts',(0.0719783555540055,-0.0766708006123362,
-0.787244254158653));
#47363=CARTESIAN_POINT('Ctrl Pts',(0.103520304952373,0.0185159876747599,
-0.780916593142782));
#47364=CARTESIAN_POINT('Ctrl Pts',(0.0409387108295975,0.0968675244426629,
-0.774588932126909));
#47365=CARTESIAN_POINT('Ctrl Pts',(-0.058865498999529,0.0871444109711961,
-0.768261271111037));
#47366=CARTESIAN_POINT('Ctrl Pts',(-0.105147558191447,-0.00181282725558375,
-0.761933610095165));
#47367=CARTESIAN_POINT('Ctrl Pts',(-0.0558265299234932,-0.089121792468657,
-0.755605949079293));
#47368=CARTESIAN_POINT('Ctrl Pts',(0.0442535336888328,-0.0953987426132174,
-0.749278288063421));
#47369=CARTESIAN_POINT('Ctrl Pts',(0.104097052351647,-0.0149364998533759,
-0.74295062704755));
#47370=CARTESIAN_POINT('Ctrl Pts',(0.069292632714499,0.0791064244397399,
-0.736622966031677));
#47371=CARTESIAN_POINT('Ctrl Pts',(-0.0285145778528813,0.101223585127291,
-0.730295305015805));
#47372=CARTESIAN_POINT('Ctrl Pts',(-0.100395540325034,0.0313054439195385,
-0.723967643999934));
#47373=CARTESIAN_POINT('Ctrl Pts',(-0.0809940822907079,-0.0670764785154766,
-0.717639982984061));
#47374=CARTESIAN_POINT('Ctrl Pts',(0.012049450423971,-0.104470599120672,
-0.71131232196819));
#47375=CARTESIAN_POINT('Ctrl Pts',(0.094137287328756,-0.0468771423034273,
-0.704984660952317));
#47376=CARTESIAN_POINT('Ctrl Pts',(0.090632881595485,0.0533383174636288,
-0.698656999936446));
#47377=CARTESIAN_POINT('Ctrl Pts',(0.00472253648757906,0.105057093931231,
-0.692329338920574));
#47378=CARTESIAN_POINT('Ctrl Pts',(-0.0854816702811205,0.0612550355652661,
-0.686001677904702));
#47379=CARTESIAN_POINT('Ctrl Pts',(-0.0979635624237802,-0.0382418066178133,
-0.67967401688883));
#47380=CARTESIAN_POINT('Ctrl Pts',(-0.0213742560796902,-0.102968133484064,
-0.673346355872957));
#47381=CARTESIAN_POINT('Ctrl Pts',(0.0746491190005382,-0.0740729665167775,
-0.667018694857086));
#47382=CARTESIAN_POINT('Ctrl Pts',(0.102799436682193,0.0221714039694361,
-0.660691033841214));
#47383=CARTESIAN_POINT('Ctrl Pts',(0.0374816443594792,0.0982569166637223,
-0.654363372825342));
#47384=CARTESIAN_POINT('Ctrl Pts',(-0.0619155025901194,0.0850045050286458,
-0.64803571180947));
#47385=CARTESIAN_POINT('Ctrl Pts',(-0.105017350714686,-0.00553636929954055,
-0.641708050793597));
#47386=CARTESIAN_POINT('Ctrl Pts',(-0.0526344996447092,-0.0910434225153208,
-0.635380389777726));
#47387=CARTESIAN_POINT('Ctrl Pts',(0.0476051039678494,-0.0937712611217446,
-0.629052728761854));
#47388=CARTESIAN_POINT('Ctrl Pts',(0.104560821617178,-0.0112396583085458,
-0.622725067745982));
#47389=CARTESIAN_POINT('Ctrl Pts',(0.0664469290382389,0.0815113547767389,
-0.61639740673011));
#47390=CARTESIAN_POINT('Ctrl Pts',(-0.0320823614577048,0.10014997463529,
-0.610069745714238));
#47391=CARTESIAN_POINT('Ctrl Pts',(-0.10144147566952,0.0277294491496382,
-0.603742084698366));
#47392=CARTESIAN_POINT('Ctrl Pts',(-0.0785671758384483,-0.0699034635545515,
-0.597414423682494));
#47393=CARTESIAN_POINT('Ctrl Pts',(0.015742587755945,-0.103978200921628,
-0.591086762666622));
#47394=CARTESIAN_POINT('Ctrl Pts',(0.0957387522527569,-0.0435130630183326,
-0.584759101650751));
#47395=CARTESIAN_POINT('Ctrl Pts',(0.0886865776141488,0.0565153632850548,
-0.578431440634878));
#47396=CARTESIAN_POINT('Ctrl Pts',(0.000998097370316146,0.105158447771881,
-0.572103779619006));
#47397=CARTESIAN_POINT('Ctrl Pts',(-0.087597880791936,0.0581885436912965,
-0.565776118603135));
#47398=CARTESIAN_POINT('Ctrl Pts',(-0.0965474268115447,-0.0416880044163974,
-0.559448457587262));
#47399=CARTESIAN_POINT('Ctrl Pts',(-0.0177133642715224,-0.103660658218711,
-0.553120796571391));
#47400=CARTESIAN_POINT('Ctrl Pts',(0.0772261822449981,-0.0713821554172644,
-0.546793135555518));
#47401=CARTESIAN_POINT('Ctrl Pts',(0.10194953370971,0.0257989905330583,
-0.540465474539647));
#47402=CARTESIAN_POINT('Ctrl Pts',(0.0339775306158899,0.0995229759874494,
-0.534137813523775));
#47403=CARTESIAN_POINT('Ctrl Pts',(-0.0648877893265522,0.0827579007253394,
-0.527810152507903));
#47404=CARTESIAN_POINT('Ctrl Pts',(-0.104755324587893,-0.00925296204667948,
-0.521482491492031));
#47405=CARTESIAN_POINT('Ctrl Pts',(-0.049376402104582,-0.0928507741020977,
-0.515154830476159));
#47406=CARTESIAN_POINT('Ctrl Pts',(0.0508969199248936,-0.0920260771646337,
-0.508827169460287));
#47407=CARTESIAN_POINT('Ctrl Pts',(0.104893345271262,-0.00752870865129053,
-0.502499508444414));
#47408=CARTESIAN_POINT('Ctrl Pts',(0.0635178206248455,0.0838139713843825,
-0.496171847428543));
#47409=CARTESIAN_POINT('Ctrl Pts',(-0.0356098750159982,0.098950655063507,
-0.489844186412671));
#47410=CARTESIAN_POINT('Ctrl Pts',(-0.102360080831417,0.0241186481449105,
-0.483516525396799));
#47411=CARTESIAN_POINT('Ctrl Pts',(-0.0760416512146703,-0.0726427051857141,
-0.477188864380927));
#47412=CARTESIAN_POINT('Ctrl Pts',(0.0194159648610402,-0.103355288421382,
-0.470861203365055));
#47413=CARTESIAN_POINT('Ctrl Pts',(0.097220045099944,-0.0400943657752184,
-0.464533542349183));
#47414=CARTESIAN_POINT('Ctrl Pts',(0.0866289535041628,0.059621470553197,
-0.458205881333311));
#47415=CARTESIAN_POINT('Ctrl Pts',(-0.00272759456705263,0.105127805855682,
-0.45187822031744));
#47416=CARTESIAN_POINT('Ctrl Pts',(-0.0896041377153937,0.0550490130741048,
-0.445550559301567));
#47417=CARTESIAN_POINT('Ctrl Pts',(-0.0950101040674725,-0.0450818750856725,
-0.439222898285696));
#47418=CARTESIAN_POINT('Ctrl Pts',(-0.0140302385014343,-0.104223067234394,
-0.432895237269823));
#47419=CARTESIAN_POINT('Ctrl Pts',(0.0797063105442395,-0.0686017448435343,
-0.426567576253952));
#47420=CARTESIAN_POINT('Ctrl Pts',(0.100971662835955,0.0293941939895359,
-0.420239915238079));
#47421=CARTESIAN_POINT('Ctrl Pts',(0.0304307679937315,0.100664113245306,
-0.413912254222208));
#47422=CARTESIAN_POINT('Ctrl Pts',(-0.0677786283710122,0.0804074180178444,
-0.407584593206336));
#47423=CARTESIAN_POINT('Ctrl Pts',(-0.104361808707819,-0.0129579403990236,
-0.401256932190463));
#47424=CARTESIAN_POINT('Ctrl Pts',(-0.0460563268945252,-0.0945415786262148,
-0.394929271174592));
#47425=CARTESIAN_POINT('Ctrl Pts',(0.0541248496454143,-0.0901653813113073,
-0.38860161015872));
#47426=CARTESIAN_POINT('Ctrl Pts',(0.105094205927356,-0.00380830889641988,
-0.382273949142848));
#47427=CARTESIAN_POINT('Ctrl Pts',(0.0605089841155697,0.0860113839991769,
-0.375946288126976));
#47428=CARTESIAN_POINT('Ctrl Pts',(-0.0390926907634774,0.0976271318078293,
-0.369618627111104));
#47429=CARTESIAN_POINT('Ctrl Pts',(-0.103150202769885,0.0204775732127567,
-0.363290966095232));
#47430=CARTESIAN_POINT('Ctrl Pts',(-0.0734206784788588,-0.0752907650901236,
-0.35696330507936));
#47431=CARTESIAN_POINT('Ctrl Pts',(0.0230649708858186,-0.102602643504875,
-0.350635644063488));
#47432=CARTESIAN_POINT('Ctrl Pts',(0.0985793065392342,-0.0366253417512498,
-0.344307983047616));
#47433=CARTESIAN_POINT('Ctrl Pts',(0.0844625920123951,0.0626527404564226,
-0.337980322031744));
#47434=CARTESIAN_POINT('Ctrl Pts',(-0.00644986280507308,0.10496520664462,
-0.331652661015872));
#47435=CARTESIAN_POINT('Ctrl Pts',(-0.0914979227811434,0.0518403844785903,
-0.325325));
#47436=CARTESIAN_POINT('Ctrl Pts',(-0.0933535238518378,-0.0484191586109931,
-0.318997338984129));
#47437=CARTESIAN_POINT('Ctrl Pts',(-0.010329501859476,-0.104654654590645,
-0.312669677968256));
#47438=CARTESIAN_POINT('Ctrl Pts',(0.0820863908206271,-0.0657352247900273,
-0.306342016952385));
#47439=CARTESIAN_POINT('Ctrl Pts',(0.0998670514925671,0.0329525016096368,
-0.300014355936512));
#47440=CARTESIAN_POINT('Ctrl Pts',(0.026845808418899,0.101678896072331,
-0.293686694920641));
#47441=CARTESIAN_POINT('Ctrl Pts',(-0.0705843911183263,0.0779560072515728,
-0.287359033904769));
#47442=CARTESIAN_POINT('Ctrl Pts',(-0.103837297018865,-0.0166466538369796,
-0.281031372888896));
#47443=CARTESIAN_POINT('Ctrl Pts',(-0.0426784414005113,-0.096113713775794,
-0.274703711873025));
#47444=CARTESIAN_POINT('Ctrl Pts',(0.0572848414052219,-0.0881915091226506,
-0.268376050857152));
#47445=CARTESIAN_POINT('Ctrl Pts',(0.1051631514635,-8.31289205999597E-5,
-0.262048389841281));
#47446=CARTESIAN_POINT('Ctrl Pts',(0.0574241962269787,0.0881008344105628,
-0.255720728825408));
#47447=CARTESIAN_POINT('Ctrl Pts',(-0.0425264370408898,0.0961810661656361,
-0.249393067809537));
#47448=CARTESIAN_POINT('Ctrl Pts',(-0.103810849717319,0.0168107946606686,
-0.243065406793664));
#47449=CARTESIAN_POINT('Ctrl Pts',(-0.0707075474977308,-0.0778443194010069,
-0.236737745777793));
#47450=CARTESIAN_POINT('Ctrl Pts',(0.02668502556757,-0.101721210898243,
-0.230410084761921));
#47451=CARTESIAN_POINT('Ctrl Pts',(0.0998148304144701,-0.0331103452942156,
-0.224082423746049));
#47452=CARTESIAN_POINT('Ctrl Pts',(0.0821902123736124,0.0656053681196284,
-0.217754762730176));
#47453=CARTESIAN_POINT('Ctrl Pts',(-0.0101640351214257,0.104670854234478,
-0.211427101714305));
#47454=CARTESIAN_POINT('Ctrl Pts',(-0.0932768588950464,0.0485666854021975,
-0.205099440698433));
#47455=CARTESIAN_POINT('Ctrl Pts',(-0.0915797655167434,-0.0516956660067222,
-0.198771779682561));
#47456=CARTESIAN_POINT('Ctrl Pts',(-0.00661579954317001,-0.104954878554757,
-0.192444118666689));
#47457=CARTESIAN_POINT('Ctrl Pts',(0.0843634355817327,-0.0627861933377942,
-0.186116457650817));
#47458=CARTESIAN_POINT('Ctrl Pts',(0.0986370861891049,0.0364694469785133,
-0.179788796634945));
#47459=CARTESIAN_POINT('Ctrl Pts',(0.0232271517771629,0.102566050700096,
-0.173461135619074));
#47460=CARTESIAN_POINT('Ctrl Pts',(-0.0733015557797646,0.0754067454663942,
-0.167133474603201));
#47461=CARTESIAN_POINT('Ctrl Pts',(-0.103182447839406,-0.0203144722733525,
-0.16080581358733));
#47462=CARTESIAN_POINT('Ctrl Pts',(-0.039246985673088,-0.0975652061623642,
-0.154478152571457));
#47463=CARTESIAN_POINT('Ctrl Pts',(0.0603729289472908,-0.0861069382789412,
-0.148150491555585));
#47464=CARTESIAN_POINT('Ctrl Pts',(0.10510009497664,0.00364215551222339,
-0.141822830539713));
#47465=CARTESIAN_POINT('Ctrl Pts',(0.0542673296971727,0.090079699708902,
-0.135495169523841));
#47466=CARTESIAN_POINT('Ctrl Pts',(-0.0459068050839857,0.0946142736566952,
-0.129167508507969));
#47467=CARTESIAN_POINT('Ctrl Pts',(-0.10434118995342,0.0131229142891147,
-0.122839847492097));
#47468=CARTESIAN_POINT('Ctrl Pts',(-0.0679056685023866,-0.0803001614144492,
-0.116512186476226));
#47469=CARTESIAN_POINT('Ctrl Pts',(0.0302715938731016,-0.100712099754892,
-0.110184525460353));
#47470=CARTESIAN_POINT('Ctrl Pts',(0.100925049024152,-0.0295537831991381,
-0.103856864444482));
#47471=CARTESIAN_POINT('Ctrl Pts',(0.0798146988809391,0.0684756374071776,
-0.0975292034286096));
#47472=CARTESIAN_POINT('Ctrl Pts',(-0.0138655101223774,0.104245137015464,
-0.0912015424127377));
#47473=CARTESIAN_POINT('Ctrl Pts',(-0.0949385980496625,0.0452319891380204,
-0.0848738813968657));
#47474=CARTESIAN_POINT('Ctrl Pts',(-0.0896912737678446,-0.054907216513919,
-0.0785462203809937));
#47475=CARTESIAN_POINT('Ctrl Pts',(-0.00289337900745932,-0.105123491379144,
-0.0722185593651219));
#47476=CARTESIAN_POINT('Ctrl Pts',(0.0865338013551485,-0.0597581072652013,
-0.06589089834925));
#47477=CARTESIAN_POINT('Ctrl Pts',(0.0972848003668635,0.0399401511237437,
-0.0595632373333777));
#47478=CARTESIAN_POINT('Ctrl Pts',(0.019576514766986,0.103325344594117,
-0.0532355763175061));
#47479=CARTESIAN_POINT('Ctrl Pts',(-0.0759213521544111,0.0727611612640329,
-0.0469079153016338));
#47480=CARTESIAN_POINT('Ctrl Pts',(-0.102408251140003,-0.0239536208583187,
-0.0405802542857621));
#47481=CARTESIAN_POINT('Ctrl Pts',(-0.0357469642855133,-0.0989002564218097,
-0.0342525932698899));
#47482=CARTESIAN_POINT('Ctrl Pts',(0.0633484888350438,-0.0839027956787714,
-0.0279249322540183));
#47483=CARTESIAN_POINT('Ctrl Pts',(0.104975946162434,0.00734051878504697,
-0.021597271238146));
#47484=CARTESIAN_POINT('Ctrl Pts',(0.0508985244218387,0.0919925081829091,
-0.0152696102222743));
#47485=CARTESIAN_POINT('Ctrl Pts',(-0.015621146325174,0.0925361401510375,
-0.0110511695450261));
#47486=CARTESIAN_POINT('Ctrl Pts',(-0.0417021627450121,0.0787195649134718,
-0.00894194920640216));
#47487=CARTESIAN_POINT('Ctrl Pts',(-0.066285514675037,-0.0474038213689209,
-0.953708050793598));
#47488=CARTESIAN_POINT('Ctrl Pts',(-0.050579891240191,-0.0693652435202928,
-0.951598830454974));
#47489=CARTESIAN_POINT('Ctrl Pts',(0.00409160755877578,-0.0960879603017703,
-0.947380389777727));
#47490=CARTESIAN_POINT('Ctrl Pts',(0.0829297499285808,-0.0488824263373707,
-0.941052728761854));
#47491=CARTESIAN_POINT('Ctrl Pts',(0.0861209628817152,0.0428058306209787,
-0.934725067745982));
#47492=CARTESIAN_POINT('Ctrl Pts',(0.0111318907798004,0.0955541350326624,
-0.92839740673011));
#47493=CARTESIAN_POINT('Ctrl Pts',(-0.0740429126153175,0.0614323416473282,
-0.922069745714238));
#47494=CARTESIAN_POINT('Ctrl Pts',(-0.0918620182971786,-0.028550920325338,
-0.915742084698367));
#47495=CARTESIAN_POINT('Ctrl Pts',(-0.0261754395083107,-0.0925720052086505,
-0.909414423682494));
#47496=CARTESIAN_POINT('Ctrl Pts',(0.0633199713564921,-0.0724255667246425,
-0.903086762666622));
#47497=CARTESIAN_POINT('Ctrl Pts',(0.0952381490570246,0.013573015491322,
-0.89675910165075));
#47498=CARTESIAN_POINT('Ctrl Pts',(0.0405657607957116,0.0872302113178526,
-0.890431440634878));
#47499=CARTESIAN_POINT('Ctrl Pts',(-0.0509915230471101,0.081575493225651,
-0.884103779619006));
#47500=CARTESIAN_POINT('Ctrl Pts',(-0.0961851687622249,0.00174994792922621,
-0.877776118603136));
#47501=CARTESIAN_POINT('Ctrl Pts',(-0.0539249635872344,-0.0796666367934459,
-0.871448457587261));
#47502=CARTESIAN_POINT('Ctrl Pts',(0.0373655215653255,-0.0886481299030314,
-0.865120796571392));
#47503=CARTESIAN_POINT('Ctrl Pts',(0.094682127837785,-0.0170282579173243,
-0.858793135555518));
#47504=CARTESIAN_POINT('Ctrl Pts',(0.0659111633695569,0.0700741711945603,
-0.852465474539647));
#47505=CARTESIAN_POINT('Ctrl Pts',(-0.022788095506527,0.0934632176161583,
-0.846137813523775));
#47506=CARTESIAN_POINT('Ctrl Pts',(-0.0907677678942492,0.0318729018268572,
-0.839810152507903));
#47507=CARTESIAN_POINT('Ctrl Pts',(-0.0762188667431783,-0.058697142388134,
-0.83348249149203));
#47508=CARTESIAN_POINT('Ctrl Pts',(0.00763035449001975,-0.0958981111815948,
-0.827154830476159));
#47509=CARTESIAN_POINT('Ctrl Pts',(0.0845418426911846,-0.0459058468948889,
-0.820827169460287));
#47510=CARTESIAN_POINT('Ctrl Pts',(0.0845855348816854,0.0458252913181626,
-0.814499508444415));
#47511=CARTESIAN_POINT('Ctrl Pts',(0.00772170306722385,0.0958907988859224,
-0.808171847428543));
#47512=CARTESIAN_POINT('Ctrl Pts',(-0.0761629158314008,0.0587697222318829,
-0.801844186412671));
#47513=CARTESIAN_POINT('Ctrl Pts',(-0.0907980912816151,-0.0317864221311527,
-0.795516525396799));
#47514=CARTESIAN_POINT('Ctrl Pts',(-0.0228771140177608,-0.0934414665004511,
-0.789188864380927));
#47515=CARTESIAN_POINT('Ctrl Pts',(0.0658443722135284,-0.0701369278941099,
-0.782861203365055));
#47516=CARTESIAN_POINT('Ctrl Pts',(0.094698321995253,0.0169380583228695,
-0.776533542349183));
#47517=CARTESIAN_POINT('Ctrl Pts',(0.0374499207860274,0.0886124903203744,
-0.770205881333311));
#47518=CARTESIAN_POINT('Ctrl Pts',(-0.0538489910866597,0.0797179789417516,
-0.76387822031744));
#47519=CARTESIAN_POINT('Ctrl Pts',(-0.096186900987293,-0.00165833842210959,
-0.757550559301566));
#47520=CARTESIAN_POINT('Ctrl Pts',(-0.0510690024435771,-0.0815268483209539,
-0.751222898285696));
#47521=CARTESIAN_POINT('Ctrl Pts',(0.040482254999354,-0.0872688778311181,
-0.744895237269823));
#47522=CARTESIAN_POINT('Ctrl Pts',(0.0952259190782751,-0.0136636138509041,
-0.738567576253951));
#47523=CARTESIAN_POINT('Ctrl Pts',(0.0633875262221782,0.0723649882690567,
-0.732239915238079));
#47524=CARTESIAN_POINT('Ctrl Pts',(-0.0260845703295907,0.0925973282469388,
-0.725912254222209));
#47525=CARTESIAN_POINT('Ctrl Pts',(-0.0918398492833032,0.0286375992599782,
-0.719584593206334));
#47526=CARTESIAN_POINT('Ctrl Pts',(-0.0740917802358122,-0.0613602323108368,
-0.713256932190464));
#47527=CARTESIAN_POINT('Ctrl Pts',(0.0110225982877466,-0.095567632254542,
-0.706929271174592));
#47528=CARTESIAN_POINT('Ctrl Pts',(0.0861149235535926,-0.0428822801295805,
-0.700601610158719));
#47529=CARTESIAN_POINT('Ctrl Pts',(0.0829091626868333,0.0487928350305729,
-0.694273949142848));
#47530=CARTESIAN_POINT('Ctrl Pts',(0.00432008272329617,0.0961041460761004,
-0.687946288126975));
#47531=CARTESIAN_POINT('Ctrl Pts',(-0.0781969367333093,0.056034891748619,
-0.681618627111104));
#47532=CARTESIAN_POINT('Ctrl Pts',(-0.0896151241292935,-0.0349828462970623,
-0.675290966095232));
#47533=CARTESIAN_POINT('Ctrl Pts',(-0.0195527455756119,-0.0941932064864976,
-0.668963305079359));
#47534=CARTESIAN_POINT('Ctrl Pts',(0.0682875336488553,-0.0677604807827472,
-0.662635644063488));
#47535=CARTESIAN_POINT('Ctrl Pts',(0.0940388859976769,0.0202819606564187,
-0.656307983047616));
#47536=CARTESIAN_POINT('Ctrl Pts',(0.0342874649383861,0.089883478770303,
-0.649980322031744));
#47537=CARTESIAN_POINT('Ctrl Pts',(-0.0566390738848248,0.0777604354233048,
-0.643652661015872));
#47538=CARTESIAN_POINT('Ctrl Pts',(-0.0960677897697764,-0.00506456084005674,
-0.637325000000001));
#47539=CARTESIAN_POINT('Ctrl Pts',(-0.0481489964476719,-0.0832847173786083,
-0.630997338984128));
#47540=CARTESIAN_POINT('Ctrl Pts',(0.0435482050235359,-0.0857800900383107,
-0.624669677968256));
#47541=CARTESIAN_POINT('Ctrl Pts',(0.0956501660050871,-0.010281816520044,
-0.618342016952384));
#47542=CARTESIAN_POINT('Ctrl Pts',(0.0607843329340448,0.0745649708476828,
-0.612014355936513));
#47543=CARTESIAN_POINT('Ctrl Pts',(-0.0293483080163605,0.0916152106602906,
-0.60568669492064));
#47544=CARTESIAN_POINT('Ctrl Pts',(-0.0927966501938481,0.0253663501622369,
-0.599359033904769));
#47545=CARTESIAN_POINT('Ctrl Pts',(-0.0718716943427677,-0.0639463021608941,
-0.593031372888896));
#47546=CARTESIAN_POINT('Ctrl Pts',(0.0144010070781465,-0.0951171961471098,
-0.586703711873026));
#47547=CARTESIAN_POINT('Ctrl Pts',(0.0875799119064274,-0.0398048871147124,
-0.580376050857152));
#47548=CARTESIAN_POINT('Ctrl Pts',(0.0811287224030647,0.0516991335420534,
-0.574048389841281));
#47549=CARTESIAN_POINT('Ctrl Pts',(0.000913039680479169,0.0961968625595162,
-0.567720728825409));
#47550=CARTESIAN_POINT('Ctrl Pts',(-0.0801328041407242,0.0532297257958081,
-0.561393067809536));
#47551=CARTESIAN_POINT('Ctrl Pts',(-0.0883196713554814,-0.0381353596995275,
-0.555065406793665));
#47552=CARTESIAN_POINT('Ctrl Pts',(-0.0162038343509091,-0.0948267143798671,
-0.548737745777793));
#47553=CARTESIAN_POINT('Ctrl Pts',(0.0706449799975524,-0.0652989801520513,
-0.542410084761921));
#47554=CARTESIAN_POINT('Ctrl Pts',(0.0932614116134009,0.023600404903908,
-0.536082423746049));
#47555=CARTESIAN_POINT('Ctrl Pts',(0.0310819711779969,0.0910416447316434,
-0.529754762730177));
#47556=CARTESIAN_POINT('Ctrl Pts',(-0.0593580628460573,0.0757052863604391,
-0.523427101714304));
#47557=CARTESIAN_POINT('Ctrl Pts',(-0.095828093465389,-0.00846442617909054,
-0.517099440698433));
#47558=CARTESIAN_POINT('Ctrl Pts',(-0.0451685534313103,-0.0849380467674849,
-0.510771779682561));
#47559=CARTESIAN_POINT('Ctrl Pts',(0.0465594929790022,-0.0841836303641677,
-0.504444118666689));
#47560=CARTESIAN_POINT('Ctrl Pts',(0.095954352049361,-0.00688711336772415,
-0.498116457650817));
#47561=CARTESIAN_POINT('Ctrl Pts',(0.0581048426464326,0.0766713588557415,
-0.491788796634945));
#47562=CARTESIAN_POINT('Ctrl Pts',(-0.0325752074631849,0.0905180969004709,
-0.485461135619073));
#47563=CARTESIAN_POINT('Ctrl Pts',(-0.0936369719785242,0.0220632610111395,
-0.479133474603201));
#47564=CARTESIAN_POINT('Ctrl Pts',(-0.069561394502176,-0.0664521060814872,
-0.47280581358733));
#47565=CARTESIAN_POINT('Ctrl Pts',(0.0177613396048748,-0.0945473681452471,
-0.466478152571457));
#47566=CARTESIAN_POINT('Ctrl Pts',(0.0889349692265999,-0.0366775306750104,
-0.460150491555585));
#47567=CARTESIAN_POINT('Ctrl Pts',(0.0792464486732655,0.054540538871816,
-0.453822830539714));
#47568=CARTESIAN_POINT('Ctrl Pts',(-0.0024951494173252,0.0961688319422557,
-0.447495169523841));
#47569=CARTESIAN_POINT('Ctrl Pts',(-0.0819680881869817,0.0503577454491741,
-0.44116750850797));
#47570=CARTESIAN_POINT('Ctrl Pts',(-0.0869133589968021,-0.0412400052818326,
-0.434839847492097));
#47571=CARTESIAN_POINT('Ctrl Pts',(-0.0128345839387771,-0.0953411949939326,
-0.428512186476226));
#47572=CARTESIAN_POINT('Ctrl Pts',(0.0729137521807407,-0.0627555156992445,
-0.422184525460353));
#47573=CARTESIAN_POINT('Ctrl Pts',(0.0923668747308512,0.026889225727191,
-0.415856864444482));
#47574=CARTESIAN_POINT('Ctrl Pts',(0.0278374630692892,0.0920855344645321,
-0.409529203428609));
#47575=CARTESIAN_POINT('Ctrl Pts',(-0.0620025450739129,0.0735551113934987,
-0.403201542412738));
#47576=CARTESIAN_POINT('Ctrl Pts',(-0.0954681129423542,-0.0118536669000983,
-0.396873881396865));
#47577=CARTESIAN_POINT('Ctrl Pts',(-0.0421314144716149,-0.0864847612147573,
-0.390546220380994));
#47578=CARTESIAN_POINT('Ctrl Pts',(0.0495123390722645,-0.0824815026981547,
-0.384218559365122));
#47579=CARTESIAN_POINT('Ctrl Pts',(0.0961380953941644,-0.0034837654535165,
-0.37789089834925));
#47580=CARTESIAN_POINT('Ctrl Pts',(0.0553524186778445,0.0786815083375071,
-0.371563237333378));
#47581=CARTESIAN_POINT('Ctrl Pts',(-0.0357612182391062,0.0893073640737851,
-0.365235576317505));
#47582=CARTESIAN_POINT('Ctrl Pts',(-0.094359759858438,0.0187324778716134,
-0.358907915301635));
#47583=CARTESIAN_POINT('Ctrl Pts',(-0.0671637806215868,-0.0688744987667276,
-0.352580254285761));
#47584=CARTESIAN_POINT('Ctrl Pts',(0.0210993779506474,-0.0938588635017939,
-0.346252593269891));
#47585=CARTESIAN_POINT('Ctrl Pts',(0.0901783946349084,-0.0335041362942443,
-0.339924932254018));
#47586=CARTESIAN_POINT('Ctrl Pts',(0.0772647041430507,0.0573134844642988,
-0.333597271238147));
#47587=CARTESIAN_POINT('Ctrl Pts',(-0.00590020658286327,0.0960200894085823,
-0.327269610222274));
#47588=CARTESIAN_POINT('Ctrl Pts',(-0.0837004852083069,0.047422555642295,
-0.320941949206402));
#47589=CARTESIAN_POINT('Ctrl Pts',(-0.0853979522682061,-0.0442928860670627,
-0.31461428819053));
#47590=CARTESIAN_POINT('Ctrl Pts',(-0.00944922345031021,-0.0957360025483553,
-0.308286627174658));
#47591=CARTESIAN_POINT('Ctrl Pts',(0.0750910024167363,-0.0601332800020278,
-0.301958966158787));
#47592=CARTESIAN_POINT('Ctrl Pts',(0.091356398180151,0.0301442949710606,
-0.295631305142914));
#47593=CARTESIAN_POINT('Ctrl Pts',(0.0245580131457824,0.0930138376699088,
-0.289303644127042));
#47594=CARTESIAN_POINT('Ctrl Pts',(-0.0645692011923398,0.0713126094399562,
-0.282975983111171));
#47595=CARTESIAN_POINT('Ctrl Pts',(-0.0949883000512143,-0.0152280287999835,
-0.276648322095299));
#47596=CARTESIAN_POINT('Ctrl Pts',(-0.0390413918106268,-0.087922919271608,
-0.270320661079426));
#47597=CARTESIAN_POINT('Ctrl Pts',(0.0524030368663857,-0.0806758435650515,
-0.263993000063555));
#47598=CARTESIAN_POINT('Ctrl Pts',(0.0962011654033275,-7.60446879838475E-5,
-0.257665339047683));
#47599=CARTESIAN_POINT('Ctrl Pts',(0.0525305158936973,0.0805928961366598,
-0.251337678031811));
#47600=CARTESIAN_POINT('Ctrl Pts',(-0.0389023412369373,0.0879845319021287,
-0.245010017015939));
#47601=CARTESIAN_POINT('Ctrl Pts',(-0.0949641065842529,0.015378181570316,
-0.238682356000067));
#47602=CARTESIAN_POINT('Ctrl Pts',(-0.0646818622058288,-0.0712104396092091,
-0.232354694984195));
#47603=CARTESIAN_POINT('Ctrl Pts',(0.0244109321819707,-0.093052546433482,
-0.226027033968323));
#47604=CARTESIAN_POINT('Ctrl Pts',(0.0913086273735362,-0.0302886872434177,
-0.219699372952451));
#47605=CARTESIAN_POINT('Ctrl Pts',(0.075185976314458,0.0600144896952148,
-0.213371711936579));
#47606=CARTESIAN_POINT('Ctrl Pts',(-0.00929785775981484,0.0957508216612688,
-0.207044050920707));
#47607=CARTESIAN_POINT('Ctrl Pts',(-0.0853278206861234,0.0444278406499617,
-0.200716389904835));
#47608=CARTESIAN_POINT('Ctrl Pts',(-0.08377535331976,-0.0472901700542316,
-0.194388728888963));
#47609=CARTESIAN_POINT('Ctrl Pts',(-0.0060520022200805,-0.0960106414767981,
-0.188061067873091));
#47610=CARTESIAN_POINT('Ctrl Pts',(0.0771739978067131,-0.0574355645135913,
-0.181733406857219));
#47611=CARTESIAN_POINT('Ctrl Pts',(0.0902312503127462,0.0333615268477907,
-0.175405745841347));
#47612=CARTESIAN_POINT('Ctrl Pts',(0.0212477378137396,0.0938253891296762,
-0.169078084825475));
#47613=CARTESIAN_POINT('Ctrl Pts',(-0.0670548095388511,0.0689805953148616,
-0.162750423809603));
#47614=CARTESIAN_POINT('Ctrl Pts',(-0.094389257008564,-0.0185832763668021,
-0.156422762793732));
#47615=CARTESIAN_POINT('Ctrl Pts',(-0.0359023641625004,-0.0892507157213992,
-0.150095101777859));
#47616=CARTESIAN_POINT('Ctrl Pts',(0.055227958108097,-0.0787689194976396,
-0.143767440761988));
#47617=CARTESIAN_POINT('Ctrl Pts',(0.0961434825796593,0.003331771632744,
-0.137439779746115));
#47618=CARTESIAN_POINT('Ctrl Pts',(0.0496426769980031,0.082403122867479,
-0.131112118730244));
#47619=CARTESIAN_POINT('Ctrl Pts',(-0.0419946348845927,0.0865512611869807,
-0.124784457714371));
#47620=CARTESIAN_POINT('Ctrl Pts',(-0.095449251314733,0.0120045817430545,
-0.1184567966985));
#47621=CARTESIAN_POINT('Ctrl Pts',(-0.0621187588666827,-0.0734569951797847,
-0.112129135682628));
#47622=CARTESIAN_POINT('Ctrl Pts',(0.0276918537404171,-0.0921294315718511,
-0.105801474666756));
#47623=CARTESIAN_POINT('Ctrl Pts',(0.0923242333402416,-0.0270352147712229,
-0.0994738136508837));
#47624=CARTESIAN_POINT('Ctrl Pts',(0.0730129036816374,0.0626401551173798,
-0.0931461526350118));
#47625=CARTESIAN_POINT('Ctrl Pts',(-0.0126838936844461,0.0953613839919759,
-0.0868184916191398));
#47626=CARTESIAN_POINT('Ctrl Pts',(-0.0868479467097893,0.041377326639916,
-0.0804908306032678));
#47627=CARTESIAN_POINT('Ctrl Pts',(-0.0820477985197149,-0.0502280327679713,
-0.0741631695873958));
#47628=CARTESIAN_POINT('Ctrl Pts',(-0.0026468057356357,-0.096164885144682,
-0.067835508571524));
#47629=CARTESIAN_POINT('Ctrl Pts',(0.0791594053743683,-0.0546655314262305,
-0.0615078475556519));
#47630=CARTESIAN_POINT('Ctrl Pts',(0.0889942060605761,0.0365364581701673,
-0.0551801865397797));
#47631=CARTESIAN_POINT('Ctrl Pts',(0.0179082074748696,0.0945199761258996,
-0.0488525255239083));
#47632=CARTESIAN_POINT('Ctrl Pts',(-0.0694513473075758,0.0665604673527576,
-0.0425248645080359));
#47633=CARTESIAN_POINT('Ctrl Pts',(-0.0936810372215236,-0.0219122973221233,
-0.0361972034921643));
#47634=CARTESIAN_POINT('Ctrl Pts',(-0.0327006140082352,-0.0904719932225328,
-0.029869542476292));
#47635=CARTESIAN_POINT('Ctrl Pts',(0.0579499412832453,-0.0767526135587191,
-0.0235418814604204));
#47636=CARTESIAN_POINT('Ctrl Pts',(0.0960299137064959,0.00671496101019401,
-0.0172142204445481));
#47637=CARTESIAN_POINT('Ctrl Pts',(0.0465609607409879,0.0841529221254132,
-0.0108865594286764));
#47638=CARTESIAN_POINT('Ctrl Pts',(-0.0142899148656573,0.0846502258687555,
-0.00666811875142826));
#47639=CARTESIAN_POINT('Ctrl Pts',(-0.0381483114577617,0.0720110968464772,
-0.00455889841280429));
#47640=CARTESIAN_POINT('Ctrl Pts',(-0.0601104350279403,-0.0429877377952337,
-0.949325));
#47641=CARTESIAN_POINT('Ctrl Pts',(-0.0458679287777906,-0.0629032599997909,
-0.947215779661376));
#47642=CARTESIAN_POINT('Ctrl Pts',(0.00371043826886423,-0.0871365202941097,
-0.942997338984126));
#47643=CARTESIAN_POINT('Ctrl Pts',(0.0752041131369929,-0.0443285976848148,
-0.936669677968258));
#47644=CARTESIAN_POINT('Ctrl Pts',(0.0780980364899326,0.0388180903923549,
-0.930342016952383));
#47645=CARTESIAN_POINT('Ctrl Pts',(0.0100948570851079,0.0866524255516566,
-0.924014355936512));
#47646=CARTESIAN_POINT('Ctrl Pts',(-0.0671451630097795,0.055709377822733,
-0.91768669492064));
#47647=CARTESIAN_POINT('Ctrl Pts',(-0.0833042620165027,-0.0258911505721542,
-0.911359033904769));
#47648=CARTESIAN_POINT('Ctrl Pts',(-0.0237369667204929,-0.0839481073924034,
-0.905031372888896));
#47649=CARTESIAN_POINT('Ctrl Pts',(0.0574211581950477,-0.0656784871371439,
-0.898703711873025));
#47650=CARTESIAN_POINT('Ctrl Pts',(0.0863658764533893,0.0123085695241889,
-0.892376050857153));
#47651=CARTESIAN_POINT('Ctrl Pts',(0.0367867028056418,0.0791039486621042,
-0.88604838984128));
#47652=CARTESIAN_POINT('Ctrl Pts',(-0.0462412134555447,0.0739760173765286,
-0.879720728825409));
#47653=CARTESIAN_POINT('Ctrl Pts',(-0.0872246729300961,0.00158692486311266,
-0.873393067809536));
#47654=CARTESIAN_POINT('Ctrl Pts',(-0.0489013781666423,-0.0722449877374248,
-0.867065406793666));
#47655=CARTESIAN_POINT('Ctrl Pts',(0.0338845940526951,-0.0803897756396443,
-0.860737745777792));
#47656=CARTESIAN_POINT('Ctrl Pts',(0.0858616535090988,-0.0154419256785799,
-0.854410084761921));
#47657=CARTESIAN_POINT('Ctrl Pts',(0.0597709578444863,0.0635461448157645,
-0.848082423746049));
#47658=CARTESIAN_POINT('Ctrl Pts',(-0.0206651836539401,0.0847562955128429,
-0.841754762730177));
#47659=CARTESIAN_POINT('Ctrl Pts',(-0.0823119506786178,0.0289036602311659,
-0.835427101714305));
#47660=CARTESIAN_POINT('Ctrl Pts',(-0.0691184078411397,-0.0532289864708019,
-0.829099440698434));
#47661=CARTESIAN_POINT('Ctrl Pts',(0.00691951974818428,-0.0869643572919913,
-0.82277177968256));
#47662=CARTESIAN_POINT('Ctrl Pts',(0.0766660252567158,-0.0416293128401549,
-0.81644411866669));
#47663=CARTESIAN_POINT('Ctrl Pts',(0.0767056471347569,0.0415562617250705,
-0.810116457650816));
#47664=CARTESIAN_POINT('Ctrl Pts',(0.00700235840066891,0.0869577262010798,
-0.803788796634946));
#47665=CARTESIAN_POINT('Ctrl Pts',(-0.0690676692497047,0.0532948048626995,
-0.797461135619073));
#47666=CARTESIAN_POINT('Ctrl Pts',(-0.0823394491753107,-0.0288252368809756,
-0.791133474603202));
#47667=CARTESIAN_POINT('Ctrl Pts',(-0.0207459093066268,-0.0847365707051847,
-0.784805813587329));
#47668=CARTESIAN_POINT('Ctrl Pts',(0.0597103888730514,-0.0636030551758837,
-0.778478152571458));
#47669=CARTESIAN_POINT('Ctrl Pts',(0.0858763390381331,0.0153601289709793,
-0.772150491555585));
#47670=CARTESIAN_POINT('Ctrl Pts',(0.0339611307424576,0.0803574561980857,
-0.765822830539714));
#47671=CARTESIAN_POINT('Ctrl Pts',(-0.0488324831737906,0.0722915469123074,
-0.759495169523841));
#47672=CARTESIAN_POINT('Ctrl Pts',(-0.0872262437831388,-0.0015038495886356,
-0.75316750850797));
#47673=CARTESIAN_POINT('Ctrl Pts',(-0.0463114749636612,-0.0739319041732507,
-0.746839847492097));
#47674=CARTESIAN_POINT('Ctrl Pts',(0.0367109763098753,-0.0791390130490189,
-0.740512186476226));
#47675=CARTESIAN_POINT('Ctrl Pts',(0.0863547858049027,-0.0123907278484321,
-0.734184525460353));
#47676=CARTESIAN_POINT('Ctrl Pts',(0.0574824197298575,0.0656235520983735,
-0.727856864444481));
#47677=CARTESIAN_POINT('Ctrl Pts',(-0.0236545628063002,0.0839710713665869,
-0.72152920342861));
#47678=CARTESIAN_POINT('Ctrl Pts',(-0.083284158241572,0.025969754600418,
-0.715201542412737));
#47679=CARTESIAN_POINT('Ctrl Pts',(-0.0671894781809166,-0.055643986106197,
-0.708873881396866));
#47680=CARTESIAN_POINT('Ctrl Pts',(0.00999574615152227,-0.0866646653884117,
-0.702546220380994));
#47681=CARTESIAN_POINT('Ctrl Pts',(0.0780925597784293,-0.0388874179557339,
-0.696218559365122));
#47682=CARTESIAN_POINT('Ctrl Pts',(0.0751854437781816,0.0442473525975172,
-0.68989089834925));
#47683=CARTESIAN_POINT('Ctrl Pts',(0.00391762895901338,0.0871511982209692,
-0.683563237333377));
#47684=CARTESIAN_POINT('Ctrl Pts',(-0.0709122031854983,0.050814747931972,
-0.677235576317507));
#47685=CARTESIAN_POINT('Ctrl Pts',(-0.0812666858348066,-0.0317238859763112,
-0.670907915301633));
#47686=CARTESIAN_POINT('Ctrl Pts',(-0.0177312350715336,-0.0854182794889314,
-0.664580254285763));
#47687=CARTESIAN_POINT('Ctrl Pts',(0.0619259482971724,-0.0614479950487169,
-0.65825259326989));
#47688=CARTESIAN_POINT('Ctrl Pts',(0.0852783353131607,0.0183925173434011,
-0.651924932254018));
#47689=CARTESIAN_POINT('Ctrl Pts',(0.0310932855172931,0.0815100408768839,
-0.645597271238146));
#47690=CARTESIAN_POINT('Ctrl Pts',(-0.0513626451795302,0.0705163658179637,
-0.639269610222275));
#47691=CARTESIAN_POINT('Ctrl Pts',(-0.0871182288248673,-0.0045927523805729,
-0.632941949206402));
#47692=CARTESIAN_POINT('Ctrl Pts',(-0.0436634932506345,-0.0755260122418957,
-0.62661428819053));
#47693=CARTESIAN_POINT('Ctrl Pts',(0.0394913060792223,-0.0777889189548767,
-0.620286627174658));
#47694=CARTESIAN_POINT('Ctrl Pts',(0.0867395103929965,-0.00932397473154213,
-0.613958966158786));
#47695=CARTESIAN_POINT('Ctrl Pts',(0.0551217368298506,0.0676185869186267,
-0.607631305142914));
#47696=CARTESIAN_POINT('Ctrl Pts',(-0.0266142545750163,0.0830804466852906,
-0.601303644127043));
#47697=CARTESIAN_POINT('Ctrl Pts',(-0.0841518247181762,0.0230032511748356,
-0.59497598311117));
#47698=CARTESIAN_POINT('Ctrl Pts',(-0.0651762128470871,-0.0579891407672368,
-0.588648322095299));
#47699=CARTESIAN_POINT('Ctrl Pts',(0.013059426400348,-0.0862561913725913,
-0.582320661079426));
#47700=CARTESIAN_POINT('Ctrl Pts',(0.0794210715600979,-0.0360967112110921,
-0.575993000063554));
#47701=CARTESIAN_POINT('Ctrl Pts',(0.0735708671919806,0.046882903799052,
-0.569665339047683));
#47702=CARTESIAN_POINT('Ctrl Pts',(0.000827981990642192,0.087235277347151,
-0.56333767803181));
#47703=CARTESIAN_POINT('Ctrl Pts',(-0.0726677274895124,0.0482709079003198,
-0.55701001701594));
#47704=CARTESIAN_POINT('Ctrl Pts',(-0.0800919158994181,-0.0345827149826577,
-0.550682356000065));
#47705=CARTESIAN_POINT('Ctrl Pts',(-0.0146943044302958,-0.0859927705410227,
-0.544354694984196));
#47706=CARTESIAN_POINT('Ctrl Pts',(0.0640637777501068,-0.0592158048868383,
-0.538027033968322));
#47707=CARTESIAN_POINT('Ctrl Pts',(0.0845732895170916,0.0214018192747577,
-0.531699372952452));
#47708=CARTESIAN_POINT('Ctrl Pts',(0.0281864117401041,0.0825603134758373,
-0.525371711936578));
#47709=CARTESIAN_POINT('Ctrl Pts',(-0.0538283363655626,0.0686526719955389,
-0.519044050920707));
#47710=CARTESIAN_POINT('Ctrl Pts',(-0.0869008623428846,-0.00767589031150163,
-0.512716389904835));
#47711=CARTESIAN_POINT('Ctrl Pts',(-0.0409607047580388,-0.077025319432872,
-0.506388728888963));
#47712=CARTESIAN_POINT('Ctrl Pts',(0.0422220660331108,-0.0763411835637019,
-0.500061067873091));
#47713=CARTESIAN_POINT('Ctrl Pts',(0.0870153588274602,-0.00624551808415768,
-0.49373340685722));
#47714=CARTESIAN_POINT('Ctrl Pts',(0.0526918646680198,0.0695287463271004,
-0.487405745841347));
#47715=CARTESIAN_POINT('Ctrl Pts',(-0.0295405399103716,0.082085538737435,
-0.481078084825476));
#47716=CARTESIAN_POINT('Ctrl Pts',(-0.0849138631256316,0.0200078738773684,
-0.474750423809603));
#47717=CARTESIAN_POINT('Ctrl Pts',(-0.0630811377896817,-0.0602615069772603,
-0.468422762793731));
#47718=CARTESIAN_POINT('Ctrl Pts',(0.0161067143487094,-0.0857394478691125,
-0.46209510177786));
#47719=CARTESIAN_POINT('Ctrl Pts',(0.0806498933532556,-0.0332606955748025,
-0.455767440761988));
#47720=CARTESIAN_POINT('Ctrl Pts',(0.0718639438423683,0.049459607190435,
-0.449439779746115));
#47721=CARTESIAN_POINT('Ctrl Pts',(-0.00226270426759789,0.0872098580288294,
-0.443112118730244));
#47722=CARTESIAN_POINT('Ctrl Pts',(-0.0743320386585697,0.0456664778242435,
-0.436784457714372));
#47723=CARTESIAN_POINT('Ctrl Pts',(-0.0788166139261316,-0.0373981354779928,
-0.4304567966985));
#47724=CARTESIAN_POINT('Ctrl Pts',(-0.0116389293761198,-0.0864593227534712,
-0.424129135682628));
#47725=CARTESIAN_POINT('Ctrl Pts',(0.0661211938172418,-0.0569092865549545,
-0.417801474666756));
#47726=CARTESIAN_POINT('Ctrl Pts',(0.0837620866257479,0.0243842574648459,
-0.411473813650883));
#47727=CARTESIAN_POINT('Ctrl Pts',(0.0252441581448469,0.0835069556837582,
-0.405146152635012));
#47728=CARTESIAN_POINT('Ctrl Pts',(-0.0562264617768135,0.066702804769153,
-0.398818491619139));
#47729=CARTESIAN_POINT('Ctrl Pts',(-0.0865744171768889,-0.010749393401173,
-0.392490830603268));
#47730=CARTESIAN_POINT('Ctrl Pts',(-0.0382065020487046,-0.0784279438032996,
-0.386163169587396));
#47731=CARTESIAN_POINT('Ctrl Pts',(0.0448998284991146,-0.0747976240850022,
-0.379835508571524));
#47732=CARTESIAN_POINT('Ctrl Pts',(0.0871819848609725,-0.00315922201061306,
-0.373507847555652));
#47733=CARTESIAN_POINT('Ctrl Pts',(0.0501958532401191,0.0713516326758373,
-0.36718018653978));
#47734=CARTESIAN_POINT('Ctrl Pts',(-0.0324297457147349,0.0809875963397409,
-0.360852525523908));
#47735=CARTESIAN_POINT('Ctrl Pts',(-0.0855693169469914,0.0169873825304703,
-0.354524864508036));
#47736=CARTESIAN_POINT('Ctrl Pts',(-0.0609068827643145,-0.0624582324433317,
-0.348197203492164));
#47737=CARTESIAN_POINT('Ctrl Pts',(0.019133785015476,-0.0851150834987123,
-0.341869542476292));
#47738=CARTESIAN_POINT('Ctrl Pts',(0.0817774827305826,-0.030382930837239,
-0.33554188146042));
#47739=CARTESIAN_POINT('Ctrl Pts',(0.0700668162737063,0.0519742284721753,
-0.329214220444548));
#47740=CARTESIAN_POINT('Ctrl Pts',(-0.00535055036065351,0.0870749721725439,
-0.322886559428676));
#47741=CARTESIAN_POINT('Ctrl Pts',(-0.0759030476354704,0.0430047268059999,
-0.316558898412805));
#47742=CARTESIAN_POINT('Ctrl Pts',(-0.0774423806845742,-0.0401666135231323,
-0.310231237396932));
#47743=CARTESIAN_POINT('Ctrl Pts',(-0.00856894504114455,-0.0868173505060656,
-0.303903576381061));
#47744=CARTESIAN_POINT('Ctrl Pts',(0.0680956140128458,-0.0545313352140282,
-0.297575915365189));
#47745=CARTESIAN_POINT('Ctrl Pts',(0.0828457448677347,0.0273360883324843,
-0.291248254349316));
#47746=CARTESIAN_POINT('Ctrl Pts',(0.0222702178726658,0.0843487792674867,
-0.284920593333445));
#47747=CARTESIAN_POINT('Ctrl Pts',(-0.0585540112663533,0.0646692116283394,
-0.278592932317572));
#47748=CARTESIAN_POINT('Ctrl Pts',(-0.0861393030835636,-0.0138094037629872,
-0.272265271301701));
#47749=CARTESIAN_POINT('Ctrl Pts',(-0.0354043422207423,-0.0797321247674219,
-0.265937610285828));
#47750=CARTESIAN_POINT('Ctrl Pts',(0.0475212323275497,-0.0731601780074524,
-0.259609949269957));
#47751=CARTESIAN_POINT('Ctrl Pts',(0.0872391793431545,-6.89604553678452E-5,
-0.253282288254085));
#47752=CARTESIAN_POINT('Ctrl Pts',(0.0476368355604161,0.0730849578627569,
-0.246954627238213));
#47753=CARTESIAN_POINT('Ctrl Pts',(-0.035278245432985,0.0797879976386212,
-0.240626966222341));
#47754=CARTESIAN_POINT('Ctrl Pts',(-0.0861173634511866,0.0139455684799636,
-0.234299305206469));
#47755=CARTESIAN_POINT('Ctrl Pts',(-0.0586561769139268,-0.0645765598174114,
-0.227971644190597));
#47756=CARTESIAN_POINT('Ctrl Pts',(0.0221368387963713,-0.0843838819687206,
-0.221643983174725));
#47757=CARTESIAN_POINT('Ctrl Pts',(0.0828024243326025,-0.0274670291926198,
-0.215316322158853));
#47758=CARTESIAN_POINT('Ctrl Pts',(0.0681817402553036,0.0544236112708011,
-0.208988661142981));
#47759=CARTESIAN_POINT('Ctrl Pts',(-0.00843168039820402,0.0868307890880593,
-0.202661000127109));
#47760=CARTESIAN_POINT('Ctrl Pts',(-0.0773787824772003,0.0402889958977259,
-0.196333339111237));
#47761=CARTESIAN_POINT('Ctrl Pts',(-0.0759709411227765,-0.042884674101741,
-0.190005678095365));
#47762=CARTESIAN_POINT('Ctrl Pts',(-0.00548820489699097,-0.0870664043988389,
-0.183678017079493));
#47763=CARTESIAN_POINT('Ctrl Pts',(0.0699845600316936,-0.0520849356893883,
-0.177350356063621));
#47764=CARTESIAN_POINT('Ctrl Pts',(0.0818254144363875,0.0302536067170679,
-0.17102269504775));
#47765=CARTESIAN_POINT('Ctrl Pts',(0.0192683238503164,0.0850847275592565,
-0.164695034031877));
#47766=CARTESIAN_POINT('Ctrl Pts',(-0.0608080632979376,0.0625544451633288,
-0.158367373016005));
#47767=CARTESIAN_POINT('Ctrl Pts',(-0.0855960661777222,-0.0168520804602516,
-0.152039712000134));
#47768=CARTESIAN_POINT('Ctrl Pts',(-0.0325577426519127,-0.0809362252804344,
-0.145712050984262));
#47769=CARTESIAN_POINT('Ctrl Pts',(0.0500829872689032,-0.0714309007163379,
-0.139384389968389));
#47770=CARTESIAN_POINT('Ctrl Pts',(0.0871868701826791,0.00302138775326442,
-0.133056728952518));
#47771=CARTESIAN_POINT('Ctrl Pts',(0.0450180242988335,0.0747265460260562,
-0.126729067936645));
#47772=CARTESIAN_POINT('Ctrl Pts',(-0.0380824646851997,0.0784882487172661,
-0.120401406920774));
#47773=CARTESIAN_POINT('Ctrl Pts',(-0.0865573126760457,0.0108862491969944,
-0.114073745904902));
#47774=CARTESIAN_POINT('Ctrl Pts',(-0.056331849230979,-0.0666138289451202,
-0.10774608488903));
#47775=CARTESIAN_POINT('Ctrl Pts',(0.0251121136077328,-0.0835467633888102,
-0.101418423873158));
#47776=CARTESIAN_POINT('Ctrl Pts',(0.0837234176563311,-0.0245166463433077,
-0.0950907628572859));
#47777=CARTESIAN_POINT('Ctrl Pts',(0.0662111084823356,0.0568046728275819,
-0.0887631018414139));
#47778=CARTESIAN_POINT('Ctrl Pts',(-0.0115022772465146,0.0864776309684878,
-0.0824354408255419));
#47779=CARTESIAN_POINT('Ctrl Pts',(-0.0787572953699165,0.0375226641418117,
-0.07610777980967));
#47780=CARTESIAN_POINT('Ctrl Pts',(-0.0744043232715852,-0.0455488490220237,
-0.069780118793798));
#47781=CARTESIAN_POINT('Ctrl Pts',(-0.00240023246381204,-0.0872062789102198,
-0.0634524577779261));
#47782=CARTESIAN_POINT('Ctrl Pts',(0.071785009393588,-0.0495729555872598,
-0.057124796762054));
#47783=CARTESIAN_POINT('Ctrl Pts',(0.0807036117542888,0.033132765216591,
-0.050797135746182));
#47784=CARTESIAN_POINT('Ctrl Pts',(0.0162399001827532,0.0857146076576825,
-0.0444694747303104));
#47785=CARTESIAN_POINT('Ctrl Pts',(-0.0629813424607405,0.0603597734414823,
-0.0381418137144381));
#47786=CARTESIAN_POINT('Ctrl Pts',(-0.0849538233030444,-0.0198709737859279,
-0.0318141526985663));
#47787=CARTESIAN_POINT('Ctrl Pts',(-0.0296542637309572,-0.082043730023256,
-0.0254864916826941));
#47788=CARTESIAN_POINT('Ctrl Pts',(0.0525513937314469,-0.0696024314386667,
-0.0191588306668225));
#47789=CARTESIAN_POINT('Ctrl Pts',(0.0870838812505578,0.006089403235341,
-0.0128311696509503));
#47790=CARTESIAN_POINT('Ctrl Pts',(0.0422233970601371,0.0763133360679174,
-0.00650350863507852));
#47791=CARTESIAN_POINT('Ctrl Pts',(-0.0129586834061405,0.0767643115864734,
-0.00228506795783038));
#47792=CARTESIAN_POINT('Ctrl Pts',(-0.0345944601705113,0.0653026287794826,
-0.000175847619206415));
#47793=CARTESIAN_POINT('Ctrl Pts',(-0.0452560140322624,0.0854280329804664,
-0.013325));
#47794=CARTESIAN_POINT('Ctrl Pts',(-0.0169523777846916,0.100422054433319,
-0.0154342203386239));
#47795=CARTESIAN_POINT('Ctrl Pts',(0.0191418551589967,0.100127074336862,
-0.0175434406772479));
#47796=CARTESIAN_POINT('Ctrl Pts',(0.0469699533834549,0.0846685813418844,
-0.0196526610158718));
#47797=CARTESIAN_POINT('Ctrl Pts',(0.0747980516079155,0.0692100883469053,
-0.0217618813544959));
#47798=CARTESIAN_POINT('Ctrl Pts',(0.0943600151131444,0.0385880824534022,
-0.0238711016931199));
#47799=CARTESIAN_POINT('Ctrl Pts',(0.0966118398271697,0.00677390378019592,
-0.025980322031744));
#47800=CARTESIAN_POINT('Ctrl Pts',(0.0988636645411949,-0.0250402748930086,
-0.028089542370368));
#47801=CARTESIAN_POINT('Ctrl Pts',(0.0838053504640186,-0.0580466263459162,
-0.030198762708992));
#47802=CARTESIAN_POINT('Ctrl Pts',(0.0583528016004915,-0.0772623923760804,
-0.032307983047616));
#47803=CARTESIAN_POINT('Ctrl Pts',(0.0329002527369644,-0.0964781584062447,
-0.03441720338624));
#47804=CARTESIAN_POINT('Ctrl Pts',(-0.00294653091291341,-0.101903339013666,
-0.0365264237248639));
#47805=CARTESIAN_POINT('Ctrl Pts',(-0.0329269478204673,-0.0910603334462807,
-0.0386356440634878));
#47806=CARTESIAN_POINT('Ctrl Pts',(-0.0629073647280212,-0.0802173278788959,
-0.0407448644021118));
#47807=CARTESIAN_POINT('Ctrl Pts',(-0.0870214148932512,-0.0531061361367054,
-0.0428540847407358));
#47808=CARTESIAN_POINT('Ctrl Pts',(-0.0942877552996606,-0.0220577403373066,
-0.0449633050793598));
#47809=CARTESIAN_POINT('Ctrl Pts',(-0.0959679031622562,-0.014878625002527,
-0.0454510061565838));
#47810=CARTESIAN_POINT('Ctrl Pts',(-0.0967473007548937,-0.00748900998154789,
-0.0459387072338078));
#47811=CARTESIAN_POINT('Ctrl Pts',(-0.0966799176497682,-8.54770466914428E-5,
-0.0464264083110319));
#47812=CARTESIAN_POINT('Origin',(0.194007127343405,-0.0342086910003853,
0.04));
#47813=CARTESIAN_POINT('',(0.18738691397118,-0.0314029373205391,0.04));
#47814=CARTESIAN_POINT('',(0.186826537413779,-0.0345809907026646,0.04));
#47815=CARTESIAN_POINT('Origin',(0.,0.,0.04));
#47816=CARTESIAN_POINT('',(0.181204626554246,-0.0319512646907152,0.04));
#47817=CARTESIAN_POINT('',(0.208025165376232,-0.02957246303897,0.04));
#47818=CARTESIAN_POINT('',(0.181204626554246,-0.0319512646907152,0.04));
#47819=CARTESIAN_POINT('Origin',(0.181204626554246,-0.0319512646907152,
0.04));
#47820=CARTESIAN_POINT('',(0.186826537413779,-0.0345809907026646,0.185));
#47821=CARTESIAN_POINT('',(0.186826537413779,-0.0345809907026646,0.0925));
#47822=CARTESIAN_POINT('',(0.181204626554246,-0.0319512646907152,0.191));
#47823=CARTESIAN_POINT('',(0.181204626554246,-0.0319512646907152,0.04));
#47824=CARTESIAN_POINT('Ctrl Pts',(0.186826537413779,-0.0345809907026646,
0.185));
#47825=CARTESIAN_POINT('Ctrl Pts',(0.183970486442383,-0.033245033637782,
0.188051499118437));
#47826=CARTESIAN_POINT('Ctrl Pts',(0.181204626554246,-0.0319512646907152,
0.191));
#47827=CARTESIAN_POINT('Origin',(0.208025165376232,-0.02957246303897,0.04));
#47828=CARTESIAN_POINT('',(0.18738691397118,-0.0314029373205391,0.185));
#47829=CARTESIAN_POINT('',(0.18738691397118,-0.0314029373205391,0.0925));
#47830=CARTESIAN_POINT('Ctrl Pts',(0.181204626554246,-0.0319512646907152,
0.191));
#47831=CARTESIAN_POINT('Ctrl Pts',(0.18424617972193,-0.0316814993535168,
0.188051499118469));
#47832=CARTESIAN_POINT('Ctrl Pts',(0.18738691397118,-0.0314029373205392,
0.185));
#47833=CARTESIAN_POINT('Origin',(0.185119446294824,-0.0673779682351569,
0.04));
#47834=CARTESIAN_POINT('',(0.179087022852749,-0.0634652522703487,0.04));
#47835=CARTESIAN_POINT('',(0.17798329649608,-0.0664977155125527,0.04));
#47836=CARTESIAN_POINT('Origin',(0.,0.,0.04));
#47837=CARTESIAN_POINT('',(0.172903442224607,-0.0629317063719232,0.04));
#47838=CARTESIAN_POINT('',(0.19972959136832,-0.0652463817528892,0.04));
#47839=CARTESIAN_POINT('',(0.172903442224607,-0.0629317063719232,0.04));
#47840=CARTESIAN_POINT('Origin',(0.172903442224607,-0.0629317063719232,
0.04));
#47841=CARTESIAN_POINT('',(0.17798329649608,-0.0664977155125527,0.185));
#47842=CARTESIAN_POINT('',(0.17798329649608,-0.0664977155125527,0.0925));
#47843=CARTESIAN_POINT('',(0.172903442224607,-0.0629317063719232,0.191));
#47844=CARTESIAN_POINT('',(0.172903442224607,-0.0629317063719232,0.04));
#47845=CARTESIAN_POINT('Ctrl Pts',(0.17798329649608,-0.0664977155125527,
0.185));
#47846=CARTESIAN_POINT('Ctrl Pts',(0.17540262186618,-0.0646861065908373,
0.188051499118472));
#47847=CARTESIAN_POINT('Ctrl Pts',(0.172903442224607,-0.0629317063719232,
0.191));
#47848=CARTESIAN_POINT('Origin',(0.19972959136832,-0.0652463817528892,0.04));
#47849=CARTESIAN_POINT('',(0.179087022852749,-0.0634652522703487,0.185));
#47850=CARTESIAN_POINT('',(0.179087022852749,-0.0634652522703487,0.0925));
#47851=CARTESIAN_POINT('Ctrl Pts',(0.172903442224607,-0.0629317063719232,
0.191));
#47852=CARTESIAN_POINT('Ctrl Pts',(0.17594563162456,-0.063194199541203,
0.188051499118452));
#47853=CARTESIAN_POINT('Ctrl Pts',(0.179087022852749,-0.0634652522703487,
0.185));
#47854=CARTESIAN_POINT('Origin',(0.170607004545534,-0.0985000000000001,
0.04));
#47855=CARTESIAN_POINT('',(0.165345663167344,-0.0935992076448907,0.04));
#47856=CARTESIAN_POINT('',(0.163732123178242,-0.0963939408860593,0.04));
#47857=CARTESIAN_POINT('Origin',(0.,0.,0.04));
#47858=CARTESIAN_POINT('',(0.159348674296337,-0.0920000000000001,0.04));
#47859=CARTESIAN_POINT('',(0.185365334794732,-0.098937822173509,0.04));
#47860=CARTESIAN_POINT('',(0.159348674296337,-0.0920000000000001,0.04));
#47861=CARTESIAN_POINT('Origin',(0.159348674296337,-0.0920000000000001,
0.04));
#47862=CARTESIAN_POINT('',(0.163732123178242,-0.0963939408860593,0.185));
#47863=CARTESIAN_POINT('',(0.163732123178242,-0.0963939408860593,0.0925));
#47864=CARTESIAN_POINT('',(0.159348674296337,-0.0920000000000001,0.191));
#47865=CARTESIAN_POINT('',(0.159348674296337,-0.0920000000000001,0.04));
#47866=CARTESIAN_POINT('Ctrl Pts',(0.163732123178242,-0.0963939408860593,
0.185));
#47867=CARTESIAN_POINT('Ctrl Pts',(0.161505237382642,-0.0941617249279212,
0.188051499118436));
#47868=CARTESIAN_POINT('Ctrl Pts',(0.159348674296337,-0.0920000000000001,
0.191));
#47869=CARTESIAN_POINT('Origin',(0.185365334794732,-0.098937822173509,0.04));
#47870=CARTESIAN_POINT('',(0.165345663167344,-0.0935992076448907,0.185));
#47871=CARTESIAN_POINT('',(0.165345663167344,-0.0935992076448907,0.0925));
#47872=CARTESIAN_POINT('Ctrl Pts',(0.159348674296337,-0.0920000000000001,
0.191));
#47873=CARTESIAN_POINT('Ctrl Pts',(0.162299064543036,-0.0927867759536363,
0.188051499118462));
#47874=CARTESIAN_POINT('Ctrl Pts',(0.165345663167344,-0.0935992076448907,
0.185));
#47875=CARTESIAN_POINT('Origin',(0.150910755294439,-0.126629159108248,0.04));
#47876=CARTESIAN_POINT('',(0.146580359175541,-0.120889198458627,0.04));
#47877=CARTESIAN_POINT('',(0.144506032150084,-0.123361285143431,0.04));
#47878=CARTESIAN_POINT('Origin',(0.,0.,0.04));
#47879=CARTESIAN_POINT('',(0.140952177533892,-0.118272920182323,0.04));
#47880=CARTESIAN_POINT('',(0.165368846322791,-0.129623086932341,0.04));
#47881=CARTESIAN_POINT('',(0.140952177533892,-0.118272920182323,0.04));
#47882=CARTESIAN_POINT('Origin',(0.140952177533892,-0.118272920182323,0.04));
#47883=CARTESIAN_POINT('',(0.144506032150084,-0.123361285143431,0.185));
#47884=CARTESIAN_POINT('',(0.144506032150084,-0.123361285143431,0.0925));
#47885=CARTESIAN_POINT('',(0.140952177533892,-0.118272920182323,0.191));
#47886=CARTESIAN_POINT('',(0.140952177533892,-0.118272920182323,0.04));
#47887=CARTESIAN_POINT('Ctrl Pts',(0.144506032150084,-0.123361285143431,
0.185));
#47888=CARTESIAN_POINT('Ctrl Pts',(0.1427005979868,-0.120776286901188,0.188051499118426));
#47889=CARTESIAN_POINT('Ctrl Pts',(0.140952177533892,-0.118272920182323,
0.191));
#47890=CARTESIAN_POINT('Origin',(0.165368846322791,-0.129623086932341,0.04));
#47891=CARTESIAN_POINT('',(0.146580359175541,-0.120889198458627,0.185));
#47892=CARTESIAN_POINT('',(0.146580359175541,-0.120889198458627,0.0925));
#47893=CARTESIAN_POINT('Ctrl Pts',(0.140952177533892,-0.118272920182323,
0.191));
#47894=CARTESIAN_POINT('Ctrl Pts',(0.143721122512686,-0.1195600731311,0.188051499118447));
#47895=CARTESIAN_POINT('Ctrl Pts',(0.146580359175541,-0.120889198458627,
0.185));
#47896=CARTESIAN_POINT('Origin',(0.126629159108248,-0.150910755294439,0.04));
#47897=CARTESIAN_POINT('',(0.123361285143431,-0.144506032150084,0.04));
#47898=CARTESIAN_POINT('',(0.120889198458627,-0.146580359175541,0.04));
#47899=CARTESIAN_POINT('Origin',(0.,0.,0.04));
#47900=CARTESIAN_POINT('',(0.118272920182323,-0.140952177533892,0.04));
#47901=CARTESIAN_POINT('',(0.140347709136006,-0.15636981978718,0.04));
#47902=CARTESIAN_POINT('',(0.118272920182323,-0.140952177533892,0.04));
#47903=CARTESIAN_POINT('Origin',(0.118272920182323,-0.140952177533892,0.04));
#47904=CARTESIAN_POINT('',(0.120889198458627,-0.146580359175541,0.185));
#47905=CARTESIAN_POINT('',(0.120889198458627,-0.146580359175541,0.0925));
#47906=CARTESIAN_POINT('',(0.118272920182323,-0.140952177533892,0.191));
#47907=CARTESIAN_POINT('',(0.118272920182323,-0.140952177533892,0.04));
#47908=CARTESIAN_POINT('Ctrl Pts',(0.120889198458627,-0.146580359175541,
0.185));
#47909=CARTESIAN_POINT('Ctrl Pts',(0.119560073131107,-0.143721122512702,
0.18805149911843));
#47910=CARTESIAN_POINT('Ctrl Pts',(0.118272920182323,-0.140952177533892,
0.191));
#47911=CARTESIAN_POINT('Origin',(0.140347709136006,-0.15636981978718,0.04));
#47912=CARTESIAN_POINT('',(0.123361285143431,-0.144506032150084,0.185));
#47913=CARTESIAN_POINT('',(0.123361285143431,-0.144506032150084,0.0925));
#47914=CARTESIAN_POINT('Ctrl Pts',(0.118272920182323,-0.140952177533892,
0.191));
#47915=CARTESIAN_POINT('Ctrl Pts',(0.120776286901169,-0.142700597986787,
0.188051499118449));
#47916=CARTESIAN_POINT('Ctrl Pts',(0.123361285143431,-0.144506032150084,
0.185));
#47917=CARTESIAN_POINT('Origin',(0.0985,-0.170607004545534,0.04));
#47918=CARTESIAN_POINT('',(0.0963939408860592,-0.163732123178242,0.04));
#47919=CARTESIAN_POINT('',(0.0935992076448907,-0.165345663167344,0.04));
#47920=CARTESIAN_POINT('Origin',(0.,0.,0.04));
#47921=CARTESIAN_POINT('',(0.092,-0.159348674296337,0.04));
#47922=CARTESIAN_POINT('',(0.111062177826491,-0.178365334794732,0.04));
#47923=CARTESIAN_POINT('',(0.092,-0.159348674296337,0.04));
#47924=CARTESIAN_POINT('Origin',(0.092,-0.159348674296337,0.04));
#47925=CARTESIAN_POINT('',(0.0935992076448907,-0.165345663167344,0.185));
#47926=CARTESIAN_POINT('',(0.0935992076448907,-0.165345663167344,0.0925));
#47927=CARTESIAN_POINT('',(0.092,-0.159348674296337,0.191));
#47928=CARTESIAN_POINT('',(0.092,-0.159348674296337,0.04));
#47929=CARTESIAN_POINT('Ctrl Pts',(0.0935992076448907,-0.165345663167344,
0.185));
#47930=CARTESIAN_POINT('Ctrl Pts',(0.0927867759536364,-0.162299064543037,
0.188051499118462));
#47931=CARTESIAN_POINT('Ctrl Pts',(0.092,-0.159348674296337,0.191));
#47932=CARTESIAN_POINT('Origin',(0.111062177826491,-0.178365334794732,0.04));
#47933=CARTESIAN_POINT('',(0.0963939408860592,-0.163732123178242,0.185));
#47934=CARTESIAN_POINT('',(0.0963939408860592,-0.163732123178242,0.0925));
#47935=CARTESIAN_POINT('Ctrl Pts',(0.092,-0.159348674296337,0.191));
#47936=CARTESIAN_POINT('Ctrl Pts',(0.0941617249279249,-0.161505237382646,
0.18805149911843));
#47937=CARTESIAN_POINT('Ctrl Pts',(0.0963939408860592,-0.163732123178242,
0.185));
#47938=CARTESIAN_POINT('Origin',(0.0673779682351567,-0.185119446294824,
0.04));
#47939=CARTESIAN_POINT('',(0.0664977155125524,-0.17798329649608,0.04));
#47940=CARTESIAN_POINT('',(0.0634652522703484,-0.179087022852749,0.04));
#47941=CARTESIAN_POINT('Origin',(0.,0.,0.04));
#47942=CARTESIAN_POINT('',(0.062931706371923,-0.172903442224607,0.04));
#47943=CARTESIAN_POINT('',(0.0784020784438917,-0.194941309361761,0.04));
#47944=CARTESIAN_POINT('',(0.062931706371923,-0.172903442224607,0.04));
#47945=CARTESIAN_POINT('Origin',(0.062931706371923,-0.172903442224607,0.04));
#47946=CARTESIAN_POINT('',(0.0634652522703484,-0.179087022852749,0.185));
#47947=CARTESIAN_POINT('',(0.0634652522703484,-0.179087022852749,0.0925));
#47948=CARTESIAN_POINT('',(0.062931706371923,-0.172903442224607,0.191));
#47949=CARTESIAN_POINT('',(0.062931706371923,-0.172903442224607,0.04));
#47950=CARTESIAN_POINT('Ctrl Pts',(0.0634652522703485,-0.179087022852749,
0.185));
#47951=CARTESIAN_POINT('Ctrl Pts',(0.0631941995412026,-0.175945631624558,
0.188051499118454));
#47952=CARTESIAN_POINT('Ctrl Pts',(0.062931706371923,-0.172903442224607,
0.191));
#47953=CARTESIAN_POINT('Origin',(0.0784020784438917,-0.194941309361761,
0.04));
#47954=CARTESIAN_POINT('',(0.0664977155125524,-0.17798329649608,0.185));
#47955=CARTESIAN_POINT('',(0.0664977155125524,-0.17798329649608,0.0925));
#47956=CARTESIAN_POINT('Ctrl Pts',(0.062931706371923,-0.172903442224607,
0.191));
#47957=CARTESIAN_POINT('Ctrl Pts',(0.0646861065908383,-0.175402621866182,
0.18805149911847));
#47958=CARTESIAN_POINT('Ctrl Pts',(0.0664977155125524,-0.17798329649608,
0.185));
#47959=CARTESIAN_POINT('Origin',(0.0342086910003852,-0.194007127343405,
0.04));
#47960=CARTESIAN_POINT('',(0.0345809907026645,-0.186826537413779,0.04));
#47961=CARTESIAN_POINT('',(0.031402937320539,-0.18738691397118,0.04));
#47962=CARTESIAN_POINT('Origin',(0.,0.,0.04));
#47963=CARTESIAN_POINT('',(0.0319512646907151,-0.181204626554246,0.04));
#47964=CARTESIAN_POINT('',(0.0433597715811408,-0.205594090888895,0.04));
#47965=CARTESIAN_POINT('',(0.0319512646907151,-0.181204626554246,0.04));
#47966=CARTESIAN_POINT('Origin',(0.0319512646907151,-0.181204626554246,
0.04));
#47967=CARTESIAN_POINT('',(0.031402937320539,-0.18738691397118,0.185));
#47968=CARTESIAN_POINT('',(0.031402937320539,-0.18738691397118,0.0925));
#47969=CARTESIAN_POINT('',(0.0319512646907151,-0.181204626554246,0.191));
#47970=CARTESIAN_POINT('',(0.0319512646907151,-0.181204626554246,0.04));
#47971=CARTESIAN_POINT('Ctrl Pts',(0.031402937320539,-0.18738691397118,
0.185));
#47972=CARTESIAN_POINT('Ctrl Pts',(0.0316814993535159,-0.184246179721939,
0.18805149911846));
#47973=CARTESIAN_POINT('Ctrl Pts',(0.0319512646907151,-0.181204626554246,
0.191));
#47974=CARTESIAN_POINT('Origin',(0.0433597715811408,-0.205594090888895,
0.04));
#47975=CARTESIAN_POINT('',(0.0345809907026646,-0.186826537413779,0.185));
#47976=CARTESIAN_POINT('',(0.0345809907026646,-0.186826537413779,0.0925));
#47977=CARTESIAN_POINT('Ctrl Pts',(0.0319512646907151,-0.181204626554246,
0.191));
#47978=CARTESIAN_POINT('Ctrl Pts',(0.0332450336377804,-0.18397048644238,
0.188051499118441));
#47979=CARTESIAN_POINT('Ctrl Pts',(0.0345809907026645,-0.186826537413779,
0.185));
#47980=CARTESIAN_POINT('Origin',(-4.16333634234434E-17,-0.197,0.04));
#47981=CARTESIAN_POINT('',(0.00161353998910185,-0.18999314853095,0.04));
#47982=CARTESIAN_POINT('',(-0.00161353998910192,-0.18999314853095,0.04));
#47983=CARTESIAN_POINT('Origin',(0.,0.,0.04));
#47984=CARTESIAN_POINT('',(-3.46944695195361E-17,-0.184,0.04));
#47985=CARTESIAN_POINT('',(0.00699999999999997,-0.21,0.04));
#47986=CARTESIAN_POINT('',(-3.46944695195361E-17,-0.184,0.04));
#47987=CARTESIAN_POINT('Origin',(-3.46944695195361E-17,-0.184,0.04));
#47988=CARTESIAN_POINT('',(-0.00161353998910191,-0.18999314853095,0.185));
#47989=CARTESIAN_POINT('',(-0.00161353998910191,-0.18999314853095,0.0925));
#47990=CARTESIAN_POINT('',(-3.46944695195361E-17,-0.184,0.191));
#47991=CARTESIAN_POINT('',(-3.46944695195361E-17,-0.184,0.04));
#47992=CARTESIAN_POINT('Ctrl Pts',(-0.0016135399891019,-0.18999314853095,
0.185));
#47993=CARTESIAN_POINT('Ctrl Pts',(-0.000793827160417415,-0.18694850088155,
0.18805149911845));
#47994=CARTESIAN_POINT('Ctrl Pts',(-3.46944695195361E-17,-0.184,0.191));
#47995=CARTESIAN_POINT('Origin',(0.00699999999999997,-0.21,0.04));
#47996=CARTESIAN_POINT('',(0.00161353998910184,-0.18999314853095,0.185));
#47997=CARTESIAN_POINT('',(0.00161353998910184,-0.18999314853095,0.0925));
#47998=CARTESIAN_POINT('Ctrl Pts',(-3.46944695195361E-17,-0.184,0.191));
#47999=CARTESIAN_POINT('Ctrl Pts',(0.000793827160417323,-0.18694850088155,
0.18805149911845));
#48000=CARTESIAN_POINT('Ctrl Pts',(0.00161353998910184,-0.18999314853095,
0.185));
#48001=CARTESIAN_POINT('Origin',(-0.0342086910003853,-0.194007127343405,
0.04));
#48002=CARTESIAN_POINT('',(-0.0314029373205391,-0.18738691397118,0.04));
#48003=CARTESIAN_POINT('',(-0.0345809907026646,-0.186826537413779,0.04));
#48004=CARTESIAN_POINT('Origin',(0.,0.,0.04));
#48005=CARTESIAN_POINT('',(-0.0319512646907152,-0.181204626554246,0.04));
#48006=CARTESIAN_POINT('',(-0.0295724630389699,-0.208025165376232,0.04));
#48007=CARTESIAN_POINT('',(-0.0319512646907152,-0.181204626554246,0.04));
#48008=CARTESIAN_POINT('Origin',(-0.0319512646907152,-0.181204626554246,
0.04));
#48009=CARTESIAN_POINT('',(-0.0345809907026646,-0.186826537413779,0.185));
#48010=CARTESIAN_POINT('',(-0.0345809907026646,-0.186826537413779,0.0925));
#48011=CARTESIAN_POINT('',(-0.0319512646907152,-0.181204626554246,0.191));
#48012=CARTESIAN_POINT('',(-0.0319512646907152,-0.181204626554246,0.04));
#48013=CARTESIAN_POINT('Ctrl Pts',(-0.0345809907026646,-0.186826537413779,
0.185));
#48014=CARTESIAN_POINT('Ctrl Pts',(-0.033245033637776,-0.18397048644237,
0.188051499118451));
#48015=CARTESIAN_POINT('Ctrl Pts',(-0.0319512646907152,-0.181204626554246,
0.191));
#48016=CARTESIAN_POINT('Origin',(-0.0295724630389699,-0.208025165376232,
0.04));
#48017=CARTESIAN_POINT('',(-0.0314029373205391,-0.18738691397118,0.185));
#48018=CARTESIAN_POINT('',(-0.0314029373205391,-0.18738691397118,0.0925));
#48019=CARTESIAN_POINT('Ctrl Pts',(-0.0319512646907152,-0.181204626554246,
0.191));
#48020=CARTESIAN_POINT('Ctrl Pts',(-0.0316814993535157,-0.184246179721942,
0.188051499118457));
#48021=CARTESIAN_POINT('Ctrl Pts',(-0.0314029373205391,-0.18738691397118,
0.185));
#48022=CARTESIAN_POINT('Origin',(-0.0673779682351569,-0.185119446294824,
0.04));
#48023=CARTESIAN_POINT('',(-0.0634652522703487,-0.179087022852749,0.04));
#48024=CARTESIAN_POINT('',(-0.0664977155125527,-0.17798329649608,0.04));
#48025=CARTESIAN_POINT('Origin',(0.,0.,0.04));
#48026=CARTESIAN_POINT('',(-0.0629317063719232,-0.172903442224607,0.04));
#48027=CARTESIAN_POINT('',(-0.0652463817528892,-0.19972959136832,0.04));
#48028=CARTESIAN_POINT('',(-0.0629317063719232,-0.172903442224607,0.04));
#48029=CARTESIAN_POINT('Origin',(-0.0629317063719232,-0.172903442224607,
0.04));
#48030=CARTESIAN_POINT('',(-0.0664977155125527,-0.17798329649608,0.185));
#48031=CARTESIAN_POINT('',(-0.0664977155125527,-0.17798329649608,0.0925));
#48032=CARTESIAN_POINT('',(-0.0629317063719232,-0.172903442224607,0.191));
#48033=CARTESIAN_POINT('',(-0.0629317063719232,-0.172903442224607,0.04));
#48034=CARTESIAN_POINT('Ctrl Pts',(-0.0664977155125527,-0.17798329649608,
0.185));
#48035=CARTESIAN_POINT('Ctrl Pts',(-0.0646861065908368,-0.175402621866179,
0.188051499118473));
#48036=CARTESIAN_POINT('Ctrl Pts',(-0.0629317063719232,-0.172903442224607,
0.191));
#48037=CARTESIAN_POINT('Origin',(-0.0652463817528892,-0.19972959136832,
0.04));
#48038=CARTESIAN_POINT('',(-0.0634652522703487,-0.179087022852749,0.185));
#48039=CARTESIAN_POINT('',(-0.0634652522703487,-0.179087022852749,0.0925));
#48040=CARTESIAN_POINT('Ctrl Pts',(-0.0629317063719232,-0.172903442224607,
0.191));
#48041=CARTESIAN_POINT('Ctrl Pts',(-0.0631941995412029,-0.175945631624558,
0.188051499118454));
#48042=CARTESIAN_POINT('Ctrl Pts',(-0.0634652522703487,-0.179087022852749,
0.185));
#48043=CARTESIAN_POINT('Origin',(-0.0985000000000001,-0.170607004545534,
0.04));
#48044=CARTESIAN_POINT('',(-0.0935992076448907,-0.165345663167344,0.04));
#48045=CARTESIAN_POINT('',(-0.0963939408860593,-0.163732123178242,0.04));
#48046=CARTESIAN_POINT('Origin',(0.,0.,0.04));
#48047=CARTESIAN_POINT('',(-0.0920000000000001,-0.159348674296337,0.04));
#48048=CARTESIAN_POINT('',(-0.098937822173509,-0.185365334794732,0.04));
#48049=CARTESIAN_POINT('',(-0.0920000000000001,-0.159348674296337,0.04));
#48050=CARTESIAN_POINT('Origin',(-0.0920000000000001,-0.159348674296337,
0.04));
#48051=CARTESIAN_POINT('',(-0.0963939408860593,-0.163732123178242,0.185));
#48052=CARTESIAN_POINT('',(-0.0963939408860593,-0.163732123178242,0.0925));
#48053=CARTESIAN_POINT('',(-0.0920000000000001,-0.159348674296337,0.191));
#48054=CARTESIAN_POINT('',(-0.0920000000000001,-0.159348674296337,0.04));
#48055=CARTESIAN_POINT('Ctrl Pts',(-0.0963939408860593,-0.163732123178242,
0.185));
#48056=CARTESIAN_POINT('Ctrl Pts',(-0.0941617249279212,-0.161505237382642,
0.188051499118436));
#48057=CARTESIAN_POINT('Ctrl Pts',(-0.0920000000000001,-0.159348674296337,
0.191));
#48058=CARTESIAN_POINT('Origin',(-0.098937822173509,-0.185365334794732,
0.04));
#48059=CARTESIAN_POINT('',(-0.0935992076448907,-0.165345663167344,0.185));
#48060=CARTESIAN_POINT('',(-0.0935992076448907,-0.165345663167344,0.0925));
#48061=CARTESIAN_POINT('Ctrl Pts',(-0.0920000000000001,-0.159348674296337,
0.191));
#48062=CARTESIAN_POINT('Ctrl Pts',(-0.0927867759536363,-0.162299064543036,
0.188051499118462));
#48063=CARTESIAN_POINT('Ctrl Pts',(-0.0935992076448907,-0.165345663167344,
0.185));
#48064=CARTESIAN_POINT('Origin',(-0.126629159108248,-0.150910755294439,
0.04));
#48065=CARTESIAN_POINT('',(-0.120889198458627,-0.146580359175541,0.04));
#48066=CARTESIAN_POINT('',(-0.123361285143431,-0.144506032150084,0.04));
#48067=CARTESIAN_POINT('Origin',(0.,0.,0.04));
#48068=CARTESIAN_POINT('',(-0.118272920182323,-0.140952177533892,0.04));
#48069=CARTESIAN_POINT('',(-0.12962308693234,-0.165368846322791,0.04));
#48070=CARTESIAN_POINT('',(-0.118272920182323,-0.140952177533892,0.04));
#48071=CARTESIAN_POINT('Origin',(-0.118272920182323,-0.140952177533892,
0.04));
#48072=CARTESIAN_POINT('',(-0.123361285143431,-0.144506032150084,0.185));
#48073=CARTESIAN_POINT('',(-0.123361285143431,-0.144506032150084,0.0925));
#48074=CARTESIAN_POINT('',(-0.118272920182323,-0.140952177533892,0.191));
#48075=CARTESIAN_POINT('',(-0.118272920182323,-0.140952177533892,0.04));
#48076=CARTESIAN_POINT('Ctrl Pts',(-0.123361285143431,-0.144506032150084,
0.185));
#48077=CARTESIAN_POINT('Ctrl Pts',(-0.120776286901195,-0.142700597986805,
0.188051499118418));
#48078=CARTESIAN_POINT('Ctrl Pts',(-0.118272920182323,-0.140952177533892,
0.191));
#48079=CARTESIAN_POINT('Origin',(-0.12962308693234,-0.165368846322791,0.04));
#48080=CARTESIAN_POINT('',(-0.120889198458627,-0.146580359175541,0.185));
#48081=CARTESIAN_POINT('',(-0.120889198458627,-0.146580359175541,0.0925));
#48082=CARTESIAN_POINT('Ctrl Pts',(-0.118272920182323,-0.140952177533892,
0.191));
#48083=CARTESIAN_POINT('Ctrl Pts',(-0.119560073131103,-0.143721122512692,
0.188051499118441));
#48084=CARTESIAN_POINT('Ctrl Pts',(-0.120889198458627,-0.146580359175541,
0.185));
#48085=CARTESIAN_POINT('Origin',(-0.150910755294439,-0.126629159108248,
0.04));
#48086=CARTESIAN_POINT('',(-0.144506032150084,-0.123361285143431,0.04));
#48087=CARTESIAN_POINT('',(-0.146580359175541,-0.120889198458627,0.04));
#48088=CARTESIAN_POINT('Origin',(0.,0.,0.04));
#48089=CARTESIAN_POINT('',(-0.140952177533892,-0.118272920182323,0.04));
#48090=CARTESIAN_POINT('',(-0.15636981978718,-0.140347709136006,0.04));
#48091=CARTESIAN_POINT('',(-0.140952177533892,-0.118272920182323,0.04));
#48092=CARTESIAN_POINT('Origin',(-0.140952177533892,-0.118272920182323,
0.04));
#48093=CARTESIAN_POINT('',(-0.146580359175541,-0.120889198458627,0.185));
#48094=CARTESIAN_POINT('',(-0.146580359175541,-0.120889198458627,0.0925));
#48095=CARTESIAN_POINT('',(-0.140952177533892,-0.118272920182323,0.191));
#48096=CARTESIAN_POINT('',(-0.140952177533892,-0.118272920182323,0.04));
#48097=CARTESIAN_POINT('Ctrl Pts',(-0.146580359175541,-0.120889198458627,
0.185));
#48098=CARTESIAN_POINT('Ctrl Pts',(-0.14372112251267,-0.119560073131093,
0.188051499118464));
#48099=CARTESIAN_POINT('Ctrl Pts',(-0.140952177533892,-0.118272920182323,
0.191));
#48100=CARTESIAN_POINT('Origin',(-0.15636981978718,-0.140347709136006,0.04));
#48101=CARTESIAN_POINT('',(-0.144506032150084,-0.123361285143431,0.185));
#48102=CARTESIAN_POINT('',(-0.144506032150084,-0.123361285143431,0.0925));
#48103=CARTESIAN_POINT('Ctrl Pts',(-0.140952177533892,-0.118272920182323,
0.191));
#48104=CARTESIAN_POINT('Ctrl Pts',(-0.142700597986788,-0.120776286901171,
0.188051499118446));
#48105=CARTESIAN_POINT('Ctrl Pts',(-0.144506032150084,-0.123361285143431,
0.185));
#48106=CARTESIAN_POINT('Origin',(-0.170607004545534,-0.0985,0.04));
#48107=CARTESIAN_POINT('',(-0.163732123178242,-0.0963939408860592,0.04));
#48108=CARTESIAN_POINT('',(-0.165345663167344,-0.0935992076448906,0.04));
#48109=CARTESIAN_POINT('Origin',(0.,0.,0.04));
#48110=CARTESIAN_POINT('',(-0.159348674296337,-0.092,0.04));
#48111=CARTESIAN_POINT('',(-0.178365334794732,-0.111062177826491,0.04));
#48112=CARTESIAN_POINT('',(-0.159348674296337,-0.092,0.04));
#48113=CARTESIAN_POINT('Origin',(-0.159348674296337,-0.092,0.04));
#48114=CARTESIAN_POINT('',(-0.165345663167344,-0.0935992076448906,0.185));
#48115=CARTESIAN_POINT('',(-0.165345663167344,-0.0935992076448906,0.0925));
#48116=CARTESIAN_POINT('',(-0.159348674296337,-0.0919999999999999,0.191));
#48117=CARTESIAN_POINT('',(-0.159348674296337,-0.092,0.04));
#48118=CARTESIAN_POINT('Ctrl Pts',(-0.165345663167344,-0.0935992076448906,
0.185));
#48119=CARTESIAN_POINT('Ctrl Pts',(-0.16229906454304,-0.0927867759536372,
0.188051499118458));
#48120=CARTESIAN_POINT('Ctrl Pts',(-0.159348674296337,-0.0919999999999999,
0.191));
#48121=CARTESIAN_POINT('Origin',(-0.178365334794732,-0.111062177826491,
0.04));
#48122=CARTESIAN_POINT('',(-0.163732123178242,-0.0963939408860592,0.185));
#48123=CARTESIAN_POINT('',(-0.163732123178242,-0.0963939408860592,0.0925));
#48124=CARTESIAN_POINT('Ctrl Pts',(-0.159348674296337,-0.0919999999999999,
0.191));
#48125=CARTESIAN_POINT('Ctrl Pts',(-0.161505237382618,-0.0941617249278968,
0.188051499118469));
#48126=CARTESIAN_POINT('Ctrl Pts',(-0.163732123178242,-0.0963939408860592,
0.185));
#48127=CARTESIAN_POINT('Origin',(-0.185119446294824,-0.0673779682351567,
0.04));
#48128=CARTESIAN_POINT('',(-0.17798329649608,-0.0664977155125525,0.04));
#48129=CARTESIAN_POINT('',(-0.179087022852749,-0.0634652522703485,0.04));
#48130=CARTESIAN_POINT('Origin',(0.,0.,0.04));
#48131=CARTESIAN_POINT('',(-0.172903442224607,-0.062931706371923,0.04));
#48132=CARTESIAN_POINT('',(-0.194941309361761,-0.0784020784438918,0.04));
#48133=CARTESIAN_POINT('',(-0.172903442224607,-0.062931706371923,0.04));
#48134=CARTESIAN_POINT('Origin',(-0.172903442224607,-0.062931706371923,
0.04));
#48135=CARTESIAN_POINT('',(-0.179087022852749,-0.0634652522703485,0.185));
#48136=CARTESIAN_POINT('',(-0.179087022852749,-0.0634652522703485,0.0925));
#48137=CARTESIAN_POINT('',(-0.172903442224607,-0.062931706371923,0.191));
#48138=CARTESIAN_POINT('',(-0.172903442224607,-0.062931706371923,0.04));
#48139=CARTESIAN_POINT('Ctrl Pts',(-0.179087022852749,-0.0634652522703485,
0.185));
#48140=CARTESIAN_POINT('Ctrl Pts',(-0.175945631624537,-0.0631941995412009,
0.188051499118474));
#48141=CARTESIAN_POINT('Ctrl Pts',(-0.172903442224607,-0.062931706371923,
0.191));
#48142=CARTESIAN_POINT('Origin',(-0.194941309361761,-0.0784020784438918,
0.04));
#48143=CARTESIAN_POINT('',(-0.17798329649608,-0.0664977155125525,0.185));
#48144=CARTESIAN_POINT('',(-0.17798329649608,-0.0664977155125525,0.0925));
#48145=CARTESIAN_POINT('Ctrl Pts',(-0.172903442224607,-0.062931706371923,
0.191));
#48146=CARTESIAN_POINT('Ctrl Pts',(-0.175402621866193,-0.0646861065908464,
0.188051499118456));
#48147=CARTESIAN_POINT('Ctrl Pts',(-0.17798329649608,-0.0664977155125525,
0.185));
#48148=CARTESIAN_POINT('Origin',(-0.194007127343405,-0.0342086910003852,
0.04));
#48149=CARTESIAN_POINT('',(-0.186826537413779,-0.0345809907026646,0.04));
#48150=CARTESIAN_POINT('',(-0.18738691397118,-0.031402937320539,0.04));
#48151=CARTESIAN_POINT('Origin',(0.,0.,0.04));
#48152=CARTESIAN_POINT('',(-0.181204626554246,-0.0319512646907151,0.04));
#48153=CARTESIAN_POINT('',(-0.205594090888895,-0.0433597715811408,0.04));
#48154=CARTESIAN_POINT('',(-0.181204626554246,-0.0319512646907151,0.04));
#48155=CARTESIAN_POINT('Origin',(-0.181204626554246,-0.0319512646907151,
0.04));
#48156=CARTESIAN_POINT('',(-0.18738691397118,-0.031402937320539,0.185));
#48157=CARTESIAN_POINT('',(-0.18738691397118,-0.031402937320539,0.0925));
#48158=CARTESIAN_POINT('',(-0.181204626554246,-0.0319512646907151,0.191));
#48159=CARTESIAN_POINT('',(-0.181204626554246,-0.0319512646907151,0.04));
#48160=CARTESIAN_POINT('Ctrl Pts',(-0.18738691397118,-0.031402937320539,
0.185));
#48161=CARTESIAN_POINT('Ctrl Pts',(-0.184246179721915,-0.031681499353518,
0.188051499118483));
#48162=CARTESIAN_POINT('Ctrl Pts',(-0.181204626554246,-0.0319512646907151,
0.191));
#48163=CARTESIAN_POINT('Origin',(-0.205594090888895,-0.0433597715811408,
0.04));
#48164=CARTESIAN_POINT('',(-0.186826537413779,-0.0345809907026646,0.185));
#48165=CARTESIAN_POINT('',(-0.186826537413779,-0.0345809907026646,0.0925));
#48166=CARTESIAN_POINT('Ctrl Pts',(-0.181204626554246,-0.0319512646907151,
0.191));
#48167=CARTESIAN_POINT('Ctrl Pts',(-0.183970486442384,-0.0332450336377824,
0.188051499118436));
#48168=CARTESIAN_POINT('Ctrl Pts',(-0.186826537413779,-0.0345809907026646,
0.185));
#48169=CARTESIAN_POINT('Origin',(-0.197,2.08166817117217E-17,0.04));
#48170=CARTESIAN_POINT('',(-0.18999314853095,-0.00161353998910186,0.04));
#48171=CARTESIAN_POINT('',(-0.19,-2.32682891837997E-17,0.04));
#48172=CARTESIAN_POINT('Origin',(0.,0.,0.04));
#48173=CARTESIAN_POINT('',(-0.184,2.08166817117217E-17,0.04));
#48174=CARTESIAN_POINT('',(-0.21,-0.00699999999999998,0.04));
#48175=CARTESIAN_POINT('',(-0.18999314853095,0.0016135399891019,0.04));
#48176=CARTESIAN_POINT('',(-0.184,2.08166817117217E-17,0.04));
#48177=CARTESIAN_POINT('Origin',(0.,0.,0.04));
#48178=CARTESIAN_POINT('Origin',(-0.184,2.08166817117217E-17,0.04));
#48179=CARTESIAN_POINT('',(-0.18999314853095,0.00161353998910189,0.185));
#48180=CARTESIAN_POINT('',(-0.18999314853095,0.00161353998910189,0.0925));
#48181=CARTESIAN_POINT('',(-0.184,2.08166817117217E-17,0.191));
#48182=CARTESIAN_POINT('',(-0.184,2.08166817117217E-17,0.04));
#48183=CARTESIAN_POINT('Ctrl Pts',(-0.18999314853095,0.00161353998910189,
0.185));
#48184=CARTESIAN_POINT('Ctrl Pts',(-0.186948500881544,0.000793827160415821,
0.188051499118456));
#48185=CARTESIAN_POINT('Ctrl Pts',(-0.184,2.08166817117217E-17,0.191));
#48186=CARTESIAN_POINT('Origin',(-0.21,-0.00699999999999998,0.04));
#48187=CARTESIAN_POINT('',(-0.18999314853095,-0.00161353998910186,0.185));
#48188=CARTESIAN_POINT('',(-0.18999314853095,-0.00161353998910186,0.0925));
#48189=CARTESIAN_POINT('Ctrl Pts',(-0.184,2.08166817117217E-17,0.191));
#48190=CARTESIAN_POINT('Ctrl Pts',(-0.186948500881545,-0.000793827160416021,
0.188051499118455));
#48191=CARTESIAN_POINT('Ctrl Pts',(-0.18999314853095,-0.00161353998910185,
0.185));
#48192=CARTESIAN_POINT('Origin',(-0.194007127343405,0.0342086910003854,
0.04));
#48193=CARTESIAN_POINT('',(-0.18738691397118,0.0314029373205392,0.04));
#48194=CARTESIAN_POINT('',(-0.186826537413779,0.0345809907026647,0.04));
#48195=CARTESIAN_POINT('Origin',(0.,0.,0.04));
#48196=CARTESIAN_POINT('',(-0.181204626554246,0.0319512646907152,0.04));
#48197=CARTESIAN_POINT('',(-0.208025165376232,0.02957246303897,0.04));
#48198=CARTESIAN_POINT('',(-0.181204626554246,0.0319512646907152,0.04));
#48199=CARTESIAN_POINT('Origin',(-0.181204626554246,0.0319512646907152,
0.04));
#48200=CARTESIAN_POINT('',(-0.186826537413779,0.0345809907026647,0.185));
#48201=CARTESIAN_POINT('',(-0.186826537413779,0.0345809907026647,0.0925));
#48202=CARTESIAN_POINT('',(-0.181204626554246,0.0319512646907153,0.191));
#48203=CARTESIAN_POINT('',(-0.181204626554246,0.0319512646907152,0.04));
#48204=CARTESIAN_POINT('Ctrl Pts',(-0.186826537413779,0.0345809907026647,
0.185));
#48205=CARTESIAN_POINT('Ctrl Pts',(-0.183970486442384,0.0332450336377824,
0.188051499118436));
#48206=CARTESIAN_POINT('Ctrl Pts',(-0.181204626554246,0.0319512646907153,
0.191));
#48207=CARTESIAN_POINT('Origin',(-0.208025165376232,0.02957246303897,0.04));
#48208=CARTESIAN_POINT('',(-0.18738691397118,0.0314029373205392,0.185));
#48209=CARTESIAN_POINT('',(-0.18738691397118,0.0314029373205392,0.0925));
#48210=CARTESIAN_POINT('Ctrl Pts',(-0.181204626554246,0.0319512646907153,
0.191));
#48211=CARTESIAN_POINT('Ctrl Pts',(-0.184246179721934,0.0316814993535164,
0.188051499118464));
#48212=CARTESIAN_POINT('Ctrl Pts',(-0.18738691397118,0.0314029373205392,
0.185));
#48213=CARTESIAN_POINT('Origin',(-0.185119446294824,0.0673779682351568,
0.04));
#48214=CARTESIAN_POINT('',(-0.179087022852749,0.0634652522703486,0.04));
#48215=CARTESIAN_POINT('',(-0.17798329649608,0.0664977155125526,0.04));
#48216=CARTESIAN_POINT('Origin',(0.,0.,0.04));
#48217=CARTESIAN_POINT('',(-0.172903442224607,0.0629317063719231,0.04));
#48218=CARTESIAN_POINT('',(-0.199729591368321,0.0652463817528891,0.04));
#48219=CARTESIAN_POINT('',(-0.172903442224607,0.0629317063719231,0.04));
#48220=CARTESIAN_POINT('Origin',(-0.172903442224607,0.0629317063719231,
0.04));
#48221=CARTESIAN_POINT('',(-0.17798329649608,0.0664977155125526,0.185));
#48222=CARTESIAN_POINT('',(-0.17798329649608,0.0664977155125526,0.0925));
#48223=CARTESIAN_POINT('',(-0.172903442224607,0.0629317063719231,0.191));
#48224=CARTESIAN_POINT('',(-0.172903442224607,0.0629317063719231,0.04));
#48225=CARTESIAN_POINT('Ctrl Pts',(-0.17798329649608,0.0664977155125526,
0.185));
#48226=CARTESIAN_POINT('Ctrl Pts',(-0.175402621866187,0.0646861065908417,
0.188051499118464));
#48227=CARTESIAN_POINT('Ctrl Pts',(-0.172903442224607,0.0629317063719231,
0.191));
#48228=CARTESIAN_POINT('Origin',(-0.199729591368321,0.0652463817528891,
0.04));
#48229=CARTESIAN_POINT('',(-0.179087022852749,0.0634652522703485,0.185));
#48230=CARTESIAN_POINT('',(-0.179087022852749,0.0634652522703485,0.0925));
#48231=CARTESIAN_POINT('Ctrl Pts',(-0.172903442224607,0.0629317063719231,
0.191));
#48232=CARTESIAN_POINT('Ctrl Pts',(-0.175945631624522,0.0631941995411996,
0.188051499118489));
#48233=CARTESIAN_POINT('Ctrl Pts',(-0.179087022852749,0.0634652522703486,
0.185));
#48234=CARTESIAN_POINT('Origin',(-0.170607004545534,0.0985,0.04));
#48235=CARTESIAN_POINT('',(-0.165345663167344,0.0935992076448906,0.04));
#48236=CARTESIAN_POINT('',(-0.163732123178242,0.0963939408860592,0.04));
#48237=CARTESIAN_POINT('Origin',(0.,0.,0.04));
#48238=CARTESIAN_POINT('',(-0.159348674296337,0.092,0.04));
#48239=CARTESIAN_POINT('',(-0.185365334794732,0.098937822173509,0.04));
#48240=CARTESIAN_POINT('',(-0.159348674296337,0.092,0.04));
#48241=CARTESIAN_POINT('Origin',(-0.159348674296337,0.092,0.04));
#48242=CARTESIAN_POINT('',(-0.163732123178242,0.0963939408860592,0.185));
#48243=CARTESIAN_POINT('',(-0.163732123178242,0.0963939408860592,0.0925));
#48244=CARTESIAN_POINT('',(-0.159348674296337,0.092,0.191));
#48245=CARTESIAN_POINT('',(-0.159348674296337,0.092,0.04));
#48246=CARTESIAN_POINT('Ctrl Pts',(-0.163732123178242,0.0963939408860592,
0.185));
#48247=CARTESIAN_POINT('Ctrl Pts',(-0.161505237382624,0.0941617249279029,
0.18805149911846));
#48248=CARTESIAN_POINT('Ctrl Pts',(-0.159348674296337,0.092,0.191));
#48249=CARTESIAN_POINT('Origin',(-0.185365334794732,0.098937822173509,0.04));
#48250=CARTESIAN_POINT('',(-0.165345663167344,0.0935992076448906,0.185));
#48251=CARTESIAN_POINT('',(-0.165345663167344,0.0935992076448906,0.0925));
#48252=CARTESIAN_POINT('Ctrl Pts',(-0.159348674296337,0.092,0.191));
#48253=CARTESIAN_POINT('Ctrl Pts',(-0.162299064543065,0.0927867759536439,
0.188051499118434));
#48254=CARTESIAN_POINT('Ctrl Pts',(-0.165345663167344,0.0935992076448907,
0.185));
#48255=CARTESIAN_POINT('Origin',(-0.150910755294439,0.126629159108248,0.04));
#48256=CARTESIAN_POINT('',(-0.146580359175541,0.120889198458627,0.04));
#48257=CARTESIAN_POINT('',(-0.144506032150084,0.123361285143431,0.04));
#48258=CARTESIAN_POINT('Origin',(0.,0.,0.04));
#48259=CARTESIAN_POINT('',(-0.140952177533892,0.118272920182323,0.04));
#48260=CARTESIAN_POINT('',(-0.165368846322791,0.12962308693234,0.04));
#48261=CARTESIAN_POINT('',(-0.140952177533892,0.118272920182323,0.04));
#48262=CARTESIAN_POINT('Origin',(-0.140952177533892,0.118272920182323,0.04));
#48263=CARTESIAN_POINT('',(-0.144506032150084,0.123361285143431,0.185));
#48264=CARTESIAN_POINT('',(-0.144506032150084,0.123361285143431,0.0925));
#48265=CARTESIAN_POINT('',(-0.140952177533892,0.118272920182323,0.191));
#48266=CARTESIAN_POINT('',(-0.140952177533892,0.118272920182323,0.04));
#48267=CARTESIAN_POINT('Ctrl Pts',(-0.144506032150084,0.123361285143431,
0.185));
#48268=CARTESIAN_POINT('Ctrl Pts',(-0.142700597986805,0.120776286901195,
0.188051499118418));
#48269=CARTESIAN_POINT('Ctrl Pts',(-0.140952177533892,0.118272920182323,
0.191));
#48270=CARTESIAN_POINT('Origin',(-0.165368846322791,0.12962308693234,0.04));
#48271=CARTESIAN_POINT('',(-0.146580359175541,0.120889198458627,0.185));
#48272=CARTESIAN_POINT('',(-0.146580359175541,0.120889198458627,0.0925));
#48273=CARTESIAN_POINT('Ctrl Pts',(-0.140952177533892,0.118272920182323,
0.191));
#48274=CARTESIAN_POINT('Ctrl Pts',(-0.143721122512692,0.119560073131103,
0.188051499118441));
#48275=CARTESIAN_POINT('Ctrl Pts',(-0.146580359175541,0.120889198458627,
0.185));
#48276=CARTESIAN_POINT('Origin',(-0.126629159108248,0.150910755294439,0.04));
#48277=CARTESIAN_POINT('',(-0.123361285143431,0.144506032150084,0.04));
#48278=CARTESIAN_POINT('',(-0.120889198458627,0.146580359175541,0.04));
#48279=CARTESIAN_POINT('Origin',(0.,0.,0.04));
#48280=CARTESIAN_POINT('',(-0.118272920182323,0.140952177533892,0.04));
#48281=CARTESIAN_POINT('',(-0.140347709136006,0.15636981978718,0.04));
#48282=CARTESIAN_POINT('',(-0.118272920182323,0.140952177533892,0.04));
#48283=CARTESIAN_POINT('Origin',(-0.118272920182323,0.140952177533892,0.04));
#48284=CARTESIAN_POINT('',(-0.120889198458627,0.146580359175541,0.185));
#48285=CARTESIAN_POINT('',(-0.120889198458627,0.146580359175541,0.0925));
#48286=CARTESIAN_POINT('',(-0.118272920182323,0.140952177533892,0.191));
#48287=CARTESIAN_POINT('',(-0.118272920182323,0.140952177533892,0.04));
#48288=CARTESIAN_POINT('Ctrl Pts',(-0.120889198458627,0.146580359175541,
0.185));
#48289=CARTESIAN_POINT('Ctrl Pts',(-0.1195600731311,0.143721122512687,0.188051499118446));
#48290=CARTESIAN_POINT('Ctrl Pts',(-0.118272920182323,0.140952177533892,
0.191));
#48291=CARTESIAN_POINT('Origin',(-0.140347709136006,0.15636981978718,0.04));
#48292=CARTESIAN_POINT('',(-0.123361285143431,0.144506032150084,0.185));
#48293=CARTESIAN_POINT('',(-0.123361285143431,0.144506032150084,0.0925));
#48294=CARTESIAN_POINT('Ctrl Pts',(-0.118272920182323,0.140952177533892,
0.191));
#48295=CARTESIAN_POINT('Ctrl Pts',(-0.120776286901187,0.142700597986799,
0.188051499118427));
#48296=CARTESIAN_POINT('Ctrl Pts',(-0.123361285143431,0.144506032150084,
0.185));
#48297=CARTESIAN_POINT('Origin',(-0.0985,0.170607004545534,0.04));
#48298=CARTESIAN_POINT('',(-0.0963939408860591,0.163732123178242,0.04));
#48299=CARTESIAN_POINT('',(-0.0935992076448906,0.165345663167344,0.04));
#48300=CARTESIAN_POINT('Origin',(0.,0.,0.04));
#48301=CARTESIAN_POINT('',(-0.092,0.159348674296337,0.04));
#48302=CARTESIAN_POINT('',(-0.111062177826491,0.178365334794732,0.04));
#48303=CARTESIAN_POINT('',(-0.092,0.159348674296337,0.04));
#48304=CARTESIAN_POINT('Origin',(-0.092,0.159348674296337,0.04));
#48305=CARTESIAN_POINT('',(-0.0935992076448906,0.165345663167344,0.185));
#48306=CARTESIAN_POINT('',(-0.0935992076448906,0.165345663167344,0.0925));
#48307=CARTESIAN_POINT('',(-0.092,0.159348674296337,0.191));
#48308=CARTESIAN_POINT('',(-0.092,0.159348674296337,0.04));
#48309=CARTESIAN_POINT('Ctrl Pts',(-0.0935992076448906,0.165345663167344,
0.185));
#48310=CARTESIAN_POINT('Ctrl Pts',(-0.0927867759536353,0.162299064543033,
0.188051499118466));
#48311=CARTESIAN_POINT('Ctrl Pts',(-0.092,0.159348674296337,0.191));
#48312=CARTESIAN_POINT('Origin',(-0.111062177826491,0.178365334794732,0.04));
#48313=CARTESIAN_POINT('',(-0.0963939408860592,0.163732123178242,0.185));
#48314=CARTESIAN_POINT('',(-0.0963939408860592,0.163732123178242,0.0925));
#48315=CARTESIAN_POINT('Ctrl Pts',(-0.092,0.159348674296337,0.191));
#48316=CARTESIAN_POINT('Ctrl Pts',(-0.0941617249279073,0.161505237382628,
0.188051499118454));
#48317=CARTESIAN_POINT('Ctrl Pts',(-0.0963939408860592,0.163732123178242,
0.185));
#48318=CARTESIAN_POINT('Origin',(-0.0673779682351567,0.185119446294824,
0.04));
#48319=CARTESIAN_POINT('',(-0.0664977155125525,0.17798329649608,0.04));
#48320=CARTESIAN_POINT('',(-0.0634652522703485,0.179087022852749,0.04));
#48321=CARTESIAN_POINT('Origin',(0.,0.,0.04));
#48322=CARTESIAN_POINT('',(-0.062931706371923,0.172903442224607,0.04));
#48323=CARTESIAN_POINT('',(-0.0784020784438918,0.194941309361761,0.04));
#48324=CARTESIAN_POINT('',(-0.062931706371923,0.172903442224607,0.04));
#48325=CARTESIAN_POINT('Origin',(-0.062931706371923,0.172903442224607,0.04));
#48326=CARTESIAN_POINT('',(-0.0634652522703485,0.179087022852749,0.185));
#48327=CARTESIAN_POINT('',(-0.0634652522703485,0.179087022852749,0.0925));
#48328=CARTESIAN_POINT('',(-0.062931706371923,0.172903442224607,0.191));
#48329=CARTESIAN_POINT('',(-0.062931706371923,0.172903442224607,0.04));
#48330=CARTESIAN_POINT('Ctrl Pts',(-0.0634652522703485,0.179087022852749,
0.185));
#48331=CARTESIAN_POINT('Ctrl Pts',(-0.0631941995412009,0.175945631624537,
0.188051499118474));
#48332=CARTESIAN_POINT('Ctrl Pts',(-0.062931706371923,0.172903442224607,
0.191));
#48333=CARTESIAN_POINT('Origin',(-0.0784020784438918,0.194941309361761,
0.04));
#48334=CARTESIAN_POINT('',(-0.0664977155125525,0.17798329649608,0.185));
#48335=CARTESIAN_POINT('',(-0.0664977155125525,0.17798329649608,0.0925));
#48336=CARTESIAN_POINT('Ctrl Pts',(-0.062931706371923,0.172903442224607,
0.191));
#48337=CARTESIAN_POINT('Ctrl Pts',(-0.0646861065908464,0.175402621866193,
0.188051499118456));
#48338=CARTESIAN_POINT('Ctrl Pts',(-0.0664977155125525,0.17798329649608,
0.185));
#48339=CARTESIAN_POINT('Origin',(-0.0342086910003853,0.194007127343405,
0.04));
#48340=CARTESIAN_POINT('',(-0.0345809907026646,0.186826537413779,0.04));
#48341=CARTESIAN_POINT('',(-0.0314029373205391,0.18738691397118,0.04));
#48342=CARTESIAN_POINT('Origin',(0.,0.,0.04));
#48343=CARTESIAN_POINT('',(-0.0319512646907152,0.181204626554246,0.04));
#48344=CARTESIAN_POINT('',(-0.0433597715811408,0.205594090888895,0.04));
#48345=CARTESIAN_POINT('',(-0.0319512646907152,0.181204626554246,0.04));
#48346=CARTESIAN_POINT('Origin',(-0.0319512646907152,0.181204626554246,
0.04));
#48347=CARTESIAN_POINT('',(-0.0314029373205391,0.18738691397118,0.185));
#48348=CARTESIAN_POINT('',(-0.0314029373205391,0.18738691397118,0.0925));
#48349=CARTESIAN_POINT('',(-0.0319512646907152,0.181204626554246,0.191));
#48350=CARTESIAN_POINT('',(-0.0319512646907152,0.181204626554246,0.04));
#48351=CARTESIAN_POINT('Ctrl Pts',(-0.0314029373205391,0.18738691397118,
0.185));
#48352=CARTESIAN_POINT('Ctrl Pts',(-0.031681499353516,0.184246179721939,
0.18805149911846));
#48353=CARTESIAN_POINT('Ctrl Pts',(-0.0319512646907152,0.181204626554246,
0.191));
#48354=CARTESIAN_POINT('Origin',(-0.0433597715811408,0.205594090888895,
0.04));
#48355=CARTESIAN_POINT('',(-0.0345809907026646,0.186826537413779,0.185));
#48356=CARTESIAN_POINT('',(-0.0345809907026646,0.186826537413779,0.0925));
#48357=CARTESIAN_POINT('Ctrl Pts',(-0.0319512646907152,0.181204626554246,
0.191));
#48358=CARTESIAN_POINT('Ctrl Pts',(-0.033245033637777,0.183970486442373,
0.188051499118448));
#48359=CARTESIAN_POINT('Ctrl Pts',(-0.0345809907026646,0.186826537413779,
0.185));
#48360=CARTESIAN_POINT('Origin',(1.38777878078145E-17,0.197,0.04));
#48361=CARTESIAN_POINT('',(-0.00161353998910187,0.18999314853095,0.04));
#48362=CARTESIAN_POINT('',(0.00161353998910189,0.18999314853095,0.04));
#48363=CARTESIAN_POINT('Origin',(0.,0.,0.04));
#48364=CARTESIAN_POINT('',(6.93889390390723E-18,0.184,0.04));
#48365=CARTESIAN_POINT('',(-0.00699999999999999,0.21,0.04));
#48366=CARTESIAN_POINT('',(6.93889390390723E-18,0.184,0.04));
#48367=CARTESIAN_POINT('Origin',(6.93889390390723E-18,0.184,0.04));
#48368=CARTESIAN_POINT('',(0.00161353998910188,0.18999314853095,0.185));
#48369=CARTESIAN_POINT('',(0.00161353998910188,0.18999314853095,0.0925));
#48370=CARTESIAN_POINT('',(6.93889390390723E-18,0.184,0.191));
#48371=CARTESIAN_POINT('',(6.93889390390723E-18,0.184,0.04));
#48372=CARTESIAN_POINT('Ctrl Pts',(0.00161353998910188,0.18999314853095,
0.185));
#48373=CARTESIAN_POINT('Ctrl Pts',(0.000793827160417808,0.186948500881552,
0.188051499118448));
#48374=CARTESIAN_POINT('Ctrl Pts',(6.93889390390723E-18,0.184,0.191));
#48375=CARTESIAN_POINT('Origin',(-0.00699999999999999,0.21,0.04));
#48376=CARTESIAN_POINT('',(-0.00161353998910187,0.18999314853095,0.185));
#48377=CARTESIAN_POINT('',(-0.00161353998910187,0.18999314853095,0.0925));
#48378=CARTESIAN_POINT('Ctrl Pts',(6.93889390390723E-18,0.184,0.191));
#48379=CARTESIAN_POINT('Ctrl Pts',(-0.000793827160415599,0.186948500881544,
0.188051499118456));
#48380=CARTESIAN_POINT('Ctrl Pts',(-0.00161353998910187,0.18999314853095,
0.185));
#48381=CARTESIAN_POINT('Origin',(0.0342086910003853,0.194007127343405,0.04));
#48382=CARTESIAN_POINT('',(0.0314029373205391,0.18738691397118,0.04));
#48383=CARTESIAN_POINT('',(0.0345809907026646,0.186826537413779,0.04));
#48384=CARTESIAN_POINT('Origin',(0.,0.,0.04));
#48385=CARTESIAN_POINT('',(0.0319512646907152,0.181204626554246,0.04));
#48386=CARTESIAN_POINT('',(0.02957246303897,0.208025165376232,0.04));
#48387=CARTESIAN_POINT('',(0.0319512646907152,0.181204626554246,0.04));
#48388=CARTESIAN_POINT('Origin',(0.0319512646907152,0.181204626554246,0.04));
#48389=CARTESIAN_POINT('',(0.0345809907026646,0.186826537413779,0.185));
#48390=CARTESIAN_POINT('',(0.0345809907026646,0.186826537413779,0.0925));
#48391=CARTESIAN_POINT('',(0.0319512646907152,0.181204626554246,0.191));
#48392=CARTESIAN_POINT('',(0.0319512646907152,0.181204626554246,0.04));
#48393=CARTESIAN_POINT('Ctrl Pts',(0.0345809907026646,0.186826537413779,
0.185));
#48394=CARTESIAN_POINT('Ctrl Pts',(0.0332450336377822,0.183970486442384,
0.188051499118437));
#48395=CARTESIAN_POINT('Ctrl Pts',(0.0319512646907152,0.181204626554246,
0.191));
#48396=CARTESIAN_POINT('Origin',(0.02957246303897,0.208025165376232,0.04));
#48397=CARTESIAN_POINT('',(0.0314029373205391,0.18738691397118,0.185));
#48398=CARTESIAN_POINT('',(0.0314029373205391,0.18738691397118,0.0925));
#48399=CARTESIAN_POINT('Ctrl Pts',(0.0319512646907152,0.181204626554246,
0.191));
#48400=CARTESIAN_POINT('Ctrl Pts',(0.0316814993535166,0.184246179721932,
0.188051499118467));
#48401=CARTESIAN_POINT('Ctrl Pts',(0.0314029373205392,0.18738691397118,
0.185));
#48402=CARTESIAN_POINT('Origin',(0.0673779682351568,0.185119446294824,0.04));
#48403=CARTESIAN_POINT('',(0.0634652522703486,0.179087022852749,0.04));
#48404=CARTESIAN_POINT('',(0.0664977155125526,0.17798329649608,0.04));
#48405=CARTESIAN_POINT('Origin',(0.,0.,0.04));
#48406=CARTESIAN_POINT('',(0.0629317063719231,0.172903442224607,0.04));
#48407=CARTESIAN_POINT('',(0.0652463817528891,0.199729591368321,0.04));
#48408=CARTESIAN_POINT('',(0.0629317063719231,0.172903442224607,0.04));
#48409=CARTESIAN_POINT('Origin',(0.0629317063719231,0.172903442224607,0.04));
#48410=CARTESIAN_POINT('',(0.0664977155125526,0.17798329649608,0.185));
#48411=CARTESIAN_POINT('',(0.0664977155125526,0.17798329649608,0.0925));
#48412=CARTESIAN_POINT('',(0.0629317063719231,0.172903442224607,0.191));
#48413=CARTESIAN_POINT('',(0.0629317063719231,0.172903442224607,0.04));
#48414=CARTESIAN_POINT('Ctrl Pts',(0.0664977155125526,0.17798329649608,
0.185));
#48415=CARTESIAN_POINT('Ctrl Pts',(0.0646861065908417,0.175402621866187,
0.188051499118464));
#48416=CARTESIAN_POINT('Ctrl Pts',(0.0629317063719231,0.172903442224607,
0.191));
#48417=CARTESIAN_POINT('Origin',(0.0652463817528891,0.199729591368321,0.04));
#48418=CARTESIAN_POINT('',(0.0634652522703485,0.179087022852749,0.185));
#48419=CARTESIAN_POINT('',(0.0634652522703485,0.179087022852749,0.0925));
#48420=CARTESIAN_POINT('Ctrl Pts',(0.0629317063719231,0.172903442224607,
0.191));
#48421=CARTESIAN_POINT('Ctrl Pts',(0.0631941995411996,0.175945631624522,
0.188051499118489));
#48422=CARTESIAN_POINT('Ctrl Pts',(0.0634652522703486,0.179087022852749,
0.185));
#48423=CARTESIAN_POINT('Origin',(0.0985,0.170607004545534,0.04));
#48424=CARTESIAN_POINT('',(0.0935992076448906,0.165345663167344,0.04));
#48425=CARTESIAN_POINT('',(0.0963939408860592,0.163732123178242,0.04));
#48426=CARTESIAN_POINT('Origin',(0.,0.,0.04));
#48427=CARTESIAN_POINT('',(0.092,0.159348674296337,0.04));
#48428=CARTESIAN_POINT('',(0.098937822173509,0.185365334794732,0.04));
#48429=CARTESIAN_POINT('',(0.092,0.159348674296337,0.04));
#48430=CARTESIAN_POINT('Origin',(0.092,0.159348674296337,0.04));
#48431=CARTESIAN_POINT('',(0.0963939408860592,0.163732123178242,0.185));
#48432=CARTESIAN_POINT('',(0.0963939408860592,0.163732123178242,0.0925));
#48433=CARTESIAN_POINT('',(0.092,0.159348674296337,0.191));
#48434=CARTESIAN_POINT('',(0.092,0.159348674296337,0.04));
#48435=CARTESIAN_POINT('Ctrl Pts',(0.0963939408860592,0.163732123178242,
0.185));
#48436=CARTESIAN_POINT('Ctrl Pts',(0.0941617249279218,0.161505237382642,
0.188051499118435));
#48437=CARTESIAN_POINT('Ctrl Pts',(0.092,0.159348674296337,0.191));
#48438=CARTESIAN_POINT('Origin',(0.098937822173509,0.185365334794732,0.04));
#48439=CARTESIAN_POINT('',(0.0935992076448906,0.165345663167344,0.185));
#48440=CARTESIAN_POINT('',(0.0935992076448906,0.165345663167344,0.0925));
#48441=CARTESIAN_POINT('Ctrl Pts',(0.092,0.159348674296337,0.191));
#48442=CARTESIAN_POINT('Ctrl Pts',(0.0927867759536358,0.162299064543034,
0.188051499118464));
#48443=CARTESIAN_POINT('Ctrl Pts',(0.0935992076448907,0.165345663167344,
0.185));
#48444=CARTESIAN_POINT('Origin',(0.126629159108248,0.150910755294439,0.04));
#48445=CARTESIAN_POINT('',(0.120889198458627,0.146580359175541,0.04));
#48446=CARTESIAN_POINT('',(0.123361285143431,0.144506032150084,0.04));
#48447=CARTESIAN_POINT('Origin',(0.,0.,0.04));
#48448=CARTESIAN_POINT('',(0.118272920182323,0.140952177533892,0.04));
#48449=CARTESIAN_POINT('',(0.12962308693234,0.165368846322791,0.04));
#48450=CARTESIAN_POINT('',(0.118272920182323,0.140952177533892,0.04));
#48451=CARTESIAN_POINT('Origin',(0.118272920182323,0.140952177533892,0.04));
#48452=CARTESIAN_POINT('',(0.123361285143431,0.144506032150084,0.185));
#48453=CARTESIAN_POINT('',(0.123361285143431,0.144506032150084,0.0925));
#48454=CARTESIAN_POINT('',(0.118272920182323,0.140952177533892,0.191));
#48455=CARTESIAN_POINT('',(0.118272920182323,0.140952177533892,0.04));
#48456=CARTESIAN_POINT('Ctrl Pts',(0.123361285143431,0.144506032150084,
0.185));
#48457=CARTESIAN_POINT('Ctrl Pts',(0.120776286901163,0.142700597986783,
0.188051499118455));
#48458=CARTESIAN_POINT('Ctrl Pts',(0.118272920182323,0.140952177533892,
0.191));
#48459=CARTESIAN_POINT('Origin',(0.12962308693234,0.165368846322791,0.04));
#48460=CARTESIAN_POINT('',(0.120889198458627,0.146580359175541,0.185));
#48461=CARTESIAN_POINT('',(0.120889198458627,0.146580359175541,0.0925));
#48462=CARTESIAN_POINT('Ctrl Pts',(0.118272920182323,0.140952177533892,
0.191));
#48463=CARTESIAN_POINT('Ctrl Pts',(0.119560073131097,0.14372112251268,0.188051499118454));
#48464=CARTESIAN_POINT('Ctrl Pts',(0.120889198458627,0.146580359175541,
0.185));
#48465=CARTESIAN_POINT('Origin',(0.150910755294439,0.126629159108248,0.04));
#48466=CARTESIAN_POINT('',(0.144506032150084,0.123361285143431,0.04));
#48467=CARTESIAN_POINT('',(0.146580359175541,0.120889198458627,0.04));
#48468=CARTESIAN_POINT('Origin',(0.,0.,0.04));
#48469=CARTESIAN_POINT('',(0.140952177533892,0.118272920182323,0.04));
#48470=CARTESIAN_POINT('',(0.15636981978718,0.140347709136006,0.04));
#48471=CARTESIAN_POINT('',(0.140952177533892,0.118272920182323,0.04));
#48472=CARTESIAN_POINT('Origin',(0.140952177533892,0.118272920182323,0.04));
#48473=CARTESIAN_POINT('',(0.146580359175541,0.120889198458627,0.185));
#48474=CARTESIAN_POINT('',(0.146580359175541,0.120889198458627,0.0925));
#48475=CARTESIAN_POINT('',(0.140952177533892,0.118272920182323,0.191));
#48476=CARTESIAN_POINT('',(0.140952177533892,0.118272920182323,0.04));
#48477=CARTESIAN_POINT('Ctrl Pts',(0.146580359175541,0.120889198458627,
0.185));
#48478=CARTESIAN_POINT('Ctrl Pts',(0.14372112251267,0.119560073131093,0.188051499118464));
#48479=CARTESIAN_POINT('Ctrl Pts',(0.140952177533892,0.118272920182323,
0.191));
#48480=CARTESIAN_POINT('Origin',(0.15636981978718,0.140347709136006,0.04));
#48481=CARTESIAN_POINT('',(0.144506032150084,0.123361285143431,0.185));
#48482=CARTESIAN_POINT('',(0.144506032150084,0.123361285143431,0.0925));
#48483=CARTESIAN_POINT('Ctrl Pts',(0.140952177533892,0.118272920182323,
0.191));
#48484=CARTESIAN_POINT('Ctrl Pts',(0.142700597986788,0.120776286901171,
0.188051499118446));
#48485=CARTESIAN_POINT('Ctrl Pts',(0.144506032150084,0.123361285143431,
0.185));
#48486=CARTESIAN_POINT('Origin',(0.170607004545534,0.0985,0.04));
#48487=CARTESIAN_POINT('',(0.163732123178242,0.0963939408860592,0.04));
#48488=CARTESIAN_POINT('',(0.165345663167344,0.0935992076448906,0.04));
#48489=CARTESIAN_POINT('Origin',(0.,0.,0.04));
#48490=CARTESIAN_POINT('',(0.159348674296337,0.092,0.04));
#48491=CARTESIAN_POINT('',(0.178365334794732,0.111062177826491,0.04));
#48492=CARTESIAN_POINT('',(0.159348674296337,0.092,0.04));
#48493=CARTESIAN_POINT('Origin',(0.159348674296337,0.092,0.04));
#48494=CARTESIAN_POINT('',(0.165345663167344,0.0935992076448906,0.185));
#48495=CARTESIAN_POINT('',(0.165345663167344,0.0935992076448906,0.0925));
#48496=CARTESIAN_POINT('',(0.159348674296337,0.092,0.191));
#48497=CARTESIAN_POINT('',(0.159348674296337,0.092,0.04));
#48498=CARTESIAN_POINT('Ctrl Pts',(0.165345663167344,0.0935992076448906,
0.185));
#48499=CARTESIAN_POINT('Ctrl Pts',(0.162299064543034,0.0927867759536356,
0.188051499118465));
#48500=CARTESIAN_POINT('Ctrl Pts',(0.159348674296337,0.092,0.191));
#48501=CARTESIAN_POINT('Origin',(0.178365334794732,0.111062177826491,0.04));
#48502=CARTESIAN_POINT('',(0.163732123178242,0.0963939408860592,0.185));
#48503=CARTESIAN_POINT('',(0.163732123178242,0.0963939408860592,0.0925));
#48504=CARTESIAN_POINT('Ctrl Pts',(0.159348674296337,0.092,0.191));
#48505=CARTESIAN_POINT('Ctrl Pts',(0.161505237382625,0.0941617249279039,
0.188051499118459));
#48506=CARTESIAN_POINT('Ctrl Pts',(0.163732123178242,0.0963939408860592,
0.185));
#48507=CARTESIAN_POINT('Origin',(0.185119446294824,0.0673779682351567,0.04));
#48508=CARTESIAN_POINT('',(0.17798329649608,0.0664977155125525,0.04));
#48509=CARTESIAN_POINT('',(0.179087022852749,0.0634652522703485,0.04));
#48510=CARTESIAN_POINT('Origin',(0.,0.,0.04));
#48511=CARTESIAN_POINT('',(0.172903442224607,0.062931706371923,0.04));
#48512=CARTESIAN_POINT('',(0.194941309361761,0.0784020784438918,0.04));
#48513=CARTESIAN_POINT('',(0.172903442224607,0.062931706371923,0.04));
#48514=CARTESIAN_POINT('Origin',(0.172903442224607,0.062931706371923,0.04));
#48515=CARTESIAN_POINT('',(0.179087022852749,0.0634652522703485,0.185));
#48516=CARTESIAN_POINT('',(0.179087022852749,0.0634652522703485,0.0925));
#48517=CARTESIAN_POINT('',(0.172903442224607,0.062931706371923,0.191));
#48518=CARTESIAN_POINT('',(0.172903442224607,0.062931706371923,0.04));
#48519=CARTESIAN_POINT('Ctrl Pts',(0.179087022852749,0.0634652522703485,
0.185));
#48520=CARTESIAN_POINT('Ctrl Pts',(0.175945631624537,0.0631941995412009,
0.188051499118474));
#48521=CARTESIAN_POINT('Ctrl Pts',(0.172903442224607,0.062931706371923,
0.191));
#48522=CARTESIAN_POINT('Origin',(0.194941309361761,0.0784020784438918,0.04));
#48523=CARTESIAN_POINT('',(0.17798329649608,0.0664977155125525,0.185));
#48524=CARTESIAN_POINT('',(0.17798329649608,0.0664977155125525,0.0925));
#48525=CARTESIAN_POINT('Ctrl Pts',(0.172903442224607,0.062931706371923,
0.191));
#48526=CARTESIAN_POINT('Ctrl Pts',(0.175402621866193,0.0646861065908464,
0.188051499118456));
#48527=CARTESIAN_POINT('Ctrl Pts',(0.17798329649608,0.0664977155125525,
0.185));
#48528=CARTESIAN_POINT('Origin',(0.194007127343405,0.0342086910003853,0.04));
#48529=CARTESIAN_POINT('',(0.186826537413779,0.0345809907026646,0.04));
#48530=CARTESIAN_POINT('',(0.18738691397118,0.0314029373205391,0.04));
#48531=CARTESIAN_POINT('Origin',(0.,0.,0.04));
#48532=CARTESIAN_POINT('',(0.181204626554246,0.0319512646907152,0.04));
#48533=CARTESIAN_POINT('',(0.205594090888895,0.0433597715811408,0.04));
#48534=CARTESIAN_POINT('',(0.181204626554246,0.0319512646907152,0.04));
#48535=CARTESIAN_POINT('Origin',(0.181204626554246,0.0319512646907152,0.04));
#48536=CARTESIAN_POINT('',(0.18738691397118,0.0314029373205391,0.185));
#48537=CARTESIAN_POINT('',(0.18738691397118,0.0314029373205391,0.0925));
#48538=CARTESIAN_POINT('',(0.181204626554246,0.0319512646907152,0.191));
#48539=CARTESIAN_POINT('',(0.181204626554246,0.0319512646907152,0.04));
#48540=CARTESIAN_POINT('Ctrl Pts',(0.18738691397118,0.0314029373205391,
0.185));
#48541=CARTESIAN_POINT('Ctrl Pts',(0.184246179721932,0.0316814993535165,
0.188051499118466));
#48542=CARTESIAN_POINT('Ctrl Pts',(0.181204626554246,0.0319512646907152,
0.191));
#48543=CARTESIAN_POINT('Origin',(0.205594090888895,0.0433597715811408,0.04));
#48544=CARTESIAN_POINT('',(0.186826537413779,0.0345809907026646,0.185));
#48545=CARTESIAN_POINT('',(0.186826537413779,0.0345809907026646,0.0925));
#48546=CARTESIAN_POINT('Ctrl Pts',(0.181204626554246,0.0319512646907152,
0.191));
#48547=CARTESIAN_POINT('Ctrl Pts',(0.183970486442399,0.0332450336377893,
0.18805149911842));
#48548=CARTESIAN_POINT('Ctrl Pts',(0.186826537413779,0.0345809907026646,
0.185));
#48549=CARTESIAN_POINT('Origin',(0.,0.,0.0925));
#48550=CARTESIAN_POINT('Origin',(0.,0.,0.185));
#48551=CARTESIAN_POINT('Origin',(0.,0.,0.185));
#48552=CARTESIAN_POINT('Origin',(0.,0.,0.185));
#48553=CARTESIAN_POINT('Origin',(0.,0.,0.185));
#48554=CARTESIAN_POINT('Origin',(0.,0.,0.185));
#48555=CARTESIAN_POINT('Origin',(0.,0.,0.185));
#48556=CARTESIAN_POINT('Origin',(0.,0.,0.185));
#48557=CARTESIAN_POINT('Origin',(0.,0.,0.185));
#48558=CARTESIAN_POINT('Origin',(0.,0.,0.185));
#48559=CARTESIAN_POINT('Origin',(0.,0.,0.185));
#48560=CARTESIAN_POINT('Origin',(0.,0.,0.185));
#48561=CARTESIAN_POINT('Origin',(0.,0.,0.185));
#48562=CARTESIAN_POINT('Origin',(0.,0.,0.185));
#48563=CARTESIAN_POINT('Origin',(0.,0.,0.185));
#48564=CARTESIAN_POINT('Origin',(0.,0.,0.185));
#48565=CARTESIAN_POINT('Origin',(0.,0.,0.185));
#48566=CARTESIAN_POINT('Origin',(0.,0.,0.185));
#48567=CARTESIAN_POINT('',(-0.19,-2.32682891837997E-17,0.));
#48568=CARTESIAN_POINT('',(-0.19,-2.32682891837997E-17,0.0925));
#48569=CARTESIAN_POINT('Origin',(0.,0.,0.));
#48570=CARTESIAN_POINT('Origin',(0.,0.,0.185));
#48571=CARTESIAN_POINT('Origin',(0.,0.,0.185));
#48572=CARTESIAN_POINT('Origin',(0.,0.,0.185));
#48573=CARTESIAN_POINT('Origin',(0.,0.,0.185));
#48574=CARTESIAN_POINT('Origin',(0.,0.,0.185));
#48575=CARTESIAN_POINT('Origin',(0.,0.,0.185));
#48576=CARTESIAN_POINT('Origin',(0.,0.,0.185));
#48577=CARTESIAN_POINT('Origin',(0.,0.,0.185));
#48578=CARTESIAN_POINT('Origin',(0.,0.,0.185));
#48579=CARTESIAN_POINT('Origin',(0.,0.,0.185));
#48580=CARTESIAN_POINT('Origin',(0.,0.,0.185));
#48581=CARTESIAN_POINT('Origin',(0.,0.,0.185));
#48582=CARTESIAN_POINT('Origin',(0.,0.,0.185));
#48583=CARTESIAN_POINT('Origin',(0.,0.,0.185));
#48584=CARTESIAN_POINT('Origin',(0.,0.,0.185));
#48585=CARTESIAN_POINT('Origin',(0.,0.,0.185));
#48586=CARTESIAN_POINT('Origin',(0.,0.,0.185));
#48587=CARTESIAN_POINT('',(0.18999314853095,0.00161353998910188,0.185));
#48588=CARTESIAN_POINT('Origin',(0.,0.,0.185));
#48589=CARTESIAN_POINT('',(0.18999314853095,0.00161353998910188,0.04));
#48590=CARTESIAN_POINT('',(0.18999314853095,0.00161353998910188,0.0925));
#48591=CARTESIAN_POINT('',(0.18999314853095,-0.00161353998910189,0.04));
#48592=CARTESIAN_POINT('Origin',(0.,0.,0.04));
#48593=CARTESIAN_POINT('',(0.18999314853095,-0.00161353998910189,0.185));
#48594=CARTESIAN_POINT('',(0.18999314853095,-0.00161353998910189,0.0925));
#48595=CARTESIAN_POINT('Origin',(0.,0.,0.185));
#48596=CARTESIAN_POINT('Origin',(0.184,0.,0.04));
#48597=CARTESIAN_POINT('',(0.184,0.,0.04));
#48598=CARTESIAN_POINT('',(0.184,0.,0.04));
#48599=CARTESIAN_POINT('',(0.184,0.,0.191));
#48600=CARTESIAN_POINT('',(0.184,0.,0.04));
#48601=CARTESIAN_POINT('Ctrl Pts',(0.18999314853095,-0.00161353998910188,
0.185));
#48602=CARTESIAN_POINT('Ctrl Pts',(0.186948500881579,-0.000793827160425129,
0.188051499118421));
#48603=CARTESIAN_POINT('Ctrl Pts',(0.184,0.,0.191));
#48604=CARTESIAN_POINT('Origin',(0.21,0.007,0.04));
#48605=CARTESIAN_POINT('Ctrl Pts',(0.184,0.,0.191));
#48606=CARTESIAN_POINT('Ctrl Pts',(0.1869485008816,0.000793827160430761,
0.1880514991184));
#48607=CARTESIAN_POINT('Ctrl Pts',(0.18999314853095,0.00161353998910188,
0.185));
#48608=CARTESIAN_POINT('',(0.21,0.007,0.04));
#48609=CARTESIAN_POINT('Origin',(0.197,0.,0.04));
#48610=CARTESIAN_POINT('Origin',(0.,0.,0.1925));
#48611=CARTESIAN_POINT('',(-0.175,-2.14313189850787E-17,0.2));
#48612=CARTESIAN_POINT('Origin',(0.,0.,0.2));
#48613=CARTESIAN_POINT('',(-0.1825,-2.23498040844392E-17,0.1925));
#48614=CARTESIAN_POINT('Origin',(0.,0.,0.078849364905389));
#48615=CARTESIAN_POINT('',(0.,0.,0.0566987298107781));
#48616=CARTESIAN_POINT('',(-0.0677181486487011,8.29308139868164E-18,0.1));
#48617=CARTESIAN_POINT('',(-0.0346410161513776,-4.24230095489963E-18,0.078849364905389));
#48618=CARTESIAN_POINT('Origin',(0.,0.,0.1));
#48619=CARTESIAN_POINT('Origin',(0.,0.0866025403784439,0.2));
#48620=CARTESIAN_POINT('',(5.30287619362453E-18,0.0866025403784439,0.2));
#48621=CARTESIAN_POINT('',(0.075,0.0433012701892219,0.2));
#48622=CARTESIAN_POINT('',(0.01875,0.0757772228311384,0.2));
#48623=CARTESIAN_POINT('',(0.,0.0866025403784439,0.1));
#48624=CARTESIAN_POINT('',(5.30287619362453E-18,0.0866025403784439,0.2));
#48625=CARTESIAN_POINT('',(0.075,0.0433012701892219,0.1));
#48626=CARTESIAN_POINT('',(0.075,0.0433012701892219,0.1));
#48627=CARTESIAN_POINT('',(0.075,0.0433012701892219,0.2));
#48628=CARTESIAN_POINT('Origin',(-0.075,0.0433012701892219,0.2));
#48629=CARTESIAN_POINT('',(-0.075,0.0433012701892219,0.2));
#48630=CARTESIAN_POINT('',(-0.05625,0.0541265877365274,0.2));
#48631=CARTESIAN_POINT('',(-0.075,0.0433012701892219,0.1));
#48632=CARTESIAN_POINT('',(-0.075,0.0433012701892219,0.2));
#48633=CARTESIAN_POINT('',(5.30287619362453E-18,0.0866025403784439,0.1));
#48634=CARTESIAN_POINT('Origin',(-0.075,-0.0433012701892219,0.2));
#48635=CARTESIAN_POINT('',(-0.075,-0.0433012701892219,0.2));
#48636=CARTESIAN_POINT('',(-0.075,-0.021650635094611,0.2));
#48637=CARTESIAN_POINT('',(-0.075,-0.0433012701892219,0.1));
#48638=CARTESIAN_POINT('',(-0.075,-0.0433012701892219,0.2));
#48639=CARTESIAN_POINT('',(-0.075,0.0433012701892219,0.1));
#48640=CARTESIAN_POINT('Origin',(-1.38777878078145E-17,-0.0866025403784439,
0.2));
#48641=CARTESIAN_POINT('',(-1.59086285808736E-17,-0.0866025403784439,0.2));
#48642=CARTESIAN_POINT('',(-0.01875,-0.0757772228311384,0.2));
#48643=CARTESIAN_POINT('',(-1.38777878078145E-17,-0.0866025403784439,0.1));
#48644=CARTESIAN_POINT('',(-1.59086285808736E-17,-0.0866025403784439,0.2));
#48645=CARTESIAN_POINT('',(-0.075,-0.0433012701892219,0.1));
#48646=CARTESIAN_POINT('Origin',(0.075,-0.043301270189222,0.2));
#48647=CARTESIAN_POINT('',(0.075,-0.043301270189222,0.2));
#48648=CARTESIAN_POINT('',(0.05625,-0.0541265877365275,0.2));
#48649=CARTESIAN_POINT('',(0.075,-0.043301270189222,0.1));
#48650=CARTESIAN_POINT('',(0.075,-0.043301270189222,0.2));
#48651=CARTESIAN_POINT('',(-1.59086285808736E-17,-0.0866025403784439,0.1));
#48652=CARTESIAN_POINT('Origin',(0.075,0.0433012701892219,0.2));
#48653=CARTESIAN_POINT('',(0.075,0.021650635094611,0.2));
#48654=CARTESIAN_POINT('',(0.075,-0.043301270189222,0.1));
#48655=CARTESIAN_POINT('Origin',(0.,0.,0.1));
#48656=CARTESIAN_POINT('Origin',(0.076,0.,-1.));
#48657=CARTESIAN_POINT('',(-0.076,-9.30731567351988E-18,-1.));
#48658=CARTESIAN_POINT('Origin',(0.,0.,-1.));
#48659=CARTESIAN_POINT('Origin',(0.,0.,-0.988));
#48660=CARTESIAN_POINT('',(-0.088,-1.07768918324967E-17,-0.988));
#48661=CARTESIAN_POINT('Origin',(0.,0.,-0.493));
#48662=CARTESIAN_POINT('Origin',(0.,0.,-0.013325));
#48663=CARTESIAN_POINT('Origin',(0.,0.,-0.005));
#48664=CARTESIAN_POINT('',(-0.11,-1.34711147906209E-17,-3.46944695195361E-18));
#48665=CARTESIAN_POINT('Origin',(0.,0.,0.));
#48666=CARTESIAN_POINT('',(-0.105,-1.28587913910472E-17,-0.005));
#48667=CARTESIAN_POINT('Origin',(0.19,0.,0.));
#48668=CARTESIAN_POINT('Origin',(0.,0.,0.2));
#48669=CARTESIAN_POINT('',(0.,0.,0.));
#48670=CARTESIAN_POINT('Origin',(0.,0.,-0.29));
#48671=CARTESIAN_POINT('',(-0.121463520633891,0.000103202980665532,-0.514010734985006));
#48672=CARTESIAN_POINT('',(-0.121467053128752,9.34507928307322E-5,-0.520489265014994));
#48673=CARTESIAN_POINT('',(-0.1215,-1.48794586096403E-17,-0.29));
#48674=CARTESIAN_POINT('',(0.0681458046084935,-0.100801883029113,-0.5435));
#48675=CARTESIAN_POINT('Ctrl Pts',(-0.121463520633891,0.000103202980665532,
-0.514010734985006));
#48676=CARTESIAN_POINT('Ctrl Pts',(-0.121553801365528,0.0106198798703647,
-0.514630387130534));
#48677=CARTESIAN_POINT('Ctrl Pts',(-0.120298811423027,0.0211154705696016,
-0.515250039276062));
#48678=CARTESIAN_POINT('Ctrl Pts',(-0.117612982943742,0.0312312632791946,
-0.515869691421591));
#48679=CARTESIAN_POINT('Ctrl Pts',(-0.107390082218629,0.0697343715095162,
-0.518228234573805));
#48680=CARTESIAN_POINT('Ctrl Pts',(-0.0764379898774561,0.102735178047276,
-0.520586777726019));
#48681=CARTESIAN_POINT('Ctrl Pts',(-0.0386628242561016,0.115388802409532,
-0.522945320878233));
#48682=CARTESIAN_POINT('Ctrl Pts',(-0.000887658634747289,0.128042426771789,
-0.525303864030447));
#48683=CARTESIAN_POINT('Ctrl Pts',(0.0437105802667884,0.120348868958541,
-0.527662407182661));
#48684=CARTESIAN_POINT('Ctrl Pts',(0.075062366606055,0.0957822364039557,
-0.530020950334875));
#48685=CARTESIAN_POINT('Ctrl Pts',(0.106414152945322,0.0712156038493702,
-0.532379493487089));
#48686=CARTESIAN_POINT('Ctrl Pts',(0.124519486722319,0.0297758965534469,
-0.534738036639304));
#48687=CARTESIAN_POINT('Ctrl Pts',(0.121273756374489,-0.00993482915230421,
-0.537096579791518));
#48688=CARTESIAN_POINT('Ctrl Pts',(0.118336381625297,-0.0458728986959281,
-0.539231053194345));
#48689=CARTESIAN_POINT('Ctrl Pts',(0.0979120851199604,-0.0803948999064519,
-0.541365526597173));
#48690=CARTESIAN_POINT('Ctrl Pts',(0.0681458046084935,-0.100801883029113,
-0.5435));
#48691=CARTESIAN_POINT('',(-0.1215,-1.48794586096403E-17,-0.5435));
#48692=CARTESIAN_POINT('Origin',(0.,0.,-0.5435));
#48693=CARTESIAN_POINT('',(-0.1215,-1.48794586096403E-17,-0.5735));
#48694=CARTESIAN_POINT('',(-0.1215,-1.48794586096403E-17,-0.29));
#48695=CARTESIAN_POINT('Origin',(0.,0.,-0.5735));
#48696=CARTESIAN_POINT('',(0.121191192277757,-0.00865707307903507,-0.5435));
#48697=CARTESIAN_POINT('Origin',(0.,0.,-0.5435));
#48698=CARTESIAN_POINT('Ctrl Pts',(0.121191192277757,-0.00865707307903506,
-0.5435));
#48699=CARTESIAN_POINT('Ctrl Pts',(0.12404209412111,0.0312529739205125,
-0.541141456847786));
#48700=CARTESIAN_POINT('Ctrl Pts',(0.10563867747241,0.0723480656890973,
-0.538782913695572));
#48701=CARTESIAN_POINT('Ctrl Pts',(0.0740709879443734,0.0965411452271748,
-0.536424370543358));
#48702=CARTESIAN_POINT('Ctrl Pts',(0.0425032984163362,0.120734224765253,
-0.534065827391144));
#48703=CARTESIAN_POINT('Ctrl Pts',(-0.00222866399103803,0.128025292072823,
-0.53170728423893));
#48704=CARTESIAN_POINT('Ctrl Pts',(-0.039883232720534,0.11499262083988,
-0.529348741086716));
#48705=CARTESIAN_POINT('Ctrl Pts',(-0.07753780145003,0.101959949606938,
-0.526990197934502));
#48706=CARTESIAN_POINT('Ctrl Pts',(-0.108114976501648,0.0686035398334826,
-0.524631654782288));
#48707=CARTESIAN_POINT('Ctrl Pts',(-0.117926982101641,0.0299874699351204,
-0.522273111630074));
#48708=CARTESIAN_POINT('Ctrl Pts',(-0.120400700246994,0.0202519197628043,
-0.521678496091714));
#48709=CARTESIAN_POINT('Ctrl Pts',(-0.121554581285855,0.0101820648492457,
-0.521083880553354));
#48710=CARTESIAN_POINT('Ctrl Pts',(-0.121467053128752,9.34507928307322E-5,
-0.520489265014994));
#48711=CARTESIAN_POINT('Origin',(0.,0.,-0.29));
#48712=CARTESIAN_POINT('',(-0.121354988926872,-7.09400307492836E-5,-0.469010734985006));
#48713=CARTESIAN_POINT('',(-0.121347519425042,-6.58635799960141E-5,-0.475489265014995));
#48714=CARTESIAN_POINT('',(-0.1215,-1.48794586096403E-17,-0.29));
#48715=CARTESIAN_POINT('Ctrl Pts',(-0.121354988926872,-7.09400307492836E-5,
-0.469010734985006));
#48716=CARTESIAN_POINT('Ctrl Pts',(-0.121219195033693,0.0249081254717452,
-0.47047912821725));
#48717=CARTESIAN_POINT('Ctrl Pts',(-0.113699226119619,0.0499622036482225,
-0.471947521449495));
#48718=CARTESIAN_POINT('Ctrl Pts',(-0.0993881694574734,0.0702183410582727,
-0.473415914681739));
#48719=CARTESIAN_POINT('Ctrl Pts',(-0.0764016533456638,0.102753886121886,
-0.475774457833953));
#48720=CARTESIAN_POINT('Ctrl Pts',(-0.0358948086527237,0.12291122288382,
-0.478133000986166));
#48721=CARTESIAN_POINT('Ctrl Pts',(0.00392099239580886,0.121627591643135,
-0.48049154413838));
#48722=CARTESIAN_POINT('Ctrl Pts',(0.0437367934443413,0.12034396040245,
-0.482850087290594));
#48723=CARTESIAN_POINT('Ctrl Pts',(0.0828615508484662,0.0976193611591442,
-0.485208630442808));
#48724=CARTESIAN_POINT('Ctrl Pts',(0.103704668945383,0.0636709283798785,
-0.487567173595023));
#48725=CARTESIAN_POINT('Ctrl Pts',(0.1245477870423,0.0297224956006128,-0.489925716747237));
#48726=CARTESIAN_POINT('Ctrl Pts',(0.127109265832009,-0.0154497707146136,
-0.492284259899451));
#48727=CARTESIAN_POINT('Ctrl Pts',(0.110238229460948,-0.0515373638505048,
-0.494642803051665));
#48728=CARTESIAN_POINT('Ctrl Pts',(0.0933671930898881,-0.0876249569863961,
-0.497001346203878));
#48729=CARTESIAN_POINT('Ctrl Pts',(0.0570636415580583,-0.114627876942952,
-0.499359889356092));
#48730=CARTESIAN_POINT('Ctrl Pts',(0.0176479671399454,-0.120404648237461,
-0.501718432508307));
#48731=CARTESIAN_POINT('Ctrl Pts',(-0.0217677072781677,-0.12618141953197,
-0.504076975660521));
#48732=CARTESIAN_POINT('Ctrl Pts',(-0.0642955045825639,-0.110732042164432,
-0.506435518812735));
#48733=CARTESIAN_POINT('Ctrl Pts',(-0.0908125486802356,-0.0810046485192209,
-0.508794061964949));
#48734=CARTESIAN_POINT('Ctrl Pts',(-0.110362858566254,-0.0590874334734252,
-0.510532952971635));
#48735=CARTESIAN_POINT('Ctrl Pts',(-0.121210171471051,-0.0294090887069978,
-0.51227184397832));
#48736=CARTESIAN_POINT('Ctrl Pts',(-0.121463520633891,0.000103202980665532,
-0.514010734985006));
#48737=CARTESIAN_POINT('Ctrl Pts',(-0.121467053128752,9.34507928307322E-5,
-0.520489265014994));
#48738=CARTESIAN_POINT('Ctrl Pts',(-0.121207400759546,-0.029834433313122,
-0.51872533740114));
#48739=CARTESIAN_POINT('Ctrl Pts',(-0.110023188032426,-0.0599274002854349,
-0.516961409787286));
#48740=CARTESIAN_POINT('Ctrl Pts',(-0.0899618218360895,-0.0819479460585449,
-0.515197482173432));
#48741=CARTESIAN_POINT('Ctrl Pts',(-0.0631378198221754,-0.111391562130578,
-0.512838939021217));
#48742=CARTESIAN_POINT('Ctrl Pts',(-0.0204429796459781,-0.126403064251376,
-0.510480395869004));
#48743=CARTESIAN_POINT('Ctrl Pts',(0.0189116888966024,-0.120215378421974,
-0.508121852716789));
#48744=CARTESIAN_POINT('Ctrl Pts',(0.0582663574391833,-0.114027692592572,
-0.505763309564575));
#48745=CARTESIAN_POINT('Ctrl Pts',(0.0942808543481472,-0.0866408188129685,
-0.503404766412361));
#48746=CARTESIAN_POINT('Ctrl Pts',(0.110771590337775,-0.0503771654710377,
-0.501046223260147));
#48747=CARTESIAN_POINT('Ctrl Pts',(0.127262326327404,-0.0141135121291072,
-0.498687680107933));
#48748=CARTESIAN_POINT('Ctrl Pts',(0.124229301397696,0.031026920775151,
-0.496329136955719));
#48749=CARTESIAN_POINT('Ctrl Pts',(0.103031791863172,0.0647543130122383,
-0.493970593803505));
#48750=CARTESIAN_POINT('Ctrl Pts',(0.0818342823286479,0.0984817052493257,
-0.491612050651291));
#48751=CARTESIAN_POINT('Ctrl Pts',(0.0424722881893066,0.120796056819242,
-0.489253507499077));
#48752=CARTESIAN_POINT('Ctrl Pts',(0.00264496221188506,0.121662374236399,
-0.486894964346863));
#48753=CARTESIAN_POINT('Ctrl Pts',(-0.0371823637655362,0.122528691653556,
-0.484536421194649));
#48754=CARTESIAN_POINT('Ctrl Pts',(-0.0774750215810378,0.101946974917955,
-0.482177878042435));
#48755=CARTESIAN_POINT('Ctrl Pts',(-0.100118934895602,0.0691719947505057,
-0.479819334890221));
#48756=CARTESIAN_POINT('Ctrl Pts',(-0.113976320659153,0.0491147044198212,
-0.478375978265146));
#48757=CARTESIAN_POINT('Ctrl Pts',(-0.121224132521449,0.0244909546593463,
-0.47693262164007));
#48758=CARTESIAN_POINT('Ctrl Pts',(-0.121347519425042,-6.58635799960141E-5,
-0.475489265014995));
#48759=CARTESIAN_POINT('Origin',(0.,0.,-0.29));
#48760=CARTESIAN_POINT('',(-0.121689032810886,-1.25051776863616E-5,-0.424010734985006));
#48761=CARTESIAN_POINT('',(-0.121686438635927,-1.99743996858978E-5,-0.430489265014994));
#48762=CARTESIAN_POINT('',(-0.1215,-1.48794586096403E-17,-0.29));
#48763=CARTESIAN_POINT('Ctrl Pts',(-0.121689032810886,-1.25051776863616E-5,
-0.424010734985006));
#48764=CARTESIAN_POINT('Ctrl Pts',(-0.121630741701287,0.0391259959765282,
-0.426327869303966));
#48765=CARTESIAN_POINT('Ctrl Pts',(-0.101028394996106,0.0783173256670956,
-0.428645003622925));
#48766=CARTESIAN_POINT('Ctrl Pts',(-0.0687315757637827,0.10042212870287,
-0.430962137941885));
#48767=CARTESIAN_POINT('Ctrl Pts',(-0.0358575894715735,0.122921960242402,
-0.4333206810941));
#48768=CARTESIAN_POINT('Ctrl Pts',(0.00913258115290106,0.12771911164248,
-0.435679224246314));
#48769=CARTESIAN_POINT('Ctrl Pts',(0.0460116911221716,0.112656815349134,
-0.438037767398528));
#48770=CARTESIAN_POINT('Ctrl Pts',(0.0828908010914419,0.0975945190557874,
-0.440396310550742));
#48771=CARTESIAN_POINT('Ctrl Pts',(0.111658850405508,0.0626727750690164,
-0.442754853702956));
#48772=CARTESIAN_POINT('Ctrl Pts',(0.119381927578032,0.0235921491730332,
-0.44511339685517));
#48773=CARTESIAN_POINT('Ctrl Pts',(0.127105004750555,-0.01548847672295,
-0.447471940007384));
#48774=CARTESIAN_POINT('Ctrl Pts',(0.113783109781535,-0.0587279845281455,
-0.449830483159598));
#48775=CARTESIAN_POINT('Ctrl Pts',(0.0854056844396275,-0.0866862229885438,
-0.452189026311812));
#48776=CARTESIAN_POINT('Ctrl Pts',(0.05702825909772,-0.114644461448942,
-0.454547569464026));
#48777=CARTESIAN_POINT('Ctrl Pts',(0.0135953033829249,-0.127321430564543,
-0.45690611261624));
#48778=CARTESIAN_POINT('Ctrl Pts',(-0.025366075857601,-0.11901763363164,
-0.459264655768454));
#48779=CARTESIAN_POINT('Ctrl Pts',(-0.064327455098127,-0.110713836698737,
-0.461623198920668));
#48780=CARTESIAN_POINT('Ctrl Pts',(-0.0988172578643837,-0.08142927371733,
-0.463981742072882));
#48781=CARTESIAN_POINT('Ctrl Pts',(-0.113329065482173,-0.0443301155439809,
-0.466340285225096));
#48782=CARTESIAN_POINT('Ctrl Pts',(-0.118806041545752,-0.0303283311594296,
-0.467230435145066));
#48783=CARTESIAN_POINT('Ctrl Pts',(-0.121437308104386,-0.0152134186731973,
-0.468120585065036));
#48784=CARTESIAN_POINT('Ctrl Pts',(-0.121354988926872,-7.09400307492836E-5,
-0.469010734985006));
#48785=CARTESIAN_POINT('Ctrl Pts',(-0.121347519425042,-6.58635799960141E-5,
-0.475489265014995));
#48786=CARTESIAN_POINT('Ctrl Pts',(-0.121425755136045,-0.0156365609472264,
-0.474574078487856));
#48787=CARTESIAN_POINT('Ctrl Pts',(-0.118639669415141,-0.0311803490001526,
-0.473658891960718));
#48788=CARTESIAN_POINT('Ctrl Pts',(-0.112858015223634,-0.0455160728540226,
-0.472743705433579));
#48789=CARTESIAN_POINT('Ctrl Pts',(-0.0979580134234747,-0.0824609166918042,
-0.470385162281365));
#48790=CARTESIAN_POINT('Ctrl Pts',(-0.063162841009528,-0.11138236076807,
-0.46802661912915));
#48791=CARTESIAN_POINT('Ctrl Pts',(-0.0241164856398025,-0.119277153472215,
-0.465668075976936));
#48792=CARTESIAN_POINT('Ctrl Pts',(0.0149298697299233,-0.12717194617636,
-0.463309532824722));
#48793=CARTESIAN_POINT('Ctrl Pts',(0.0582274080554279,-0.114040087508383,
-0.460950989672509));
#48794=CARTESIAN_POINT('Ctrl Pts',(0.0863100510388977,-0.0857857662793123,
-0.458592446520295));
#48795=CARTESIAN_POINT('Ctrl Pts',(0.114392694022367,-0.0575314450502418,
-0.456233903368081));
#48796=CARTESIAN_POINT('Ctrl Pts',(0.127260441663802,-0.0141546612600778,
-0.453875360215866));
#48797=CARTESIAN_POINT('Ctrl Pts',(0.11912795666395,0.0248428088327164,
-0.451516817063652));
#48798=CARTESIAN_POINT('Ctrl Pts',(0.110995471664098,0.0638402789255106,
-0.449158273911438));
#48799=CARTESIAN_POINT('Ctrl Pts',(0.0818627540229589,0.0984584353209352,
-0.446799730759224));
#48800=CARTESIAN_POINT('Ctrl Pts',(0.0448277078769713,0.113133153866057,
-0.44444118760701));
#48801=CARTESIAN_POINT('Ctrl Pts',(0.00779266173098367,0.127807872411178,
-0.442082644454797));
#48802=CARTESIAN_POINT('Ctrl Pts',(-0.0371447129198525,0.122539153105997,
-0.439724101302582));
#48803=CARTESIAN_POINT('Ctrl Pts',(-0.0697809290729632,0.0996958028250744,
-0.437365558150368));
#48804=CARTESIAN_POINT('Ctrl Pts',(-0.101497709957742,0.0774960008585949,
-0.435073460438577));
#48805=CARTESIAN_POINT('Ctrl Pts',(-0.121596671566893,0.0386978527648168,
-0.432781362726786));
#48806=CARTESIAN_POINT('Ctrl Pts',(-0.121686438635927,-1.99743996858978E-5,
-0.430489265014994));
#48807=CARTESIAN_POINT('Origin',(0.,0.,-0.29));
#48808=CARTESIAN_POINT('',(-0.121383410361094,8.5849798153903E-5,-0.379010734985006));
#48809=CARTESIAN_POINT('',(-0.121393079482962,8.9638819514881E-5,-0.385489265014994));
#48810=CARTESIAN_POINT('',(-0.1215,-1.48794586096403E-17,-0.29));
#48811=CARTESIAN_POINT('Ctrl Pts',(-0.121383410361094,8.5849798153903E-5,
-0.379010734985006));
#48812=CARTESIAN_POINT('Ctrl Pts',(-0.121475175728008,0.0138114136519433,
-0.379818067238468));
#48813=CARTESIAN_POINT('Ctrl Pts',(-0.119322368561901,0.0275090559256997,
-0.380625399491929));
#48814=CARTESIAN_POINT('Ctrl Pts',(-0.114798393001489,0.0403727954403562,
-0.381432731745391));
#48815=CARTESIAN_POINT('Ctrl Pts',(-0.101582035630596,0.0779529671900597,
-0.383791274897605));
#48816=CARTESIAN_POINT('Ctrl Pts',(-0.0681287102894151,0.108416114494445,
-0.386149818049819));
#48817=CARTESIAN_POINT('Ctrl Pts',(-0.0294787857423598,0.118066230703992,
-0.388508361202033));
#48818=CARTESIAN_POINT('Ctrl Pts',(0.00917113880469548,0.127716346913539,
-0.390866904354247));
#48819=CARTESIAN_POINT('Ctrl Pts',(0.0530176625576257,0.116553432028247,
-0.393225447506461));
#48820=CARTESIAN_POINT('Ctrl Pts',(0.0823477114274472,0.0895962502971781,
-0.395583990658675));
#48821=CARTESIAN_POINT('Ctrl Pts',(0.111677760297269,0.0626390685661086,
-0.397942533810889));
#48822=CARTESIAN_POINT('Ctrl Pts',(0.126491334283982,0.0198876199892615,
-0.400301076963103));
#48823=CARTESIAN_POINT('Ctrl Pts',(0.120128359435606,-0.0194373588391155,
-0.402659620115317));
#48824=CARTESIAN_POINT('Ctrl Pts',(0.11376538458723,-0.0587623376674924,
-0.405018163267531));
#48825=CARTESIAN_POINT('Ctrl Pts',(0.0862258609037655,-0.0946608467473989,
-0.407376706419745));
#48826=CARTESIAN_POINT('Ctrl Pts',(0.049891355764218,-0.110993181039425,
-0.409735249571959));
#48827=CARTESIAN_POINT('Ctrl Pts',(0.0135568506246707,-0.127325515331451,
-0.412093792724173));
#48828=CARTESIAN_POINT('Ctrl Pts',(-0.0315726359709597,-0.124091674835596,
-0.414452335876387));
#48829=CARTESIAN_POINT('Ctrl Pts',(-0.0652072198369896,-0.102745569896818,
-0.416810879028601));
#48830=CARTESIAN_POINT('Ctrl Pts',(-0.0988418037030196,-0.0813994649580399,
-0.419169422180815));
#48831=CARTESIAN_POINT('Ctrl Pts',(-0.120981484839449,-0.0419410955763378,
-0.421527965333029));
#48832=CARTESIAN_POINT('Ctrl Pts',(-0.121672424427692,-0.00211065504599355,
-0.423886508485243));
#48833=CARTESIAN_POINT('Ctrl Pts',(-0.12168455522215,-0.00141135384015577,
-0.423927917318497));
#48834=CARTESIAN_POINT('Ctrl Pts',(-0.121690074514347,-0.000711937944640976,
-0.423969326151752));
#48835=CARTESIAN_POINT('Ctrl Pts',(-0.121689032810886,-1.25051776863616E-5,
-0.424010734985006));
#48836=CARTESIAN_POINT('Ctrl Pts',(-0.121686438635927,-1.99743996858978E-5,
-0.430489265014994));
#48837=CARTESIAN_POINT('Ctrl Pts',(-0.121689040886436,-0.00114236244838274,
-0.430422819574572));
#48838=CARTESIAN_POINT('Ctrl Pts',(-0.121674828258958,-0.0022646829987791,
-0.430356374134149));
#48839=CARTESIAN_POINT('Ctrl Pts',(-0.121643596330701,-0.00338652974087634,
-0.430289928693726));
#48840=CARTESIAN_POINT('Ctrl Pts',(-0.120534989779944,-0.0432075307692407,
-0.427931385541512));
#48841=CARTESIAN_POINT('Ctrl Pts',(-0.0979827190230435,-0.0824315515693056,
-0.425572842389298));
#48842=CARTESIAN_POINT('Ctrl Pts',(-0.0641261260412589,-0.103423753071392,
-0.423214299237084));
#48843=CARTESIAN_POINT('Ctrl Pts',(-0.030269533059474,-0.124415954573479,
-0.42085575608487));
#48844=CARTESIAN_POINT('Ctrl Pts',(0.0148913821471955,-0.127176336777588,
-0.418497212932656));
#48845=CARTESIAN_POINT('Ctrl Pts',(0.051052608431988,-0.110463856476749,
-0.416138669780442));
#48846=CARTESIAN_POINT('Ctrl Pts',(0.0872138347167803,-0.0937513761759113,
-0.413780126628228));
#48847=CARTESIAN_POINT('Ctrl Pts',(0.114375372079696,-0.0575660333701267,
-0.411421583476013));
#48848=CARTESIAN_POINT('Ctrl Pts',(0.120325591369617,-0.0181764894408694,
-0.409063040323799));
#48849=CARTESIAN_POINT('Ctrl Pts',(0.126275810659539,0.0212130544883879,
-0.406704497171585));
#48850=CARTESIAN_POINT('Ctrl Pts',(0.111014711876466,0.0638067995411181,
-0.404345954019372));
#48851=CARTESIAN_POINT('Ctrl Pts',(0.0814035736878408,0.0904549104188703,
-0.401987410867158));
#48852=CARTESIAN_POINT('Ctrl Pts',(0.0517924354992152,0.117103021296623,
-0.399628867714944));
#48853=CARTESIAN_POINT('Ctrl Pts',(0.00783125790503672,0.127805497999397,
-0.397270324562729));
#48854=CARTESIAN_POINT('Ctrl Pts',(-0.0307153379373213,0.117750586445704,
-0.394911781410515));
#48855=CARTESIAN_POINT('Ctrl Pts',(-0.0692619337796792,0.107695674892012,
-0.392553238258301));
#48856=CARTESIAN_POINT('Ctrl Pts',(-0.102393947870216,0.0768833750818523,
-0.390194695106087));
#48857=CARTESIAN_POINT('Ctrl Pts',(-0.115215470377363,0.0391666697696868,
-0.387836151953873));
#48858=CARTESIAN_POINT('Ctrl Pts',(-0.119468189360593,0.0266565682137656,
-0.38705385630758));
#48859=CARTESIAN_POINT('Ctrl Pts',(-0.121486437931333,0.0133868745156882,
-0.386271560661287));
#48860=CARTESIAN_POINT('Ctrl Pts',(-0.121393079482962,8.9638819514881E-5,
-0.385489265014994));
#48861=CARTESIAN_POINT('Origin',(0.,0.,-0.29));
#48862=CARTESIAN_POINT('',(-0.121426763094784,-9.9191016992628E-5,-0.334010734985006));
#48863=CARTESIAN_POINT('',(-0.121415770900973,-9.66275040455964E-5,-0.340489265014995));
#48864=CARTESIAN_POINT('',(-0.1215,-1.48794586096403E-17,-0.29));
#48865=CARTESIAN_POINT('Ctrl Pts',(-0.121426763094784,-9.9191016992628E-5,
-0.334010734985006));
#48866=CARTESIAN_POINT('Ctrl Pts',(-0.121203576807245,0.0280304944041191,
-0.335666808325183));
#48867=CARTESIAN_POINT('Ctrl Pts',(-0.111451175585138,0.0562998709178246,
-0.337322881665361));
#48868=CARTESIAN_POINT('Ctrl Pts',(-0.0935666813062145,0.0778068749824484,
-0.338978955005538));
#48869=CARTESIAN_POINT('Ctrl Pts',(-0.0680959787177338,0.108436676169773,
-0.341337498157752));
#48870=CARTESIAN_POINT('Ctrl Pts',(-0.0261310911381096,0.125350473202342,
-0.343696041309966));
#48871=CARTESIAN_POINT('Ctrl Pts',(0.0134608770154306,0.120943947492484,
-0.34605458446218));
#48872=CARTESIAN_POINT('Ctrl Pts',(0.0530528451689708,0.116537421782626,
-0.348413127614394));
#48873=CARTESIAN_POINT('Ctrl Pts',(0.0902718938964271,0.0908105733303415,
-0.350771670766608));
#48874=CARTESIAN_POINT('Ctrl Pts',(0.10838461298205,0.0553300037393775,
-0.353130213918822));
#48875=CARTESIAN_POINT('Ctrl Pts',(0.126497332067673,0.0198494341484135,
-0.355488757071036));
#48876=CARTESIAN_POINT('Ctrl Pts',(0.125503721511462,-0.02538485658123,
-0.35784730022325));
#48877=CARTESIAN_POINT('Ctrl Pts',(0.105850501298503,-0.0600358644506952,
-0.360205843375464));
#48878=CARTESIAN_POINT('Ctrl Pts',(0.0861972810855425,-0.0946868723201607,
-0.362564386527678));
#48879=CARTESIAN_POINT('Ctrl Pts',(0.0478844512158326,-0.118754597329448,
-0.364922929679892));
#48880=CARTESIAN_POINT('Ctrl Pts',(0.00813717786102508,-0.121418367560867,
-0.367281472832106));
#48881=CARTESIAN_POINT('Ctrl Pts',(-0.0316100954937825,-0.124082137792286,
-0.369640015984321));
#48882=CARTESIAN_POINT('Ctrl Pts',(-0.0727918123336877,-0.105341953245838,
-0.371998559136535));
#48883=CARTESIAN_POINT('Ctrl Pts',(-0.0968929760533375,-0.0736232628751029,
-0.374357102288749));
#48884=CARTESIAN_POINT('Ctrl Pts',(-0.112744281465937,-0.0527619196552203,
-0.375908313187501));
#48885=CARTESIAN_POINT('Ctrl Pts',(-0.12120709207742,-0.0262864946117645,
-0.377459524086254));
#48886=CARTESIAN_POINT('Ctrl Pts',(-0.121383410361094,8.5849798153903E-5,
-0.379010734985006));
#48887=CARTESIAN_POINT('Ctrl Pts',(-0.121393079482962,8.9638819514881E-5,
-0.385489265014994));
#48888=CARTESIAN_POINT('Ctrl Pts',(-0.121204971544359,-0.0267029615241794,
-0.383913017509073));
#48889=CARTESIAN_POINT('Ctrl Pts',(-0.112444114863846,-0.0536073774791074,
-0.382336770003152));
#48890=CARTESIAN_POINT('Ctrl Pts',(-0.0961155486467309,-0.0746353396772124,
-0.380760522497231));
#48891=CARTESIAN_POINT('Ctrl Pts',(-0.0716830734851945,-0.106099532997775,
-0.378401979345017));
#48892=CARTESIAN_POINT('Ctrl Pts',(-0.0303070922383648,-0.124406808824729,
-0.376043436192803));
#48893=CARTESIAN_POINT('Ctrl Pts',(0.00941005870800238,-0.121326350857264,
-0.373684893040589));
#48894=CARTESIAN_POINT('Ctrl Pts',(0.0491272096543692,-0.118245892889799,
-0.371326349888375));
#48895=CARTESIAN_POINT('Ctrl Pts',(0.0871855303002735,-0.0937777011279164,
-0.368967806736161));
#48896=CARTESIAN_POINT('Ctrl Pts',(0.106474279911884,-0.0589224943497298,
-0.366609263583947));
#48897=CARTESIAN_POINT('Ctrl Pts',(0.125763029523496,-0.0240672875715429,
-0.364250720431733));
#48898=CARTESIAN_POINT('Ctrl Pts',(0.126282208100813,0.0211749342229483,
-0.361892177279519));
#48899=CARTESIAN_POINT('Ctrl Pts',(0.107798396801026,0.0564636012642046,
-0.359533634127305));
#48900=CARTESIAN_POINT('Ctrl Pts',(0.0893145855012401,0.0917522683054609,
-0.357175090975091));
#48901=CARTESIAN_POINT('Ctrl Pts',(0.0518277843243512,0.117087380593482,
-0.354816547822877));
#48902=CARTESIAN_POINT('Ctrl Pts',(0.0121917830058918,0.121078458230895,
-0.352458004670663));
#48903=CARTESIAN_POINT('Ctrl Pts',(-0.0274442183125677,0.125069535868307,
-0.350099461518449));
#48904=CARTESIAN_POINT('Ctrl Pts',(-0.0692294197725976,0.107716578855109,
-0.347740918366234));
#48905=CARTESIAN_POINT('Ctrl Pts',(-0.0943775025079859,0.076821348865989,
-0.34538237521402));
#48906=CARTESIAN_POINT('Ctrl Pts',(-0.111768512152077,0.0554559331263187,
-0.343751338481012));
#48907=CARTESIAN_POINT('Ctrl Pts',(-0.121203097283924,0.0276141512297166,
-0.342120301748003));
#48908=CARTESIAN_POINT('Ctrl Pts',(-0.121415770900973,-9.66275040455964E-5,
-0.340489265014995));
#48909=CARTESIAN_POINT('Origin',(0.,0.,-0.29));
#48910=CARTESIAN_POINT('',(-0.121671190739018,4.27946393402705E-5,-0.289010734985006));
#48911=CARTESIAN_POINT('',(-0.12167703567116,3.58475784977506E-5,-0.295489265014995));
#48912=CARTESIAN_POINT('',(-0.1215,-1.48794586096403E-17,-0.29));
#48913=CARTESIAN_POINT('Ctrl Pts',(-0.121671190739018,4.27946393402705E-5,
-0.289010734985006));
#48914=CARTESIAN_POINT('Ctrl Pts',(-0.121682586494413,0.00251441956358687,
-0.289157006259685));
#48915=CARTESIAN_POINT('Ctrl Pts',(-0.121613663427898,0.00498539735850438,
-0.289303277534364));
#48916=CARTESIAN_POINT('Ctrl Pts',(-0.121462386894709,0.00745132303565125,
-0.289449548809043));
#48917=CARTESIAN_POINT('Ctrl Pts',(-0.119023136725957,0.0472130064725989,
-0.291808091961257));
#48918=CARTESIAN_POINT('Ctrl Pts',(-0.0951721719288084,0.0856611507430487,
-0.294166635113471));
#48919=CARTESIAN_POINT('Ctrl Pts',(-0.0606327106317513,0.105509753324465,
-0.296525178265685));
#48920=CARTESIAN_POINT('Ctrl Pts',(-0.0260932493346944,0.125358355905882,
-0.298883721417899));
#48921=CARTESIAN_POINT('Ctrl Pts',(0.0191347084622706,0.126607416798265,
-0.301242264570113));
#48922=CARTESIAN_POINT('Ctrl Pts',(0.0547170060032727,0.108695367422808,
-0.303600807722327));
#48923=CARTESIAN_POINT('Ctrl Pts',(0.0902993035442753,0.0907833180473516,
-0.305959350874541));
#48924=CARTESIAN_POINT('Ctrl Pts',(0.116235940829315,0.0537101584040538,
-0.308317894026755));
#48925=CARTESIAN_POINT('Ctrl Pts',(0.120865996738776,0.0141437080527541,
-0.310676437178969));
#48926=CARTESIAN_POINT('Ctrl Pts',(0.125496052648237,-0.0254227422985456,
-0.313034980331183));
#48927=CARTESIAN_POINT('Ctrl Pts',(0.10881952718212,-0.0674824833578473,
-0.315393523483397));
#48928=CARTESIAN_POINT('Ctrl Pts',(0.078334063379927,-0.0931257652829706,
-0.317752066635612));
#48929=CARTESIAN_POINT('Ctrl Pts',(0.0478485995777338,-0.118769047208094,
-0.320110609787826));
#48930=CARTESIAN_POINT('Ctrl Pts',(0.00355419743946411,-0.127995869999039,
-0.32246915294004));
#48931=CARTESIAN_POINT('Ctrl Pts',(-0.0346347060280981,-0.116657922077687,
-0.324827696092254));
#48932=CARTESIAN_POINT('Ctrl Pts',(-0.0728236094956603,-0.105319974156336,
-0.327186239244468));
#48933=CARTESIAN_POINT('Ctrl Pts',(-0.104907014292515,-0.0734172555226875,
-0.329544782396682));
#48934=CARTESIAN_POINT('Ctrl Pts',(-0.116460457892274,-0.0352929935348227,
-0.331903325548896));
#48935=CARTESIAN_POINT('Ctrl Pts',(-0.119901541998062,-0.0239380420142126,
-0.332605795360932));
#48936=CARTESIAN_POINT('Ctrl Pts',(-0.121521433799066,-0.0120311836111781,
-0.333308265172969));
#48937=CARTESIAN_POINT('Ctrl Pts',(-0.121426763094784,-9.9191016992628E-5,
-0.334010734985006));
#48938=CARTESIAN_POINT('Ctrl Pts',(-0.121415770900973,-9.66275040455964E-5,
-0.340489265014995));
#48939=CARTESIAN_POINT('Ctrl Pts',(-0.121510631683975,-0.012456722774741,
-0.339761758595789));
#48940=CARTESIAN_POINT('Ctrl Pts',(-0.119770783742297,-0.0247907548322472,
-0.339034252176584));
#48941=CARTESIAN_POINT('Ctrl Pts',(-0.116083927801042,-0.0365123859409015,
-0.338306745757379));
#48942=CARTESIAN_POINT('Ctrl Pts',(-0.104131306347963,-0.0745133877936318,
-0.335948202605165));
#48943=CARTESIAN_POINT('Ctrl Pts',(-0.0717150994310587,-0.106077888534051,
-0.33358965945295));
#48944=CARTESIAN_POINT('Ctrl Pts',(-0.0334093949576405,-0.117014721079873,
-0.331231116300736));
#48945=CARTESIAN_POINT('Ctrl Pts',(0.00489630951577786,-0.127951553625695,
-0.328872573148522));
#48946=CARTESIAN_POINT('Ctrl Pts',(0.0490915115457099,-0.11826071797692,
-0.326514029996308));
#48947=CARTESIAN_POINT('Ctrl Pts',(0.0793063737628009,-0.0922991424745387,
-0.324155486844094));
#48948=CARTESIAN_POINT('Ctrl Pts',(0.109521235979892,-0.0663375669721578,
-0.32179694369188));
#48949=CARTESIAN_POINT('Ctrl Pts',(0.125755758384142,-0.0241052516161715,
-0.319438400539666));
#48950=CARTESIAN_POINT('Ctrl Pts',(0.12071101925804,0.0154104656178542,
-0.317079857387452));
#48951=CARTESIAN_POINT('Ctrl Pts',(0.115666280131938,0.0549261828518797,
-0.314721314235238));
#48952=CARTESIAN_POINT('Ctrl Pts',(0.0893422794754841,0.0917253019639447,
-0.312362771083024));
#48953=CARTESIAN_POINT('Ctrl Pts',(0.0535740941272359,0.109263209999201,
-0.31000422793081));
#48954=CARTESIAN_POINT('Ctrl Pts',(0.0178059087789875,0.126801118034458,
-0.307645684778596));
#48955=CARTESIAN_POINT('Ctrl Pts',(-0.0274064612610546,0.125077814992907,
-0.305287141626382));
#48956=CARTESIAN_POINT('Ctrl Pts',(-0.0617358673776313,0.104868085231056,
-0.302928598474168));
#48957=CARTESIAN_POINT('Ctrl Pts',(-0.0960652734942078,0.0846583554692045,
-0.300570055321954));
#48958=CARTESIAN_POINT('Ctrl Pts',(-0.119511715687319,0.0459621989870536,
-0.29821151216974));
#48959=CARTESIAN_POINT('Ctrl Pts',(-0.121533846212305,0.00617712277116327,
-0.295852969017526));
#48960=CARTESIAN_POINT('Ctrl Pts',(-0.121637788479221,0.00413207624217357,
-0.295731734350015));
#48961=CARTESIAN_POINT('Ctrl Pts',(-0.121685123389425,0.00208415256740887,
-0.295610499682505));
#48962=CARTESIAN_POINT('Ctrl Pts',(-0.12167703567116,3.58475784977506E-5,
-0.295489265014995));
#48963=CARTESIAN_POINT('Origin',(0.,0.,-0.29));
#48964=CARTESIAN_POINT('',(-0.121328086182402,4.76889891967633E-5,-0.244010734985006));
#48965=CARTESIAN_POINT('',(-0.121333512465724,5.36033326936202E-5,-0.250489265014994));
#48966=CARTESIAN_POINT('',(-0.1215,-1.48794586096403E-17,-0.29));
#48967=CARTESIAN_POINT('Ctrl Pts',(-0.121328086182402,4.76889891967633E-5,
-0.244010734985006));
#48968=CARTESIAN_POINT('Ctrl Pts',(-0.121389094799374,0.0169834435373647,
-0.245005747346401));
#48969=CARTESIAN_POINT('Ctrl Pts',(-0.118076715360543,0.0338963940472306,
-0.246000759707796));
#48970=CARTESIAN_POINT('Ctrl Pts',(-0.111273178531525,0.0492637126557456,
-0.24699577206919));
#48971=CARTESIAN_POINT('Ctrl Pts',(-0.0951463083322207,0.085689877272637,
-0.249354315221404));
#48972=CARTESIAN_POINT('Ctrl Pts',(-0.0594039044238847,0.113431702779544,
-0.251712858373618));
#48973=CARTESIAN_POINT('Ctrl Pts',(-0.0201154883879651,0.120016668725902,
-0.254071401525832));
#48974=CARTESIAN_POINT('Ctrl Pts',(0.0191729276479541,0.126601634672261,
-0.256429944678046));
#48975=CARTESIAN_POINT('Ctrl Pts',(0.0620073558114569,0.112029741058072,
-0.25878848783026));
#48976=CARTESIAN_POINT('Ctrl Pts',(0.0891297526433666,0.0828524039414163,
-0.261147030982474));
#48977=CARTESIAN_POINT('Ctrl Pts',(0.116252149475276,0.0536750668247602,
-0.263505574134689));
#48978=CARTESIAN_POINT('Ctrl Pts',(0.127662514975593,0.00989228620563701,
-0.265864117286902));
#48979=CARTESIAN_POINT('Ctrl Pts',(0.118230832844077,-0.028811522176682,
-0.268222660439116));
#48980=CARTESIAN_POINT('Ctrl Pts',(0.108799150712561,-0.067515330559001,
-0.270581203591331));
#48981=CARTESIAN_POINT('Ctrl Pts',(0.0785254209492124,-0.101140166704516,
-0.272939746743545));
#48982=CARTESIAN_POINT('Ctrl Pts',(0.0410204895125326,-0.114568551903633,
-0.275298289895759));
#48983=CARTESIAN_POINT('Ctrl Pts',(0.00351555807585251,-0.12799693710275,
-0.277656833047973));
#48984=CARTESIAN_POINT('Ctrl Pts',(-0.0412205750341589,-0.121228871355469,
-0.280015376200187));
#48985=CARTESIAN_POINT('Ctrl Pts',(-0.0730748738189873,-0.0973072271801054,
-0.282373919352401));
#48986=CARTESIAN_POINT('Ctrl Pts',(-0.102953644243061,-0.0748691468660444,
-0.284586191229936));
#48987=CARTESIAN_POINT('Ctrl Pts',(-0.121498836261088,-0.0373391610708751,
-0.286798463107471));
#48988=CARTESIAN_POINT('Ctrl Pts',(-0.121671190739018,4.27946393402705E-5,
-0.289010734985006));
#48989=CARTESIAN_POINT('Ctrl Pts',(-0.12167703567116,3.58475784977506E-5,
-0.295489265014995));
#48990=CARTESIAN_POINT('Ctrl Pts',(-0.121527781987638,-0.0377643149085251,
-0.293251956530291));
#48991=CARTESIAN_POINT('Ctrl Pts',(-0.102503604523412,-0.0756943390720712,
-0.291014648045587));
#48992=CARTESIAN_POINT('Ctrl Pts',(-0.0720503805424354,-0.0980682175048509,
-0.288777339560883));
#48993=CARTESIAN_POINT('Ctrl Pts',(-0.0399469654907172,-0.121654485615344,
-0.286418796408669));
#48994=CARTESIAN_POINT('Ctrl Pts',(0.00485768346958088,-0.127953025886699,
-0.284060253256455));
#48995=CARTESIAN_POINT('Ctrl Pts',(0.0422197261182076,-0.114132060996872,
-0.281701710104241));
#48996=CARTESIAN_POINT('Ctrl Pts',(0.0795817687668341,-0.100311096107045,
-0.279343166952027));
#48997=CARTESIAN_POINT('Ctrl Pts',(0.109501205103789,-0.0663706260560358,
-0.276984623799813));
#48998=CARTESIAN_POINT('Ctrl Pts',(0.118526476885983,-0.0275700362329285,
-0.274626080647599));
#48999=CARTESIAN_POINT('Ctrl Pts',(0.127551748668178,0.011230553590179,
-0.272267537495385));
#49000=CARTESIAN_POINT('Ctrl Pts',(0.115682855895611,0.0548912631853853,
-0.269908994343171));
#49001=CARTESIAN_POINT('Ctrl Pts',(0.0882559653534158,0.0837825590467683,
-0.267550451190957));
#49002=CARTESIAN_POINT('Ctrl Pts',(0.0608290748112208,0.112673854908151,
-0.265191908038743));
#49003=CARTESIAN_POINT('Ctrl Pts',(0.017844186499398,0.126795737035712,
-0.262833364886529));
#49004=CARTESIAN_POINT('Ctrl Pts',(-0.0213730103482152,0.11979911122185,
-0.260474821734315));
#49005=CARTESIAN_POINT('Ctrl Pts',(-0.0605902071958284,0.112802485407989,
-0.258116278582101));
#49006=CARTESIAN_POINT('Ctrl Pts',(-0.0960397125792319,0.0846873516527053,
-0.255757735429887));
#49007=CARTESIAN_POINT('Ctrl Pts',(-0.111783689936811,0.0480940670457318,
-0.253399192277673));
#49008=CARTESIAN_POINT('Ctrl Pts',(-0.118258566725731,0.0330446926881158,
-0.252429216523447));
#49009=CARTESIAN_POINT('Ctrl Pts',(-0.121400544301244,0.0165613642508264,
-0.251459240769221));
#49010=CARTESIAN_POINT('Ctrl Pts',(-0.121333512465724,5.36033326936202E-5,
-0.250489265014994));
#49011=CARTESIAN_POINT('Origin',(0.,0.,-0.29));
#49012=CARTESIAN_POINT('',(-0.121516972739373,-0.000104509287172358,-0.199010734985006));
#49013=CARTESIAN_POINT('',(-0.121504492117652,-0.000105281444988491,-0.205489265014994));
#49014=CARTESIAN_POINT('',(-0.1215,-1.48794586096403E-17,-0.29));
#49015=CARTESIAN_POINT('Ctrl Pts',(-0.121516972739373,-0.000104509287172358,
-0.199010734985006));
#49016=CARTESIAN_POINT('Ctrl Pts',(-0.121237398482098,0.0311537138205197,
-0.200854488433116));
#49017=CARTESIAN_POINT('Ctrl Pts',(-0.108897454112275,0.0626080735884432,
-0.202698241881227));
#49018=CARTESIAN_POINT('Ctrl Pts',(-0.0871671833886449,0.0849147559896284,
-0.204541995329337));
#49019=CARTESIAN_POINT('Ctrl Pts',(-0.0593696591244869,0.113449630367679,
-0.206900538481551));
#49020=CARTESIAN_POINT('Ctrl Pts',(-0.0162060704891954,0.127015504311929,
-0.209259081633765));
#49021=CARTESIAN_POINT('Ctrl Pts',(0.0229175509337778,0.119513260790107,
-0.211617624785979));
#49022=CARTESIAN_POINT('Ctrl Pts',(0.0620411723567516,0.112011017268286,
-0.213976167938193));
#49023=CARTESIAN_POINT('Ctrl Pts',(0.0971248265674069,0.083440656280392,
-0.216334711090408));
#49024=CARTESIAN_POINT('Ctrl Pts',(0.112395160997276,0.0466472017324166,
-0.218693254242622));
#49025=CARTESIAN_POINT('Ctrl Pts',(0.127665495427144,0.00985374718444192,
-0.221051797394836));
#49026=CARTESIAN_POINT('Ctrl Pts',(0.123122510076227,-0.0351628009236139,
-0.22341034054705));
#49027=CARTESIAN_POINT('Ctrl Pts',(0.100808697702601,-0.0681633340777489,
-0.225768883699264));
#49028=CARTESIAN_POINT('Ctrl Pts',(0.078494885328975,-0.101163867231884,
-0.228127426851478));
#49029=CARTESIAN_POINT('Ctrl Pts',(0.0384102459326391,-0.122148385432099,
-0.230485970003692));
#49030=CARTESIAN_POINT('Ctrl Pts',(-0.00142346180680877,-0.121682403829303,
-0.232844513155906));
#49031=CARTESIAN_POINT('Ctrl Pts',(-0.0412571695462569,-0.121216422226508,
-0.23520305630812));
#49032=CARTESIAN_POINT('Ctrl Pts',(-0.080839945628817,-0.099299940820702,
-0.237561599460334));
#49033=CARTESIAN_POINT('Ctrl Pts',(-0.10237566542496,-0.0657864482543611,
-0.239920142612548));
#49034=CARTESIAN_POINT('Ctrl Pts',(-0.114825985452785,-0.046411488343535,
-0.241283673403367));
#49035=CARTESIAN_POINT('Ctrl Pts',(-0.121244482067543,-0.0231604878015092,
-0.242647204194187));
#49036=CARTESIAN_POINT('Ctrl Pts',(-0.121328086182402,4.76889891967633E-5,
-0.244010734985006));
#49037=CARTESIAN_POINT('Ctrl Pts',(-0.121333512465724,5.36033326936202E-5,
-0.250489265014994));
#49038=CARTESIAN_POINT('Ctrl Pts',(-0.121237553137851,-0.0235780581029944,
-0.249100697617007));
#49039=CARTESIAN_POINT('Ctrl Pts',(-0.114565270411393,-0.0472597897861873,
-0.247712130219019));
#49040=CARTESIAN_POINT('Ctrl Pts',(-0.101680121938708,-0.0668564538650969,
-0.246323562821031));
#49041=CARTESIAN_POINT('Ctrl Pts',(-0.0797941272512696,-0.100142254710288,
-0.243965019668817));
#49042=CARTESIAN_POINT('Ctrl Pts',(-0.0399836885446386,-0.121642420942007,
-0.241606476516603));
#49043=CARTESIAN_POINT('Ctrl Pts',(-0.000147285887556907,-0.121690636154816,
-0.239247933364389));
#49044=CARTESIAN_POINT('Ctrl Pts',(0.0396891167695248,-0.121738851367624,
-0.236889390212175));
#49045=CARTESIAN_POINT('Ctrl Pts',(0.0795514833770574,-0.100335115561522,
-0.234530847059961));
#49046=CARTESIAN_POINT('Ctrl Pts',(0.101517987464407,-0.06710239073282,
-0.232172303907747));
#49047=CARTESIAN_POINT('Ctrl Pts',(0.123484491551756,-0.033869665904118,
-0.229813760755532));
#49048=CARTESIAN_POINT('Ctrl Pts',(0.127555133118923,0.0111920479471833,
-0.227455217603318));
#49049=CARTESIAN_POINT('Ctrl Pts',(0.111899781694571,0.0478233361193179,
-0.225096674451104));
#49050=CARTESIAN_POINT('Ctrl Pts',(0.0962444302702202,0.0844546242914523,
-0.22273813129889));
#49051=CARTESIAN_POINT('Ctrl Pts',(0.0608630858543512,0.11265548678442,
-0.220379588146676));
#49052=CARTESIAN_POINT('Ctrl Pts',(0.021662940339392,0.119747023498675,
-0.218021044994462));
#49053=CARTESIAN_POINT('Ctrl Pts',(-0.0175372051755671,0.12683856021293,
-0.215662501842248));
#49054=CARTESIAN_POINT('Ctrl Pts',(-0.0605561517896168,0.112820771148474,
-0.213303958690034));
#49055=CARTESIAN_POINT('Ctrl Pts',(-0.0880528979067979,0.0839959510396251,
-0.21094541553782));
#49056=CARTESIAN_POINT('Ctrl Pts',(-0.109256154326964,0.0617685918667089,
-0.209126698696878));
#49057=CARTESIAN_POINT('Ctrl Pts',(-0.121229535898851,0.0307366148535648,
-0.207307981855936));
#49058=CARTESIAN_POINT('Ctrl Pts',(-0.121504492117652,-0.000105281444988491,
-0.205489265014994));
#49059=CARTESIAN_POINT('Origin',(0.,0.,-0.29));
#49060=CARTESIAN_POINT('',(-0.121603817730479,8.52412621186009E-5,-0.154010734985006));
#49061=CARTESIAN_POINT('',(-0.12161467894854,8.07629804098239E-5,-0.160489265014994));
#49062=CARTESIAN_POINT('',(-0.1215,-1.48794586096403E-17,-0.29));
#49063=CARTESIAN_POINT('Ctrl Pts',(-0.121603817730479,8.52412621186009E-5,
-0.154010734985006));
#49064=CARTESIAN_POINT('Ctrl Pts',(-0.121649091313963,0.00573644262637322,
-0.154344686367618));
#49065=CARTESIAN_POINT('Ctrl Pts',(-0.121288511086501,0.0113818407630408,
-0.15467863775023));
#49066=CARTESIAN_POINT('Ctrl Pts',(-0.120502055093573,0.0169672735145346,
-0.155012589132842));
#49067=CARTESIAN_POINT('Ctrl Pts',(-0.114947682531521,0.0564145848720949,
-0.157371132285057));
#49068=CARTESIAN_POINT('Ctrl Pts',(-0.0881508852131287,0.0928708592047098,
-0.159729675437271));
#49069=CARTESIAN_POINT('Ctrl Pts',(-0.0521593058589881,0.109945624876804,
-0.162088218589485));
#49070=CARTESIAN_POINT('Ctrl Pts',(-0.0161677265048477,0.127020390548898,
-0.164446761741699));
#49071=CARTESIAN_POINT('Ctrl Pts',(0.0290186348850403,0.124713647560471,
-0.166805304893913));
#49072=CARTESIAN_POINT('Ctrl Pts',(0.0630843229848925,0.104062490133902,
-0.169163848046127));
#49073=CARTESIAN_POINT('Ctrl Pts',(0.0971500110847444,0.0834113327073327,
-0.171522391198341));
#49074=CARTESIAN_POINT('Ctrl Pts',(0.12009502589456,0.0444157608426204,
-0.173880934350555));
#49075=CARTESIAN_POINT('Ctrl Pts',(0.121603457732842,0.00460789670778811,
-0.176239477502769));
#49076=CARTESIAN_POINT('Ctrl Pts',(0.123111889571124,-0.0351999674270442,
-0.178598020654983));
#49077=CARTESIAN_POINT('Ctrl Pts',(0.103183738437872,-0.0758201238319969,
-0.180956563807197));
#49078=CARTESIAN_POINT('Ctrl Pts',(0.0707785543245695,-0.0989900494454684,
-0.183315106959411));
#49079=CARTESIAN_POINT('Ctrl Pts',(0.0383733702112669,-0.12215997505894,
-0.185673650111625));
#49080=CARTESIAN_POINT('Ctrl Pts',(-0.00650884688208582,-0.12787966988093,
-0.188032193263839));
#49081=CARTESIAN_POINT('Ctrl Pts',(-0.0436893826726646,-0.113577601176793,
-0.190390736416053));
#49082=CARTESIAN_POINT('Ctrl Pts',(-0.0808699184632431,-0.0992755324726549,
-0.192749279568267));
#49083=CARTESIAN_POINT('Ctrl Pts',(-0.110348772951047,-0.0649517002423889,
-0.195107822720481));
#49084=CARTESIAN_POINT('Ctrl Pts',(-0.118872470248437,-0.0260378467213308,
-0.197466365872695));
#49085=CARTESIAN_POINT('Ctrl Pts',(-0.120732903289687,-0.0175442768153356,
-0.197981155576799));
#49086=CARTESIAN_POINT('Ctrl Pts',(-0.121595031955655,-0.00883203814462564,
-0.198495945280902));
#49087=CARTESIAN_POINT('Ctrl Pts',(-0.121516972739373,-0.000104509287172358,
-0.199010734985006));
#49088=CARTESIAN_POINT('Ctrl Pts',(-0.121504492117652,-0.000105281444988491,
-0.205489265014994));
#49089=CARTESIAN_POINT('Ctrl Pts',(-0.12158610383313,-0.00925968455859438,
-0.204949438703722));
#49090=CARTESIAN_POINT('Ctrl Pts',(-0.120637079500945,-0.0183973414836741,
-0.20440961239245));
#49091=CARTESIAN_POINT('Ctrl Pts',(-0.118592867240787,-0.0272830434597006,
-0.203869786081178));
#49092=CARTESIAN_POINT('Ctrl Pts',(-0.109661544837283,-0.0661053666969373,
-0.201511242928964));
#49093=CARTESIAN_POINT('Ctrl Pts',(-0.0798243544099606,-0.10011816201817,
-0.19915269977675));
#49094=CARTESIAN_POINT('Ctrl Pts',(-0.0424958770457137,-0.114029527120612,
-0.196794156624536));
#49095=CARTESIAN_POINT('Ctrl Pts',(-0.00516739968146744,-0.127940892223055,
-0.194435613472322));
#49096=CARTESIAN_POINT('Ctrl Pts',(0.0396523646197032,-0.121750827106708,
-0.192077070320108));
#49097=CARTESIAN_POINT('Ctrl Pts',(0.071812779889887,-0.0982423394719399,
-0.189718527167894));
#49098=CARTESIAN_POINT('Ctrl Pts',(0.103973195160071,-0.0747338518371711,
-0.18735998401568));
#49099=CARTESIAN_POINT('Ctrl Pts',(0.123474261399268,-0.0339069416839796,
-0.185001440863466));
#49100=CARTESIAN_POINT('Ctrl Pts',(0.121548442840219,0.00588291285951405,
-0.182642897711252));
#49101=CARTESIAN_POINT('Ctrl Pts',(0.11962262428117,0.0456727674030071,
-0.180284354559038));
#49102=CARTESIAN_POINT('Ctrl Pts',(0.0962699209238745,0.0844255663368025,
-0.177925811406823));
#49103=CARTESIAN_POINT('Ctrl Pts',(0.0619895362165354,0.10471833661211,
-0.175567268254609));
#49104=CARTESIAN_POINT('Ctrl Pts',(0.027709151509196,0.125011106887417,
-0.173208725102395));
#49105=CARTESIAN_POINT('Ctrl Pts',(-0.0174989145481876,0.126843848504235,
-0.170850181950181));
#49106=CARTESIAN_POINT('Ctrl Pts',(-0.0533094483675094,0.109392574391408,
-0.168491638797967));
#49107=CARTESIAN_POINT('Ctrl Pts',(-0.0891199821868312,0.0919413002785813,
-0.166133095645753));
#49108=CARTESIAN_POINT('Ctrl Pts',(-0.115532983768091,0.0552060104361086,
-0.163774552493539));
#49109=CARTESIAN_POINT('Ctrl Pts',(-0.120673362134684,0.015702620529911,
-0.161416009341325));
#49110=CARTESIAN_POINT('Ctrl Pts',(-0.121346633186486,0.0105285872243599,
-0.161107094565881));
#49111=CARTESIAN_POINT('Ctrl Pts',(-0.121654973238394,0.00530706727299804,
-0.160798179790438));
#49112=CARTESIAN_POINT('Ctrl Pts',(-0.12161467894854,8.07629804098239E-5,
-0.160489265014994));
#49113=CARTESIAN_POINT('Origin',(0.,0.,-0.29));
#49114=CARTESIAN_POINT('',(-0.121309037101631,-9.33618319136557E-7,-0.109010734985006));
#49115=CARTESIAN_POINT('',(-0.121309301434334,5.79271293234657E-6,-0.115489265014994));
#49116=CARTESIAN_POINT('',(-0.1215,-1.48794586096403E-17,-0.29));
#49117=CARTESIAN_POINT('Ctrl Pts',(-0.121309046518887,-9.33572278136174E-7,
-0.109010734985006));
#49118=CARTESIAN_POINT('Ctrl Pts',(-0.121307664074448,0.0201371841581811,
-0.110193427454334));
#49119=CARTESIAN_POINT('Ctrl Pts',(-0.116556959955105,0.0402759190252943,
-0.111376119923662));
#49120=CARTESIAN_POINT('Ctrl Pts',(-0.107060609773819,0.0578503306347235,
-0.11255881239299));
#49121=CARTESIAN_POINT('Ctrl Pts',(-0.0881228450784662,0.0928974872122608,
-0.114917355545204));
#49122=CARTESIAN_POINT('Ctrl Pts',(-0.0503121501341162,0.11774660260711,
-0.117275898697418));
#49123=CARTESIAN_POINT('Ctrl Pts',(-0.0106279342068158,0.121225736562482,
-0.119634441849632));
#49124=CARTESIAN_POINT('Ctrl Pts',(0.0290562817204846,0.124704870517854,
-0.121992985001846));
#49125=CARTESIAN_POINT('Ctrl Pts',(0.0706140186307353,0.106814023033748,
-0.12435152815406));
#49126=CARTESIAN_POINT('Ctrl Pts',(0.0953612236640026,0.0755967668366386,
-0.126710071306274));
#49127=CARTESIAN_POINT('Ctrl Pts',(0.12010842869727,0.0443795106395292,
-0.129068614458488));
#49128=CARTESIAN_POINT('Ctrl Pts',(0.128045101853553,-0.000164154270584499,
-0.131427157610702));
#49129=CARTESIAN_POINT('Ctrl Pts',(0.115602973532799,-0.0380077133606588,
-0.133785700762916));
#49130=CARTESIAN_POINT('Ctrl Pts',(0.103160845212044,-0.0758512724507334,
-0.13614424391513));
#49131=CARTESIAN_POINT('Ctrl Pts',(0.0703399154142509,-0.106994725720769,
-0.138502787067344));
#49132=CARTESIAN_POINT('Ctrl Pts',(0.0318962323681036,-0.117436211625325,
-0.140861330219558));
#49133=CARTESIAN_POINT('Ctrl Pts',(-0.00654745067804376,-0.127877697529882,
-0.143219873371772));
#49134=CARTESIAN_POINT('Ctrl Pts',(-0.0506138869725449,-0.117617216068959,
-0.145578416523986));
#49135=CARTESIAN_POINT('Ctrl Pts',(-0.08049113121694,-0.0912678011472448,
-0.1479369596762));
#49136=CARTESIAN_POINT('Ctrl Pts',(-0.106137989846092,-0.0686492586226994,
-0.149961551445802));
#49137=CARTESIAN_POINT('Ctrl Pts',(-0.121329345069859,-0.0341753618260928,
-0.151986143215404));
#49138=CARTESIAN_POINT('Ctrl Pts',(-0.121603817730479,8.52412621186009E-5,
-0.154010734985006));
#49139=CARTESIAN_POINT('Ctrl Pts',(-0.12161467894854,8.07629804098239E-5,
-0.160489265014994));
#49140=CARTESIAN_POINT('Ctrl Pts',(-0.121347329095214,-0.0345954080390664,
-0.158439636638224));
#49141=CARTESIAN_POINT('Ctrl Pts',(-0.105732288041653,-0.0694821968403921,
-0.156390008261453));
#49142=CARTESIAN_POINT('Ctrl Pts',(-0.0795295660295233,-0.0921068985596655,
-0.154340379884683));
#49143=CARTESIAN_POINT('Ctrl Pts',(-0.0493776364058448,-0.11814153777312,
-0.151981836732469));
#49144=CARTESIAN_POINT('Ctrl Pts',(-0.00520602200656287,-0.127939326230107,
-0.149623293580255));
#49145=CARTESIAN_POINT('Ctrl Pts',(0.0331260445435072,-0.117095250825184,
-0.147264750428041));
#49146=CARTESIAN_POINT('Ctrl Pts',(0.0714581110935774,-0.106251175420261,
-0.144906207275827));
#49147=CARTESIAN_POINT('Ctrl Pts',(0.103950629794436,-0.0747652361534276,
-0.142547664123613));
#49148=CARTESIAN_POINT('Ctrl Pts',(0.115995203675548,-0.0367932786294693,
-0.140189120971399));
#49149=CARTESIAN_POINT('Ctrl Pts',(0.12803977755666,0.00117867889448893,
-0.137830577819185));
#49150=CARTESIAN_POINT('Ctrl Pts',(0.119636406618026,0.0456366546755723,
-0.135472034666971));
#49151=CARTESIAN_POINT('Ctrl Pts',(0.0945631842556541,0.0765926686457221,
-0.133113491514757));
#49152=CARTESIAN_POINT('Ctrl Pts',(0.0694899618932821,0.107548682615872,
-0.130754948362543));
#49153=CARTESIAN_POINT('Ctrl Pts',(0.0277468881071721,0.125002734775089,
-0.128396405210329));
#49154=CARTESIAN_POINT('Ctrl Pts',(-0.0118986579771398,0.121107614763766,
-0.126037862058114));
#49155=CARTESIAN_POINT('Ctrl Pts',(-0.0515442040614505,0.117212494752444,
-0.1236793189059));
#49156=CARTESIAN_POINT('Ctrl Pts',(-0.0890922224439633,0.091968202570584,
-0.121320775753686));
#49157=CARTESIAN_POINT('Ctrl Pts',(-0.107661401631213,0.056724380465849,
-0.118962232601472));
#49158=CARTESIAN_POINT('Ctrl Pts',(-0.116775807327555,0.03942547405146,
-0.117804576739313));
#49159=CARTESIAN_POINT('Ctrl Pts',(-0.121317847477761,0.0197174895250484,
-0.116646920877154));
#49160=CARTESIAN_POINT('Ctrl Pts',(-0.121309301434334,5.79271293234657E-6,
-0.115489265014994));
#49161=CARTESIAN_POINT('Origin',(0.,0.,-0.29));
#49162=CARTESIAN_POINT('',(-0.121606852599128,-8.52915087747597E-5,-0.0640107349850058));
#49163=CARTESIAN_POINT('',(-0.121595695105322,-8.84116883933851E-5,-0.0704892650149944));
#49164=CARTESIAN_POINT('',(-0.1215,-1.48794586096403E-17,-0.29));
#49165=CARTESIAN_POINT('Ctrl Pts',(-0.121606852599128,-8.52915087747597E-5,
-0.0640107349850058));
#49166=CARTESIAN_POINT('Ctrl Pts',(-0.121334152356696,0.0342887112479717,
-0.0660421685410495));
#49167=CARTESIAN_POINT('Ctrl Pts',(-0.106027699321683,0.0688771005653459,
-0.0680736020970932));
#49168=CARTESIAN_POINT('Ctrl Pts',(-0.0802292283098266,0.0914986392585654,
-0.0701050356531369));
#49169=CARTESIAN_POINT('Ctrl Pts',(-0.0502765838033985,0.11776278903531,
-0.072463578805351));
#49170=CARTESIAN_POINT('Ctrl Pts',(-0.00618094275775686,0.127895902119566,
-0.074822121957565));
#49171=CARTESIAN_POINT('Ctrl Pts',(0.0322326537889043,0.117344037501139,
-0.077180665109779));
#49172=CARTESIAN_POINT('Ctrl Pts',(0.0706462503355655,0.106792172882712,
-0.079539208261993));
#49173=CARTESIAN_POINT('Ctrl Pts',(0.103377802383246,0.0755553305616026,
-0.081897751414207));
#49174=CARTESIAN_POINT('Ctrl Pts',(0.115711427039349,0.0376764002307086,
-0.0842562945664211));
#49175=CARTESIAN_POINT('Ctrl Pts',(0.128045051695452,-0.000202530100185408,
-0.0866148377186352));
#49176=CARTESIAN_POINT('Ctrl Pts',(0.119980748959977,-0.0447235484408638,
-0.0889733808708493));
#49177=CARTESIAN_POINT('Ctrl Pts',(0.0951441795036263,-0.0758698249428511,
-0.0913319240230634));
#49178=CARTESIAN_POINT('Ctrl Pts',(0.0703076100472756,-0.107016101444838,
-0.0936904671752774));
#49179=CARTESIAN_POINT('Ctrl Pts',(0.028698773870049,-0.124787636108134,
-0.0960490103274914));
#49180=CARTESIAN_POINT('Ctrl Pts',(-0.0109753077276821,-0.121194745221755,
-0.0984075534797054));
#49181=CARTESIAN_POINT('Ctrl Pts',(-0.050649389325413,-0.117601854335375,
-0.100766096631919));
#49182=CARTESIAN_POINT('Ctrl Pts',(-0.0883887163436492,-0.0926445378993189,
-0.103124639784134));
#49183=CARTESIAN_POINT('Ctrl Pts',(-0.107225962629589,-0.0575432808011788,
-0.105483182936348));
#49184=CARTESIAN_POINT('Ctrl Pts',(-0.116617263733503,-0.0400435640415918,
-0.106659033619234));
#49185=CARTESIAN_POINT('Ctrl Pts',(-0.121310420965989,-0.0200225538154995,
-0.10783488430212));
#49186=CARTESIAN_POINT('Ctrl Pts',(-0.121309046518887,-9.33572278136174E-7,
-0.109010734985006));
#49187=CARTESIAN_POINT('Ctrl Pts',(-0.121309301434334,5.79271293234657E-6,
-0.115489265014994));
#49188=CARTESIAN_POINT('Ctrl Pts',(-0.121300436247998,-0.0204420164683971,
-0.11428837772494));
#49189=CARTESIAN_POINT('Ctrl Pts',(-0.116394765147926,-0.0408938203752012,
-0.113087490434885));
#49190=CARTESIAN_POINT('Ctrl Pts',(-0.106616599719654,-0.0586645870706639,
-0.11188660314483));
#49191=CARTESIAN_POINT('Ctrl Pts',(-0.087412278628859,-0.0935663804748282,
-0.109528059992616));
#49192=CARTESIAN_POINT('Ctrl Pts',(-0.0494132964552827,-0.118126615255547,
-0.107169516840402));
#49193=CARTESIAN_POINT('Ctrl Pts',(-0.00970371956802299,-0.121303210962312,
-0.104810973688188));
#49194=CARTESIAN_POINT('Ctrl Pts',(0.0300058573192376,-0.124479806669077,
-0.102452430535974));
#49195=CARTESIAN_POINT('Ctrl Pts',(0.0714260289201816,-0.106272763301887,
-0.10009388738376));
#49196=CARTESIAN_POINT('Ctrl Pts',(0.0959345983609506,-0.0748677950423748,
-0.097735344231546));
#49197=CARTESIAN_POINT('Ctrl Pts',(0.120443167801719,-0.0434628267828625,
-0.095376801079332));
#49198=CARTESIAN_POINT('Ctrl Pts',(0.128040135082313,0.00114006636897254,
-0.0930182579271179));
#49199=CARTESIAN_POINT('Ctrl Pts',(0.11530994589185,0.0388876791290693,
-0.0906597147749039));
#49200=CARTESIAN_POINT('Ctrl Pts',(0.102579756701387,0.0766352918891664,
-0.0883011716226898));
#49201=CARTESIAN_POINT('Ctrl Pts',(0.0695224110398688,0.107527624257525,
-0.0859426284704758));
#49202=CARTESIAN_POINT('Ctrl Pts',(0.0310002742191683,0.117675849709285,
-0.0835840853182618));
#49203=CARTESIAN_POINT('Ctrl Pts',(-0.00752186260153201,0.127824075161045,
-0.0812255421660478));
#49204=CARTESIAN_POINT('Ctrl Pts',(-0.0515087905814142,0.117228193696207,
-0.0788669990138337));
#49205=CARTESIAN_POINT('Ctrl Pts',(-0.0811843604808662,0.0906517723674608,
-0.0765084558616196));
#49206=CARTESIAN_POINT('Ctrl Pts',(-0.106429170119603,0.0680433877737934,
-0.0745020589127445));
#49207=CARTESIAN_POINT('Ctrl Pts',(-0.121317148211621,0.033870219567978,
-0.0724956619638695));
#49208=CARTESIAN_POINT('Ctrl Pts',(-0.121595695105322,-8.84116883933851E-5,
-0.0704892650149944));
#49209=CARTESIAN_POINT('Origin',(0.,0.,-0.29));
#49210=CARTESIAN_POINT('',(-0.121508540285962,0.000130861710946541,-0.0190107349850059));
#49211=CARTESIAN_POINT('',(-0.121526217441981,0.000102663445846418,-0.0254892650149941));
#49212=CARTESIAN_POINT('',(-0.1215,-1.48794586096403E-17,-0.29));
#49213=CARTESIAN_POINT('Ctrl Pts',(-0.121508540285962,0.000130861710946541,
-0.0190107349850059));
#49214=CARTESIAN_POINT('Ctrl Pts',(-0.121590276950577,0.0089502089992317,
-0.0195323664755513));
#49215=CARTESIAN_POINT('Ctrl Pts',(-0.120706038295682,0.0177562809340787,
-0.0200539979660966));
#49216=CARTESIAN_POINT('Ctrl Pts',(-0.118797094411048,0.0263429264125233,
-0.020575629456642));
#49217=CARTESIAN_POINT('Ctrl Pts',(-0.110165854524904,0.0651672195404196,
-0.0229341726088561));
#49218=CARTESIAN_POINT('Ctrl Pts',(-0.080585821771702,0.0995056183337115,
-0.0252927157610701));
#49219=CARTESIAN_POINT('Ctrl Pts',(-0.0433635147056392,0.113725897500623,
-0.0276512589132841));
#49220=CARTESIAN_POINT('Ctrl Pts',(-0.00614120763957639,0.127946176667534,
-0.0300098020654982));
#49221=CARTESIAN_POINT('Ctrl Pts',(0.0387233737393477,0.122048336208064,
-0.0323683452177122));
#49222=CARTESIAN_POINT('Ctrl Pts',(0.0710617426615871,0.0987737492725815,
-0.0347268883699262));
#49223=CARTESIAN_POINT('Ctrl Pts',(0.103400111583827,0.0754991623370986,
-0.0370854315221403));
#49224=CARTESIAN_POINT('Ctrl Pts',(0.123212268049381,0.0348478289256035,
-0.0394439746743542));
#49225=CARTESIAN_POINT('Ctrl Pts',(0.121589879662122,-0.00494942974450984,
-0.0418025178265683));
#49226=CARTESIAN_POINT('Ctrl Pts',(0.119967491274862,-0.0447466884146232,
-0.0441610609787823));
#49227=CARTESIAN_POINT('Ctrl Pts',(0.0969105580347855,-0.0836898723433555,
-0.0465196041309965));
#49228=CARTESIAN_POINT('Ctrl Pts',(0.0627857651119705,-0.104246522245439,
-0.0488781472832105));
#49229=CARTESIAN_POINT('Ctrl Pts',(0.0286609721891549,-0.124803172147523,
-0.0512366904354246));
#49230=CARTESIAN_POINT('Ctrl Pts',(-0.0165316804163984,-0.126973288022959,
-0.0535952335876386));
#49231=CARTESIAN_POINT('Ctrl Pts',(-0.0524741460072976,-0.109793759220386,
-0.0559537767398526));
#49232=CARTESIAN_POINT('Ctrl Pts',(-0.0884166115981963,-0.0926142304178135,
-0.0583123198920666));
#49233=CARTESIAN_POINT('Ctrl Pts',(-0.11510889017444,-0.0560850569372318,
-0.0606708630442807));
#49234=CARTESIAN_POINT('Ctrl Pts',(-0.120550205478954,-0.0166228769623238,
-0.0630294061964947));
#49235=CARTESIAN_POINT('Ctrl Pts',(-0.121304868988174,-0.0111498129043366,
-0.0633565157926651));
#49236=CARTESIAN_POINT('Ctrl Pts',(-0.121650763888233,-0.00562033159269298,
-0.0636836253888354));
#49237=CARTESIAN_POINT('Ctrl Pts',(-0.121606852599128,-8.52915087747597E-5,
-0.0640107349850058));
#49238=CARTESIAN_POINT('Ctrl Pts',(-0.121595695105322,-8.84116883933851E-5,
-0.0704892650149944));
#49239=CARTESIAN_POINT('Ctrl Pts',(-0.121644583353046,-0.00604854987252561,
-0.0701371188116555));
#49240=CARTESIAN_POINT('Ctrl Pts',(-0.121243437305456,-0.0120020793815115,
-0.0697849726083166));
#49241=CARTESIAN_POINT('Ctrl Pts',(-0.12036926516354,-0.0178853149891245,
-0.0694328264049777));
#49242=CARTESIAN_POINT('Ctrl Pts',(-0.11451438812774,-0.0572890198243118,
-0.0670742832527636));
#49243=CARTESIAN_POINT('Ctrl Pts',(-0.087440422237116,-0.0935394683020307,
-0.0647157401005495));
#49244=CARTESIAN_POINT('Ctrl Pts',(-0.0513198022297531,-0.110339675010818,
-0.0623571969483354));
#49245=CARTESIAN_POINT('Ctrl Pts',(-0.0151991822223908,-0.127139881719604,
-0.0599986537961213));
#49246=CARTESIAN_POINT('Ctrl Pts',(0.0299680919017115,-0.124489846659459,
-0.0576401106439072));
#49247=CARTESIAN_POINT('Ctrl Pts',(0.0638754863487052,-0.103579203383963,
-0.0552815674916932));
#49248=CARTESIAN_POINT('Ctrl Pts',(0.0977828807956984,-0.0826685601084671,
-0.0529230243394792));
#49249=CARTESIAN_POINT('Ctrl Pts',(0.120430395565585,-0.0434973086176221,
-0.0505644811872652));
#49250=CARTESIAN_POINT('Ctrl Pts',(0.121635229050253,-0.00367997854823185,
-0.0482059380350512));
#49251=CARTESIAN_POINT('Ctrl Pts',(0.122840062534921,0.0361373515211595,
-0.0458473948828371));
#49252=CARTESIAN_POINT('Ctrl Pts',(0.10260221473437,0.0766007601690952,
-0.043488851730623));
#49253=CARTESIAN_POINT('Ctrl Pts',(0.0700216994762484,0.0995246985894165,
-0.041130308578409));
#49254=CARTESIAN_POINT('Ctrl Pts',(0.0374411842181272,0.122448637009737,
-0.0387717654261949));
#49255=CARTESIAN_POINT('Ctrl Pts',(-0.00748199849756367,0.127833105202444,
-0.0364132222739809));
#49256=CARTESIAN_POINT('Ctrl Pts',(-0.0445530473550404,0.11324493435664,
-0.0340546791217669));
#49257=CARTESIAN_POINT('Ctrl Pts',(-0.0816240962125166,0.098656763510837,
-0.0316961359695529));
#49258=CARTESIAN_POINT('Ctrl Pts',(-0.110843011211779,0.0640959536265228,
-0.0293375928173388));
#49259=CARTESIAN_POINT('Ctrl Pts',(-0.119068742960021,0.0251242850883948,
-0.0269790496651247));
#49260=CARTESIAN_POINT('Ctrl Pts',(-0.120800683414184,0.0169187404179371,
-0.0264824547817479));
#49261=CARTESIAN_POINT('Ctrl Pts',(-0.121601955132731,0.00851765378525109,
-0.025985859898371));
#49262=CARTESIAN_POINT('Ctrl Pts',(-0.121526217441981,0.000102663445846418,
-0.0254892650149941));
#49263=CARTESIAN_POINT('Origin',(0.,0.,-0.656687266823562));
#49264=CARTESIAN_POINT('',(-0.0959092728420695,-6.72679739015819E-5,-0.0491872668235618));
#49265=CARTESIAN_POINT('',(-0.0958456772541386,8.09689275490001E-5,-0.0403127331764372));
#49266=CARTESIAN_POINT('',(-0.095825,-8.02710626669594E-15,-0.656687266823562));
#49267=CARTESIAN_POINT('',(-0.0256835729485001,0.0924624001170202,-0.0134999999999999));
#49268=CARTESIAN_POINT('Ctrl Pts',(-0.0959092728420695,-6.72679739015716E-5,
-0.0491872668235618));
#49269=CARTESIAN_POINT('Ctrl Pts',(-0.0959439049348964,-0.00443266069852132,
-0.0488601572273916));
#49270=CARTESIAN_POINT('Ctrl Pts',(-0.0937041356633229,-0.0402376474948893,
-0.0461745044790073));
#49271=CARTESIAN_POINT('Ctrl Pts',(-0.0486809400150489,-0.101853223691883,
-0.041130308578409));
#49272=CARTESIAN_POINT('Ctrl Pts',(0.0582471077856237,-0.0967186223643828,
-0.0340546791217668));
#49273=CARTESIAN_POINT('Ctrl Pts',(0.112800950445628,-0.0045771260688116,
-0.0269790496651248));
#49274=CARTESIAN_POINT('Ctrl Pts',(0.0674088876487516,0.0885600284958335,
-0.0201274899578691));
#49275=CARTESIAN_POINT('Ctrl Pts',(0.00179055959947813,0.0999014741116878,
-0.0156344734028275));
#49276=CARTESIAN_POINT('Ctrl Pts',(-0.0256835729485001,0.0924624001170201,
-0.0134999999999999));
#49277=CARTESIAN_POINT('',(0.0789701248920219,0.054278448757665,-0.0135));
#49278=CARTESIAN_POINT('Origin',(0.,0.,-0.0135));
#49279=CARTESIAN_POINT('Ctrl Pts',(-0.0958456772541386,8.09689275489984E-5,
-0.0403127331764372));
#49280=CARTESIAN_POINT('Ctrl Pts',(-0.0956217123444332,-0.0248031083775501,
-0.0384507849076002));
#49281=CARTESIAN_POINT('Ctrl Pts',(-0.073072965252975,-0.0815574531722432,
-0.0342302934865492));
#49282=CARTESIAN_POINT('Ctrl Pts',(0.022090743255976,-0.110784791206306,
-0.0276512589132841));
#49283=CARTESIAN_POINT('Ctrl Pts',(0.104628794236781,-0.0423248975405764,
-0.0205756294566421));
#49284=CARTESIAN_POINT('Ctrl Pts',(0.0968448185910171,0.0282724219436266,
-0.0158585431522139));
#49285=CARTESIAN_POINT('Ctrl Pts',(0.0789701248920212,0.0542784487576661,
-0.0134999999999998));
#49286=CARTESIAN_POINT('Origin',(0.,0.,-0.656687266823562));
#49287=CARTESIAN_POINT('',(-0.095674398211295,-7.36292708573769E-7,-0.094187266823562));
#49288=CARTESIAN_POINT('',(-0.0959004731149589,-6.97288069272384E-5,-0.0853127331764372));
#49289=CARTESIAN_POINT('',(-0.095825,-8.02710626669594E-15,-0.656687266823562));
#49290=CARTESIAN_POINT('Ctrl Pts',(-0.095674398211295,-7.36292708577307E-7,
-0.094187266823562));
#49291=CARTESIAN_POINT('Ctrl Pts',(-0.0956754822145337,-0.0157914503651906,
-0.093011416140676));
#49292=CARTESIAN_POINT('Ctrl Pts',(-0.0845497034522949,-0.0632540260551953,
-0.0894770223055759));
#49293=CARTESIAN_POINT('Ctrl Pts',(-0.0101819483175724,-0.112434012668085,
-0.0835840853182618));
#49294=CARTESIAN_POINT('Ctrl Pts',(0.0882666128350871,-0.0703856840480749,
-0.0765084558616196));
#49295=CARTESIAN_POINT('Ctrl Pts',(0.107347151344391,0.0349532439147777,
-0.0694328264049776));
#49296=CARTESIAN_POINT('Ctrl Pts',(0.0299026828266366,0.108861155406636,
-0.0623571969483354));
#49297=CARTESIAN_POINT('Ctrl Pts',(-0.0696064437572946,0.08599410531552,
-0.0556086770878635));
#49298=CARTESIAN_POINT('Ctrl Pts',(-0.0956941987619804,0.0270429280274596,
-0.0512187003796056));
#49299=CARTESIAN_POINT('Ctrl Pts',(-0.0959092728420695,-6.72679739015716E-5,
-0.0491872668235618));
#49300=CARTESIAN_POINT('Ctrl Pts',(-0.0959004731149589,-6.97288069272505E-5,
-0.0853127331764372));
#49301=CARTESIAN_POINT('Ctrl Pts',(-0.0959390304510746,-0.00477038923074731,
-0.0849605869730985));
#49302=CARTESIAN_POINT('Ctrl Pts',(-0.0935036780836808,-0.0409141884060264,
-0.0822498976175458));
#49303=CARTESIAN_POINT('Ctrl Pts',(-0.0476100055917889,-0.102363117493165,
-0.0771806651097791));
#49304=CARTESIAN_POINT('Ctrl Pts',(0.0592579954685063,-0.0960930036749314,
-0.0701050356531369));
#49305=CARTESIAN_POINT('Ctrl Pts',(0.112843133809849,-0.00341188826479888,
-0.0630294061964947));
#49306=CARTESIAN_POINT('Ctrl Pts',(0.064959386513852,0.0923265347892355,
-0.0559537767398527));
#49307=CARTESIAN_POINT('Ctrl Pts',(-0.04133108222025,0.105066452432841,
-0.0488781472832105));
#49308=CARTESIAN_POINT('Ctrl Pts',(-0.0922720603096074,0.0448122828611172,
-0.0436644660954054));
#49309=CARTESIAN_POINT('Ctrl Pts',(-0.0959054102929546,0.00671772982692123,
-0.0408093280598143));
#49310=CARTESIAN_POINT('Ctrl Pts',(-0.0958456772541386,8.09689275489984E-5,
-0.0403127331764372));
#49311=CARTESIAN_POINT('Origin',(0.,0.,-0.656687266823562));
#49312=CARTESIAN_POINT('',(-0.0959068792923712,6.72283452001022E-5,-0.139187266823562));
#49313=CARTESIAN_POINT('',(-0.0956745992588073,4.56861494406435E-6,-0.130312733176437));
#49314=CARTESIAN_POINT('',(-0.095825,-8.02710626669594E-15,-0.656687266823562));
#49315=CARTESIAN_POINT('Ctrl Pts',(-0.0959068792923711,6.7228345200105E-5,
-0.139187266823562));
#49316=CARTESIAN_POINT('Ctrl Pts',(-0.0956904073359593,-0.0269535312509126,
-0.13716267505396));
#49317=CARTESIAN_POINT('Ctrl Pts',(-0.0697518127439643,-0.0858162475683075,
-0.132779540132144));
#49318=CARTESIAN_POINT('Ctrl Pts',(0.0295905909193192,-0.108947251043571,
-0.126037862058114));
#49319=CARTESIAN_POINT('Ctrl Pts',(0.107246531607553,-0.0352603026583548,
-0.118962232601472));
#49320=CARTESIAN_POINT('Ctrl Pts',(0.0884679709853073,0.0701322082061288,
-0.11188660314483));
#49321=CARTESIAN_POINT('Ctrl Pts',(-0.00985968677826821,0.112462836852163,
-0.104810973688188));
#49322=CARTESIAN_POINT('Ctrl Pts',(-0.084454582307197,0.0634392161651233,
-0.0989111949144321));
#49323=CARTESIAN_POINT('Ctrl Pts',(-0.0956733079006921,0.0158818573823644,
-0.09536995929289));
#49324=CARTESIAN_POINT('Ctrl Pts',(-0.095674398211295,-7.36292708577307E-7,
-0.094187266823562));
#49325=CARTESIAN_POINT('Ctrl Pts',(-0.0956745992588073,4.56861494405394E-6,
-0.130312733176437));
#49326=CARTESIAN_POINT('Ctrl Pts',(-0.0956676074359193,-0.01612227348218,
-0.129111845886383));
#49327=CARTESIAN_POINT('Ctrl Pts',(-0.0841998304209556,-0.0639315786664402,
-0.125552415444114));
#49328=CARTESIAN_POINT('Ctrl Pts',(-0.00900227708678451,-0.112534711150002,
-0.119634441849632));
#49329=CARTESIAN_POINT('Ctrl Pts',(0.0889998943616218,-0.0694559474299769,
-0.11255881239299));
#49330=CARTESIAN_POINT('Ctrl Pts',(0.106974694106382,0.0360767003792724,
-0.105483182936348));
#49331=CARTESIAN_POINT('Ctrl Pts',(0.0287593818097131,0.109169484310085,
-0.0984075534797054));
#49332=CARTESIAN_POINT('Ctrl Pts',(-0.0701361529300369,0.0853468303619958,
-0.0916840702264021));
#49333=CARTESIAN_POINT('Ctrl Pts',(-0.0956807878796623,0.0267128707004158,
-0.0873191301253126));
#49334=CARTESIAN_POINT('Ctrl Pts',(-0.0959004731149589,-6.97288069272505E-5,
-0.0853127331764372));
#49335=CARTESIAN_POINT('Origin',(0.,0.,-0.656687266823562));
#49336=CARTESIAN_POINT('',(-0.0958383861131722,-8.24247114732218E-5,-0.184187266823562));
#49337=CARTESIAN_POINT('',(-0.0959154453518014,6.36963999718059E-5,-0.175312733176437));
#49338=CARTESIAN_POINT('',(-0.095825,-8.02710626669594E-15,-0.656687266823562));
#49339=CARTESIAN_POINT('Ctrl Pts',(-0.0958383861131722,-8.24247114732208E-5,
-0.184187266823562));
#49340=CARTESIAN_POINT('Ctrl Pts',(-0.0958999501000052,-0.00696567946674315,
-0.183672477119459));
#49341=CARTESIAN_POINT('Ctrl Pts',(-0.0921047845740635,-0.0453177134055506,
-0.180799144263141));
#49342=CARTESIAN_POINT('Ctrl Pts',(-0.040531265065401,-0.105367564795535,
-0.17556726825461));
#49343=CARTESIAN_POINT('Ctrl Pts',(0.0656622769832545,-0.0918344843926382,
-0.168491638797967));
#49344=CARTESIAN_POINT('Ctrl Pts',(0.112813266670755,0.00427481159513008,
-0.161416009341325));
#49345=CARTESIAN_POINT('Ctrl Pts',(0.0585242285435791,0.0965402603342907,
-0.154340379884683));
#49346=CARTESIAN_POINT('Ctrl Pts',(-0.0483889339301513,0.10199812815814,
-0.147264750428041));
#49347=CARTESIAN_POINT('Ctrl Pts',(-0.0936497336964331,0.0404221079648366,
-0.142213712741001));
#49348=CARTESIAN_POINT('Ctrl Pts',(-0.0959425858037904,0.00452423551170105,
-0.139521218206174));
#49349=CARTESIAN_POINT('Ctrl Pts',(-0.0959068792923711,6.7228345200105E-5,
-0.139187266823562));
#49350=CARTESIAN_POINT('Ctrl Pts',(-0.0959154453518014,6.36963999718103E-5,
-0.175312733176437));
#49351=CARTESIAN_POINT('Ctrl Pts',(-0.0957045910333214,-0.0272848146118881,
-0.173263104799667));
#49352=CARTESIAN_POINT('Ctrl Pts',(-0.0692178185861295,-0.0864609918133612,
-0.168854933270683));
#49353=CARTESIAN_POINT('Ctrl Pts',(0.0307315052759879,-0.108630938394162,
-0.162088218589485));
#49354=CARTESIAN_POINT('Ctrl Pts',(0.107610409091042,-0.0341336512276352,
-0.155012589132842));
#49355=CARTESIAN_POINT('Ctrl Pts',(0.087727618468951,0.0710561149260017,
-0.147936959676201));
#49356=CARTESIAN_POINT('Ctrl Pts',(-0.0110385554953438,0.112353264263208,
-0.140861330219558));
#49357=CARTESIAN_POINT('Ctrl Pts',(-0.0848008734968956,0.0627613659991513,
-0.134986588052971));
#49358=CARTESIAN_POINT('Ctrl Pts',(-0.0956813393790671,0.0155508513064774,
-0.131470389038597));
#49359=CARTESIAN_POINT('Ctrl Pts',(-0.0956745992588073,4.56861494405394E-6,
-0.130312733176437));
#49360=CARTESIAN_POINT('Origin',(0.,0.,-0.656687266823562));
#49361=CARTESIAN_POINT('',(-0.0956894144726637,3.76115011439749E-5,-0.229187266823562));
#49362=CARTESIAN_POINT('',(-0.0958285428573996,-8.30336993179887E-5,-0.220312733176437));
#49363=CARTESIAN_POINT('',(-0.095825,-8.02710626669594E-15,-0.656687266823562));
#49364=CARTESIAN_POINT('Ctrl Pts',(-0.0956894144726637,3.76115011439743E-5,
-0.229187266823562));
#49365=CARTESIAN_POINT('Ctrl Pts',(-0.0956234773178782,-0.0182662859553927,
-0.227823736032743));
#49366=CARTESIAN_POINT('Ctrl Pts',(-0.0818051360670546,-0.0683232197199062,
-0.22410166208971));
#49367=CARTESIAN_POINT('Ctrl Pts',(-0.00132056587373289,-0.112886506095197,
-0.218021044994462));
#49368=CARTESIAN_POINT('Ctrl Pts',(0.0935216704263627,-0.0632360997609839,
-0.21094541553782));
#49369=CARTESIAN_POINT('Ctrl Pts',(0.104270598111585,0.04327527610209,-0.203869786081178));
#49370=CARTESIAN_POINT('Ctrl Pts',(0.0212609397230408,0.110874161081468,
-0.196794156624536));
#49371=CARTESIAN_POINT('Ctrl Pts',(-0.0734359464271463,0.0811118993918514,
-0.190233316871997));
#49372=CARTESIAN_POINT('Ctrl Pts',(-0.0956178906135575,0.0245704084514466,
-0.186031020271673));
#49373=CARTESIAN_POINT('Ctrl Pts',(-0.0958383861131722,-8.24247114732208E-5,
-0.184187266823562));
#49374=CARTESIAN_POINT('Ctrl Pts',(-0.0958285428573997,-8.30336993179982E-5,
-0.220312733176437));
#49375=CARTESIAN_POINT('Ctrl Pts',(-0.0958929086404081,-0.00730295697800942,
-0.219772906865166));
#49376=CARTESIAN_POINT('Ctrl Pts',(-0.0918742640892126,-0.045996375015137,
-0.21687453740168));
#49377=CARTESIAN_POINT('Ctrl Pts',(-0.0394240328282805,-0.105786822938669,
-0.211617624785979));
#49378=CARTESIAN_POINT('Ctrl Pts',(0.0666217428299838,-0.0911408231911627,
-0.204541995329337));
#49379=CARTESIAN_POINT('Ctrl Pts',(0.112762228567538,0.00545766237499973,
-0.197466365872695));
#49380=CARTESIAN_POINT('Ctrl Pts',(0.0575085792042569,0.0971486983708248,
-0.190390736416053));
#49381=CARTESIAN_POINT('Ctrl Pts',(-0.0494559375846015,0.101485055541974,
-0.183315106959411));
#49382=CARTESIAN_POINT('Ctrl Pts',(-0.0938473597137678,0.0397453190179913,
-0.178289105879539));
#49383=CARTESIAN_POINT('Ctrl Pts',(-0.0959472247783466,0.00418559441509606,
-0.175621647951881));
#49384=CARTESIAN_POINT('Ctrl Pts',(-0.0959154453518014,6.36963999718103E-5,
-0.175312733176437));
#49385=CARTESIAN_POINT('Origin',(0.,0.,-0.656687266823562));
#49386=CARTESIAN_POINT('',(-0.0959600152474598,3.37514099930798E-5,-0.274187266823562));
#49387=CARTESIAN_POINT('',(-0.0956936940907658,4.2276044067896E-5,-0.265312733176437));
#49388=CARTESIAN_POINT('',(-0.095825,-8.02710626669594E-15,-0.656687266823562));
#49389=CARTESIAN_POINT('Ctrl Pts',(-0.0959600152474598,3.3751409993089E-5,
-0.274187266823562));
#49390=CARTESIAN_POINT('Ctrl Pts',(-0.0958240821787534,-0.0294487663342971,
-0.271974994946027));
#49391=CARTESIAN_POINT('Ctrl Pts',(-0.0656044598416009,-0.0906043475731541,
-0.267404179916278));
#49392=CARTESIAN_POINT('Ctrl Pts',(0.038055294715108,-0.106286883935013,
-0.260474821734315));
#49393=CARTESIAN_POINT('Ctrl Pts',(0.10968443433419,-0.0267288611289883,
-0.253399192277673));
#49394=CARTESIAN_POINT('Ctrl Pts',(0.0826869460855996,0.0768633599284799,
-0.246323562821031));
#49395=CARTESIAN_POINT('Ctrl Pts',(-0.0186614262296518,0.111341179819334,
-0.239247933364389));
#49396=CARTESIAN_POINT('Ctrl Pts',(-0.0869327277281451,0.0583517239853639,
-0.233535834698566));
#49397=CARTESIAN_POINT('Ctrl Pts',(-0.0957375309395074,0.0133945553659869,
-0.230182279184957));
#49398=CARTESIAN_POINT('Ctrl Pts',(-0.0956894144726637,3.76115011439743E-5,
-0.229187266823562));
#49399=CARTESIAN_POINT('Ctrl Pts',(-0.0956936940907658,4.22760440678986E-5,
-0.265312733176437));
#49400=CARTESIAN_POINT('Ctrl Pts',(-0.0956180125879371,-0.0185956166067511,
-0.26392416577845));
#49401=CARTESIAN_POINT('Ctrl Pts',(-0.0814174178878608,-0.0689973587414746,
-0.260177055228248));
#49402=CARTESIAN_POINT('Ctrl Pts',(-0.000136639224089264,-0.112894143340924,
-0.254071401525832));
#49403=CARTESIAN_POINT('Ctrl Pts',(0.0941796886812631,-0.0622518474490773,
-0.24699577206919));
#49404=CARTESIAN_POINT('Ctrl Pts',(0.103811027648513,0.0443663927929224,
-0.239920142612548));
#49405=CARTESIAN_POINT('Ctrl Pts',(0.0200970195336817,0.111091026086466,
-0.232844513155906));
#49406=CARTESIAN_POINT('Ctrl Pts',(-0.0739223767674631,0.0804546630638847,
-0.226308710010535));
#49407=CARTESIAN_POINT('Ctrl Pts',(-0.0956116895268125,0.0242414495336793,
-0.22213145001738));
#49408=CARTESIAN_POINT('Ctrl Pts',(-0.0958285428573997,-8.30336993179982E-5,
-0.220312733176437));
#49409=CARTESIAN_POINT('Origin',(0.,0.,-0.656687266823562));
#49410=CARTESIAN_POINT('',(-0.0957672392885407,-7.82302815145639E-5,-0.319187266823562));
#49411=CARTESIAN_POINT('',(-0.0959646250468222,2.82723803149889E-5,-0.310312733176438));
#49412=CARTESIAN_POINT('',(-0.095825,-8.02710626669594E-15,-0.656687266823562));
#49413=CARTESIAN_POINT('Ctrl Pts',(-0.0957672392885407,-7.82302815145602E-5,
-0.319187266823562));
#49414=CARTESIAN_POINT('Ctrl Pts',(-0.0958419044756827,-0.00948879151886152,
-0.318484797011526));
#49415=CARTESIAN_POINT('Ctrl Pts',(-0.0902748424426151,-0.05040894390654,
-0.315423784047275));
#49416=CARTESIAN_POINT('Ctrl Pts',(-0.0321311120597763,-0.108225222523459,
-0.31000422793081));
#49417=CARTESIAN_POINT('Ctrl Pts',(0.0726716307772531,-0.0863941041545113,
-0.302928598474167));
#49418=CARTESIAN_POINT('Ctrl Pts',(0.112129113562205,0.0131213202160467,
-0.295852969017526));
#49419=CARTESIAN_POINT('Ctrl Pts',(0.050761748924207,0.100838246705403,
-0.288777339560883));
#49420=CARTESIAN_POINT('Ctrl Pts',(-0.0562498327028107,0.0978829069520032,
-0.281701710104242));
#49421=CARTESIAN_POINT('Ctrl Pts',(-0.0950381444241069,0.0353555158065548,
-0.276838352525134));
#49422=CARTESIAN_POINT('Ctrl Pts',(-0.0959690028874658,0.00198308028543397,
-0.274333538098241));
#49423=CARTESIAN_POINT('Ctrl Pts',(-0.0959600152474598,3.3751409993089E-5,
-0.274187266823562));
#49424=CARTESIAN_POINT('Ctrl Pts',(-0.0959646250468222,2.82723803149913E-5,
-0.310312733176438));
#49425=CARTESIAN_POINT('Ctrl Pts',(-0.0958469111848973,-0.0297840779926777,
-0.308075424691734));
#49426=CARTESIAN_POINT('Ctrl Pts',(-0.0650257803347639,-0.0912346316416612,
-0.303479573054817));
#49427=CARTESIAN_POINT('Ctrl Pts',(0.0391678436633201,-0.105881945078975,
-0.296525178265685));
#49428=CARTESIAN_POINT('Ctrl Pts',(0.109958707539584,-0.02557711686569,
-0.289449548809043));
#49429=CARTESIAN_POINT('Ctrl Pts',(0.0818763211215267,0.07772627812099,
-0.2823739193524));
#49430=CARTESIAN_POINT('Ctrl Pts',(-0.0198280473347807,0.111139348611692,
-0.275298289895759));
#49431=CARTESIAN_POINT('Ctrl Pts',(-0.0872430988643529,0.0576722220502956,
-0.269611227837104));
#49432=CARTESIAN_POINT('Ctrl Pts',(-0.0957465609684512,0.0130616685541945,
-0.266282708930664));
#49433=CARTESIAN_POINT('Ctrl Pts',(-0.0956936940907658,4.22760440678986E-5,
-0.265312733176437));
#49434=CARTESIAN_POINT('Origin',(0.,0.,-0.656687266823562));
#49435=CARTESIAN_POINT('',(-0.0957330477189453,6.77082873043808E-5,-0.364187266823562));
#49436=CARTESIAN_POINT('',(-0.0957585699307466,-7.62084821080075E-5,-0.355312733176438));
#49437=CARTESIAN_POINT('',(-0.095825,-8.02710626669594E-15,-0.656687266823562));
#49438=CARTESIAN_POINT('Ctrl Pts',(-0.0957330477189453,6.77082873043813E-5,
-0.364187266823562));
#49439=CARTESIAN_POINT('Ctrl Pts',(-0.0955939884635277,-0.0207317147833155,
-0.36263605592481));
#49440=CARTESIAN_POINT('Ctrl Pts',(-0.0787712860380626,-0.0733605892247887,
-0.358726301873844));
#49441=CARTESIAN_POINT('Ctrl Pts',(0.00754897625919715,-0.112641555869212,
-0.352458004670662));
#49442=CARTESIAN_POINT('Ctrl Pts',(0.0981990237225277,-0.0556961299676074,
-0.345382375214021));
#49443=CARTESIAN_POINT('Ctrl Pts',(0.100549955365708,0.0513304356908642,
-0.338306745757378));
#49444=CARTESIAN_POINT('Ctrl Pts',(0.0124878480988304,0.11220142959062,
-0.331231116300736));
#49445=CARTESIAN_POINT('Ctrl Pts',(-0.0769455196192706,0.0761556323356412,
-0.324857956656131));
#49446=CARTESIAN_POINT('Ctrl Pts',(-0.0955912160292541,0.0221071779940261,
-0.320843340163739));
#49447=CARTESIAN_POINT('Ctrl Pts',(-0.0957672392885407,-7.82302815145602E-5,
-0.319187266823562));
#49448=CARTESIAN_POINT('Ctrl Pts',(-0.0957585699307466,-7.62084821080058E-5,
-0.355312733176438));
#49449=CARTESIAN_POINT('Ctrl Pts',(-0.095833385029768,-0.00982440707728614,
-0.354585226757233));
#49450=CARTESIAN_POINT('Ctrl Pts',(-0.090012622095492,-0.0510886319044539,
-0.351499177185813));
#49451=CARTESIAN_POINT('Ctrl Pts',(-0.0309943734581772,-0.108556230059475,
-0.34605458446218));
#49452=CARTESIAN_POINT('Ctrl Pts',(0.0735736570237532,-0.0856272343546855,
-0.338978955005538));
#49453=CARTESIAN_POINT('Ctrl Pts',(0.111985338737018,0.0142965093240165,
-0.331903325548895));
#49454=CARTESIAN_POINT('Ctrl Pts',(0.0497014532331962,0.101365042383611,
-0.324827696092254));
#49455=CARTESIAN_POINT('Ctrl Pts',(-0.0572732469911756,0.0972876222859135,
-0.317752066635611));
#49456=CARTESIAN_POINT('Ctrl Pts',(-0.0952073964263819,0.0346808621441382,
-0.312913745663673));
#49457=CARTESIAN_POINT('Ctrl Pts',(-0.0959710036937587,0.00164373596519372,
-0.310433967843948));
#49458=CARTESIAN_POINT('Ctrl Pts',(-0.0959646250468222,2.82723803149913E-5,
-0.310312733176438));
#49459=CARTESIAN_POINT('Origin',(0.,0.,-0.656687266823562));
#49460=CARTESIAN_POINT('',(-0.0959740869885037,-9.86262265154315E-6,-0.409187266823562));
#49461=CARTESIAN_POINT('',(-0.0957406735922206,7.06966245190496E-5,-0.400312733176438));
#49462=CARTESIAN_POINT('',(-0.095825,-8.02710626669594E-15,-0.656687266823562));
#49463=CARTESIAN_POINT('Ctrl Pts',(-0.0959740869885037,-9.86262265153463E-6,
-0.409187266823562));
#49464=CARTESIAN_POINT('Ctrl Pts',(-0.0959749085624466,-0.000561493444819199,
-0.409145857990308));
#49465=CARTESIAN_POINT('Ctrl Pts',(-0.0957226212003185,-0.0325318593928511,
-0.40674590600484));
#49466=CARTESIAN_POINT('Ctrl Pts',(-0.0604936699172284,-0.0953185347786495,
-0.401987410867158));
#49467=CARTESIAN_POINT('Ctrl Pts',(0.0462849239846546,-0.102969961087666,
-0.394911781410515));
#49468=CARTESIAN_POINT('Ctrl Pts',(0.111444796996209,-0.0180323158387254,
-0.387836151953873));
#49469=CARTESIAN_POINT('Ctrl Pts',(0.0763951494091263,0.0831197226767399,
-0.380760522497231));
#49470=CARTESIAN_POINT('Ctrl Pts',(-0.0273478910507391,0.109531730550394,
-0.373684893040589));
#49471=CARTESIAN_POINT('Ctrl Pts',(-0.0891473386466404,0.0532561389240456,
-0.368160474482699));
#49472=CARTESIAN_POINT('Ctrl Pts',(-0.0958054215155266,0.0108928289152016,
-0.364994599077024));
#49473=CARTESIAN_POINT('Ctrl Pts',(-0.0957330477189453,6.77082873043813E-5,
-0.364187266823562));
#49474=CARTESIAN_POINT('Ctrl Pts',(-0.0957406735922206,7.06966245190514E-5,
-0.400312733176438));
#49475=CARTESIAN_POINT('Ctrl Pts',(-0.0955923160348808,-0.0210601752103308,
-0.398736485670517));
#49476=CARTESIAN_POINT('Ctrl Pts',(-0.0783440141407614,-0.0740293659639809,
-0.394801695012381));
#49477=CARTESIAN_POINT('Ctrl Pts',(0.00872984600194528,-0.112556190631666,
-0.388508361202033));
#49478=CARTESIAN_POINT('Ctrl Pts',(0.0987777120733966,-0.054663240617283,
-0.38143273174539));
#49479=CARTESIAN_POINT('Ctrl Pts',(0.100006114225775,0.0523820903322742,
-0.374357102288749));
#49480=CARTESIAN_POINT('Ctrl Pts',(0.0113104914411958,0.112326217122388,
-0.367281472832106));
#49481=CARTESIAN_POINT('Ctrl Pts',(-0.0773901089245864,0.0754897857684629,
-0.360933349794669));
#49482=CARTESIAN_POINT('Ctrl Pts',(-0.0955908378373022,0.0217788151570939,
-0.356943769909447));
#49483=CARTESIAN_POINT('Ctrl Pts',(-0.0957585699307466,-7.62084821080058E-5,
-0.355312733176438));
#49484=CARTESIAN_POINT('Origin',(0.,0.,-0.656687266823562));
#49485=CARTESIAN_POINT('',(-0.0957106322133127,-5.59492053251305E-5,-0.454187266823562));
#49486=CARTESIAN_POINT('',(-0.0959720410064835,-1.57534720231084E-5,-0.445312733176438));
#49487=CARTESIAN_POINT('',(-0.095825,-8.02710626669594E-15,-0.656687266823562));
#49488=CARTESIAN_POINT('Ctrl Pts',(-0.0957106322133127,-5.59492053251263E-5,
-0.454187266823563));
#49489=CARTESIAN_POINT('Ctrl Pts',(-0.0957755559596934,-0.0119985666202428,
-0.453297116903593));
#49490=CARTESIAN_POINT('Ctrl Pts',(-0.0882017718506858,-0.0555050230914065,
-0.450048423831408));
#49491=CARTESIAN_POINT('Ctrl Pts',(-0.0235324529605039,-0.110414375714813,
-0.44444118760701));
#49492=CARTESIAN_POINT('Ctrl Pts',(0.07923206509802,-0.0804200407641335,
-0.437365558150368));
#49493=CARTESIAN_POINT('Ctrl Pts',(0.110752326466076,0.0218867699872954,
-0.430289928693726));
#49494=CARTESIAN_POINT('Ctrl Pts',(0.0426857011445824,0.104513340790562,
-0.423214299237084));
#49495=CARTESIAN_POINT('Ctrl Pts',(-0.0631402910989122,0.0932294692290819,
-0.416180078613696));
#49496=CARTESIAN_POINT('Ctrl Pts',(-0.0959281137738762,0.0308580128761358,
-0.411504401142522));
#49497=CARTESIAN_POINT('Ctrl Pts',(-0.0959740869885037,-9.86262265153463E-6,
-0.409187266823562));
#49498=CARTESIAN_POINT('Ctrl Pts',(-0.0959720410064835,-1.57534720231178E-5,
-0.445312733176438));
#49499=CARTESIAN_POINT('Ctrl Pts',(-0.0959740933575537,-0.000900961988616875,
-0.445246287736015));
#49500=CARTESIAN_POINT('Ctrl Pts',(-0.0955650009318915,-0.0332055331898721,
-0.442821299143378));
#49501=CARTESIAN_POINT('Ctrl Pts',(-0.0594907218526991,-0.0959476973028402,
-0.438037767398527));
#49502=CARTESIAN_POINT('Ctrl Pts',(0.0473622336949324,-0.10247889791293,
-0.430962137941886));
#49503=CARTESIAN_POINT('Ctrl Pts',(0.111627772406076,-0.0168625899039329,
-0.423886508485243));
#49504=CARTESIAN_POINT('Ctrl Pts',(0.0755192590508171,0.0839163142856434,
-0.416810879028601));
#49505=CARTESIAN_POINT('Ctrl Pts',(-0.0284950580593602,0.109238902681774,
-0.409735249571959));
#49506=CARTESIAN_POINT('Ctrl Pts',(-0.0894235522255543,0.0525762734766696,
-0.404235867621238));
#49507=CARTESIAN_POINT('Ctrl Pts',(-0.0958143038252681,0.0105580020614414,
-0.401095028822731));
#49508=CARTESIAN_POINT('Ctrl Pts',(-0.0957406735922206,7.06966245190514E-5,
-0.400312733176438));
#49509=CARTESIAN_POINT('Origin',(0.,0.,-0.656687266823562));
#49510=CARTESIAN_POINT('',(-0.095796229339445,8.13944495619803E-5,-0.499187266823562));
#49511=CARTESIAN_POINT('',(-0.0957047411432482,-5.19454942728911E-5,-0.490312733176438));
#49512=CARTESIAN_POINT('',(-0.095825,-8.02710626669594E-15,-0.656687266823562));
#49513=CARTESIAN_POINT('Ctrl Pts',(-0.095796229339445,8.13944495619877E-5,
-0.499187266823562));
#49514=CARTESIAN_POINT('Ctrl Pts',(-0.0955964171293276,-0.0231944520604812,
-0.497448375816877));
#49515=CARTESIAN_POINT('Ctrl Pts',(-0.075437632712349,-0.0783490658574657,
-0.493350941657977));
#49516=CARTESIAN_POINT('Ctrl Pts',(0.0163731327305643,-0.111701819859221,
-0.486894964346863));
#49517=CARTESIAN_POINT('Ctrl Pts',(0.10226912842285,-0.0478115777644791,
-0.479819334890221));
#49518=CARTESIAN_POINT('Ctrl Pts',(0.0962085431136162,0.0590682350665474,
-0.472743705433579));
#49519=CARTESIAN_POINT('Ctrl Pts',(0.00363743500867127,0.112835759078637,
-0.465668075976936));
#49520=CARTESIAN_POINT('Ctrl Pts',(-0.0801464535262578,0.0711425571216517,
-0.459482596440265));
#49521=CARTESIAN_POINT('Ctrl Pts',(-0.0956035338609357,0.0196446182990092,
-0.455655660055807));
#49522=CARTESIAN_POINT('Ctrl Pts',(-0.0957106322133127,-5.59492053251263E-5,
-0.454187266823563));
#49523=CARTESIAN_POINT('Ctrl Pts',(-0.0957047411432482,-5.1945494272879E-5,
-0.490312733176438));
#49524=CARTESIAN_POINT('Ctrl Pts',(-0.0957664443284886,-0.0123322917923352,
-0.489397546649299));
#49525=CARTESIAN_POINT('Ctrl Pts',(-0.0879063054038062,-0.0561846157158543,
-0.486123816969947));
#49526=CARTESIAN_POINT('Ctrl Pts',(-0.0223731015898872,-0.110655243614886,
-0.48049154413838));
#49527=CARTESIAN_POINT('Ctrl Pts',(0.0800710122382963,-0.0795846175196028,
-0.473415914681738));
#49528=CARTESIAN_POINT('Ctrl Pts',(0.110516738602258,0.023046994991323,
-0.466340285225096));
#49529=CARTESIAN_POINT('Ctrl Pts',(0.041587290010598,0.104955262561484,
-0.459264655768454));
#49530=CARTESIAN_POINT('Ctrl Pts',(-0.0637382953975096,0.0926062780139632,
-0.452255471752234));
#49531=CARTESIAN_POINT('Ctrl Pts',(-0.0959012432337274,0.0305203435488716,
-0.447604830888229));
#49532=CARTESIAN_POINT('Ctrl Pts',(-0.0959720410064835,-1.57534720231178E-5,
-0.445312733176438));
#49533=CARTESIAN_POINT('Origin',(0.,0.,-0.656687266823562));
#49534=CARTESIAN_POINT('',(-0.095825,-8.02710626669594E-15,-0.5435));
#49535=CARTESIAN_POINT('',(-0.0957990153585407,7.37030635558182E-5,-0.535312733176437));
#49536=CARTESIAN_POINT('',(-0.095825,-8.02710626669594E-15,-0.656687266823562));
#49537=CARTESIAN_POINT('',(-0.0953841396803776,-0.00918131376406525,-0.5435));
#49538=CARTESIAN_POINT('Origin',(0.,0.,-0.5435));
#49539=CARTESIAN_POINT('Ctrl Pts',(-0.0953841396803776,-0.00918131376406524,
-0.5435));
#49540=CARTESIAN_POINT('Ctrl Pts',(-0.0923605976477055,-0.0405927177292199,
-0.541141456847786));
#49541=CARTESIAN_POINT('Ctrl Pts',(-0.0529443191752485,-0.0996768450839476,
-0.536424370543358));
#49542=CARTESIAN_POINT('Ctrl Pts',(0.0542885591219757,-0.0990657329549278,
-0.529348741086716));
#49543=CARTESIAN_POINT('Ctrl Pts',(0.112485789500799,-0.00919905073578263,
-0.522273111630074));
#49544=CARTESIAN_POINT('Ctrl Pts',(0.0696476756938639,0.0888493431316701,
-0.515197482173432));
#49545=CARTESIAN_POINT('Ctrl Pts',(-0.0358739599293379,0.107052680846593,
-0.508121852716789));
#49546=CARTESIAN_POINT('Ctrl Pts',(-0.0911102694613287,0.0481602885445596,
-0.502785114266833));
#49547=CARTESIAN_POINT('Ctrl Pts',(-0.0958674322292328,0.00837572007059505,
-0.499806918969091));
#49548=CARTESIAN_POINT('Ctrl Pts',(-0.095796229339445,8.13944495619877E-5,
-0.499187266823562));
#49549=CARTESIAN_POINT('Ctrl Pts',(-0.0957990153585407,7.3703063555813E-5,
-0.535312733176437));
#49550=CARTESIAN_POINT('Ctrl Pts',(-0.0955942319159112,-0.0235299141747378,
-0.533548805562583));
#49551=CARTESIAN_POINT('Ctrl Pts',(-0.0749791628368817,-0.0789981539215374,
-0.529426334796515));
#49552=CARTESIAN_POINT('Ctrl Pts',(0.0175496669572723,-0.111531282490646,
-0.522945320878233));
#49553=CARTESIAN_POINT('Ctrl Pts',(0.102761745137553,-0.0467325866898933,
-0.515869691421591));
#49554=CARTESIAN_POINT('Ctrl Pts',(0.0955854583748553,0.0600719067187621,
-0.508794061964948));
#49555=CARTESIAN_POINT('Ctrl Pts',(0.00245303643899368,0.11286876447647,
-0.501718432508308));
#49556=CARTESIAN_POINT('Ctrl Pts',(-0.0805504964401501,0.0704700920038005,
-0.495557989578802));
#49557=CARTESIAN_POINT('Ctrl Pts',(-0.095607427974223,0.0193156027179515,
-0.491756089801513));
#49558=CARTESIAN_POINT('Ctrl Pts',(-0.0957047411432482,-5.1945494272879E-5,
-0.490312733176438));
#49559=CARTESIAN_POINT('Origin',(1.13809670924099E-17,0.,-0.0135));
#49560=CARTESIAN_POINT('',(-0.0872731800879825,-0.0845318995251531,-0.0135));
#49561=CARTESIAN_POINT('Ctrl Pts',(-0.0256835729485001,0.0924624001170202,
-0.0134999999999999));
#49562=CARTESIAN_POINT('Ctrl Pts',(-0.0286929696929738,0.0920530644409703,
-0.0134999999999999));
#49563=CARTESIAN_POINT('Ctrl Pts',(-0.0316740080847999,0.0914938944008697,
-0.0135000000000002));
#49564=CARTESIAN_POINT('Ctrl Pts',(-0.0346156128527234,0.0907835000445219,
-0.0135000000000001));
#49565=CARTESIAN_POINT('Ctrl Pts',(-0.0386263660453573,0.0898149075048917,
-0.0135000000000001));
#49566=CARTESIAN_POINT('Ctrl Pts',(-0.0425638695384247,0.0885654375663179,
-0.0135));
#49567=CARTESIAN_POINT('Ctrl Pts',(-0.0464123421802407,0.0870586227379721,
-0.0135));
#49568=CARTESIAN_POINT('Ctrl Pts',(-0.0499619860475324,0.0856688100739905,
-0.0134999999999999));
#49569=CARTESIAN_POINT('Ctrl Pts',(-0.053437219658575,0.0840585579962781,
-0.0135000000000001));
#49570=CARTESIAN_POINT('Ctrl Pts',(-0.05680648974238,0.0822549280939232,
-0.0135000000000001));
#49571=CARTESIAN_POINT('Ctrl Pts',(-0.0607057413385475,0.0801675897088359,
-0.0135000000000001));
#49572=CARTESIAN_POINT('Ctrl Pts',(-0.0644691098509119,0.0778193898967427,
-0.0135));
#49573=CARTESIAN_POINT('Ctrl Pts',(-0.0680778405577365,0.0752361825612141,
-0.0135));
#49574=CARTESIAN_POINT('Ctrl Pts',(-0.0716069103383439,0.0727099982361779,
-0.0135000000000001));
#49575=CARTESIAN_POINT('Ctrl Pts',(-0.0749921954747181,0.0699544156545884,
-0.0135000000000001));
#49576=CARTESIAN_POINT('Ctrl Pts',(-0.0781906931260397,0.0670135871053226,
-0.0135000000000001));
#49577=CARTESIAN_POINT('Ctrl Pts',(-0.0841982556543313,0.0614899903043682,
-0.0135));
#49578=CARTESIAN_POINT('Ctrl Pts',(-0.0895641926404807,0.0553073555873199,
-0.0135000000000001));
#49579=CARTESIAN_POINT('Ctrl Pts',(-0.09417415447868,0.0486046086051259,
-0.0135000000000001));
#49580=CARTESIAN_POINT('Ctrl Pts',(-0.0960082526817258,0.0459378845351681,
-0.0135000000000001));
#49581=CARTESIAN_POINT('Ctrl Pts',(-0.097722436957705,0.0431883046963393,
-0.0135000000000001));
#49582=CARTESIAN_POINT('Ctrl Pts',(-0.0993080945262219,0.0403628223276675,
-0.0135));
#49583=CARTESIAN_POINT('Ctrl Pts',(-0.100621192866324,0.0380230131015422,
-0.0135));
#49584=CARTESIAN_POINT('Ctrl Pts',(-0.101841576040244,0.0356391671272654,
-0.0135));
#49585=CARTESIAN_POINT('Ctrl Pts',(-0.102965121363602,0.0332172590887685,
-0.0135));
#49586=CARTESIAN_POINT('Ctrl Pts',(-0.104411047879092,0.0301004279488587,
-0.0135));
#49587=CARTESIAN_POINT('Ctrl Pts',(-0.105696927631408,0.0269200665199215,
-0.0135000000000001));
#49588=CARTESIAN_POINT('Ctrl Pts',(-0.106814378879639,0.0236857924562531,
-0.0135000000000001));
#49589=CARTESIAN_POINT('Ctrl Pts',(-0.10872275852689,0.0181623096139294,
-0.0135000000000001));
#49590=CARTESIAN_POINT('Ctrl Pts',(-0.110140714954151,0.0124819005222567,
-0.0135));
#49591=CARTESIAN_POINT('Ctrl Pts',(-0.111089665498783,0.00669929876611018,
-0.0135));
#49592=CARTESIAN_POINT('Ctrl Pts',(-0.111763452113654,0.00259345817783101,
-0.0135));
#49593=CARTESIAN_POINT('Ctrl Pts',(-0.112200243379474,-0.00157061108088781,
-0.0135000000000001));
#49594=CARTESIAN_POINT('Ctrl Pts',(-0.112403879549441,-0.00573895849727011,
-0.0135000000000001));
#49595=CARTESIAN_POINT('Ctrl Pts',(-0.112746158071992,-0.0127452570118909,
-0.0135));
#49596=CARTESIAN_POINT('Ctrl Pts',(-0.112435256625197,-0.0197769752940045,
-0.0135000000000001));
#49597=CARTESIAN_POINT('Ctrl Pts',(-0.111507238982716,-0.0267440426387617,
-0.0135000000000001));
#49598=CARTESIAN_POINT('Ctrl Pts',(-0.110923739318404,-0.0311246505828438,
-0.0135));
#49599=CARTESIAN_POINT('Ctrl Pts',(-0.110095815737416,-0.0354799462789394,
-0.0134999999999999));
#49600=CARTESIAN_POINT('Ctrl Pts',(-0.109027864350346,-0.0397884631534964,
-0.0134999999999999));
#49601=CARTESIAN_POINT('Ctrl Pts',(-0.108289706193421,-0.0427664703116023,
-0.0134999999999999));
#49602=CARTESIAN_POINT('Ctrl Pts',(-0.107435885652299,-0.0457239504344895,
-0.0135000000000001));
#49603=CARTESIAN_POINT('Ctrl Pts',(-0.10647336946096,-0.0486369389278256,
-0.0135000000000001));
#49604=CARTESIAN_POINT('Ctrl Pts',(-0.10365954094822,-0.0571527957555754,
-0.0134999999999999));
#49605=CARTESIAN_POINT('Ctrl Pts',(-0.09991451527938,-0.0653187550302201,
-0.0135000000000001));
#49606=CARTESIAN_POINT('Ctrl Pts',(-0.0952853579514916,-0.0729633148625617,
-0.0135000000000002));
#49607=CARTESIAN_POINT('Ctrl Pts',(-0.0928581545785142,-0.0769715824792622,
-0.0135000000000003));
#49608=CARTESIAN_POINT('Ctrl Pts',(-0.0901870237235777,-0.0808365421038318,
-0.0135000000000001));
#49609=CARTESIAN_POINT('Ctrl Pts',(-0.0872731800879837,-0.0845318995251519,
-0.0135000000000001));
#49610=CARTESIAN_POINT('',(-0.1215,-1.48794586096403E-17,-0.0135));
#49611=CARTESIAN_POINT('Origin',(0.,0.,-0.0135));
#49612=CARTESIAN_POINT('',(0.0125914725202458,-0.12102200839196,-0.0134999999999998));
#49613=CARTESIAN_POINT('Origin',(0.,0.,-0.0135));
#49614=CARTESIAN_POINT('Ctrl Pts',(0.0125914725202424,-0.12102200839196,
-0.0134999999999999));
#49615=CARTESIAN_POINT('Ctrl Pts',(0.01630909845269,-0.120270541987533,
-0.0134999999999999));
#49616=CARTESIAN_POINT('Ctrl Pts',(0.0199811919896631,-0.119336381645409,
-0.0135));
#49617=CARTESIAN_POINT('Ctrl Pts',(0.0235953222232064,-0.118214550041642,
-0.0135));
#49618=CARTESIAN_POINT('Ctrl Pts',(0.0298728004468691,-0.116266011110226,
-0.0135000000000001));
#49619=CARTESIAN_POINT('Ctrl Pts',(0.0359760464873946,-0.113751796213398,
-0.0135000000000001));
#49620=CARTESIAN_POINT('Ctrl Pts',(0.0418497129701972,-0.110722148829279,
-0.0135000000000002));
#49621=CARTESIAN_POINT('Ctrl Pts',(0.0452658144899046,-0.108960117725986,
-0.0135000000000003));
#49622=CARTESIAN_POINT('Ctrl Pts',(0.0485961822757404,-0.107027418200187,
-0.0134999999999999));
#49623=CARTESIAN_POINT('Ctrl Pts',(0.0518253785851629,-0.104937954428778,
-0.0134999999999999));
#49624=CARTESIAN_POINT('Ctrl Pts',(0.0558573654441519,-0.102329041974594,
-0.0134999999999999));
#49625=CARTESIAN_POINT('Ctrl Pts',(0.0597343728416072,-0.0994744335231951,
-0.0135000000000001));
#49626=CARTESIAN_POINT('Ctrl Pts',(0.0634335156525812,-0.0963933155043625,
-0.0135000000000001));
#49627=CARTESIAN_POINT('Ctrl Pts',(0.0666996161571287,-0.0936728903599141,
-0.0135000000000001));
#49628=CARTESIAN_POINT('Ctrl Pts',(0.0698300587296424,-0.0907719367810035,
-0.0135));
#49629=CARTESIAN_POINT('Ctrl Pts',(0.0727869511219022,-0.0877247167350274,
-0.0135));
#49630=CARTESIAN_POINT('Ctrl Pts',(0.0787244614333784,-0.0816058263446699,
-0.0135));
#49631=CARTESIAN_POINT('Ctrl Pts',(0.0839828754633012,-0.0748863675200879,
-0.0135));
#49632=CARTESIAN_POINT('Ctrl Pts',(0.0884251702134852,-0.0676735386298863,
-0.0135000000000001));
#49633=CARTESIAN_POINT('Ctrl Pts',(0.0901937988706099,-0.0648018660841556,
-0.0135000000000001));
#49634=CARTESIAN_POINT('Ctrl Pts',(0.0918325225091036,-0.0618517952811021,
-0.0135));
#49635=CARTESIAN_POINT('Ctrl Pts',(0.0933302931359342,-0.0588296707391292,
-0.0134999999999999));
#49636=CARTESIAN_POINT('Ctrl Pts',(0.0944446233987782,-0.0565812324436539,
-0.0134999999999999));
#49637=CARTESIAN_POINT('Ctrl Pts',(0.0954796740979294,-0.054294932786333,
-0.0135));
#49638=CARTESIAN_POINT('Ctrl Pts',(0.0964281978132539,-0.0519815122319335,
-0.0135000000000001));
#49639=CARTESIAN_POINT('Ctrl Pts',(0.0979408892394924,-0.0482921037528562,
-0.0135000000000001));
#49640=CARTESIAN_POINT('Ctrl Pts',(0.0992365826214292,-0.0445280346329004,
-0.0135000000000001));
#49641=CARTESIAN_POINT('Ctrl Pts',(0.100299532825755,-0.040700640312293,
-0.0135000000000001));
#49642=CARTESIAN_POINT('Ctrl Pts',(0.101687029451378,-0.0357046426793301,
-0.0135000000000001));
#49643=CARTESIAN_POINT('Ctrl Pts',(0.102678183721985,-0.0306005696481754,
-0.0135000000000001));
#49644=CARTESIAN_POINT('Ctrl Pts',(0.103279392849383,-0.0254317444710534,
-0.0135000000000001));
#49645=CARTESIAN_POINT('Ctrl Pts',(0.103615422494957,-0.0225427688831181,
-0.0135000000000001));
#49646=CARTESIAN_POINT('Ctrl Pts',(0.103829532743543,-0.0196319843360579,
-0.0135000000000001));
#49647=CARTESIAN_POINT('Ctrl Pts',(0.103921664321782,-0.0167123916178717,
-0.0135000000000001));
#49648=CARTESIAN_POINT('Ctrl Pts',(0.104174258631648,-0.00870783420299761,
-0.0135000000000001));
#49649=CARTESIAN_POINT('Ctrl Pts',(0.103512737427135,-0.00070037618932715,
-0.0135000000000001));
#49650=CARTESIAN_POINT('Ctrl Pts',(0.101968203321781,0.00714835440083033,
-0.0135000000000002));
#49651=CARTESIAN_POINT('Ctrl Pts',(0.101237186149509,0.0108631036071164,
-0.0135000000000003));
#49652=CARTESIAN_POINT('Ctrl Pts',(0.100307649317537,0.0145420857439938,
-0.0135));
#49653=CARTESIAN_POINT('Ctrl Pts',(0.0991794056182389,0.0181660256448864,
-0.0135));
#49654=CARTESIAN_POINT('Ctrl Pts',(0.098236594455864,0.0211943527629211,
-0.0135));
#49655=CARTESIAN_POINT('Ctrl Pts',(0.0971539272984628,0.0241854881404279,
-0.0135));
#49656=CARTESIAN_POINT('Ctrl Pts',(0.0959395234098873,0.0271085791501241,
-0.0135));
#49657=CARTESIAN_POINT('Ctrl Pts',(0.0930741567527453,0.0340055658888603,
-0.0135000000000001));
#49658=CARTESIAN_POINT('Ctrl Pts',(0.0894707573383288,0.0405524725288617,
-0.0135000000000001));
#49659=CARTESIAN_POINT('Ctrl Pts',(0.0851332279891031,0.046597744453004,
-0.0135000000000002));
#49660=CARTESIAN_POINT('Ctrl Pts',(0.0832222855077887,0.0492610502201462,
-0.0135000000000002));
#49661=CARTESIAN_POINT('Ctrl Pts',(0.0811684147236789,0.0518265208596175,
-0.0135));
#49662=CARTESIAN_POINT('Ctrl Pts',(0.0789701248920227,0.0542784487576638,
-0.0135000000000001));
#49663=CARTESIAN_POINT('Ctrl Pts',(0.0955814485598029,-0.00682768747159289,
-0.558323468161444));
#49664=CARTESIAN_POINT('Ctrl Pts',(0.0978299067420195,0.024648693217557,
-0.55596492500923));
#49665=CARTESIAN_POINT('Ctrl Pts',(0.0688009783410032,0.0894707042253711,
-0.551247838704802));
#49666=CARTESIAN_POINT('Ctrl Pts',(-0.0370370537006431,0.106721729527787,
-0.54417220924816));
#49667=CARTESIAN_POINT('Ctrl Pts',(-0.109384159856722,0.0277988167736781,
-0.537096579791517));
#49668=CARTESIAN_POINT('Ctrl Pts',(-0.0834684332867814,-0.0760133271640939,
-0.530020950334875));
#49669=CARTESIAN_POINT('Ctrl Pts',(0.0175496669572723,-0.111531282490646,
-0.522945320878233));
#49670=CARTESIAN_POINT('Ctrl Pts',(0.102761745137553,-0.0467325866898933,
-0.515869691421591));
#49671=CARTESIAN_POINT('Ctrl Pts',(0.0955854583748553,0.0600719067187621,
-0.508794061964948));
#49672=CARTESIAN_POINT('Ctrl Pts',(0.00245303643899368,0.11286876447647,
-0.501718432508308));
#49673=CARTESIAN_POINT('Ctrl Pts',(-0.0928813817133624,0.0641714062989615,
-0.494642803051664));
#49674=CARTESIAN_POINT('Ctrl Pts',(-0.104700197801406,-0.0422256787109809,
-0.487567173595023));
#49675=CARTESIAN_POINT('Ctrl Pts',(-0.0223731015898872,-0.110655243614886,
-0.48049154413838));
#49676=CARTESIAN_POINT('Ctrl Pts',(0.0800710122382963,-0.0795846175196028,
-0.473415914681738));
#49677=CARTESIAN_POINT('Ctrl Pts',(0.110516738602258,0.023046994991323,
-0.466340285225096));
#49678=CARTESIAN_POINT('Ctrl Pts',(0.041587290010598,0.104955262561484,
-0.459264655768454));
#49679=CARTESIAN_POINT('Ctrl Pts',(-0.0647367575428925,0.0924892125017532,
-0.452189026311811));
#49680=CARTESIAN_POINT('Ctrl Pts',(-0.11285050815591,-0.00314172710120585,
-0.44511339685517));
#49681=CARTESIAN_POINT('Ctrl Pts',(-0.0594907218526991,-0.0959476973028402,
-0.438037767398527));
#49682=CARTESIAN_POINT('Ctrl Pts',(0.0473622336949324,-0.10247889791293,
-0.430962137941886));
#49683=CARTESIAN_POINT('Ctrl Pts',(0.111627772406076,-0.0168625899039329,
-0.423886508485243));
#49684=CARTESIAN_POINT('Ctrl Pts',(0.0755192590508171,0.0839163142856434,
-0.416810879028601));
#49685=CARTESIAN_POINT('Ctrl Pts',(-0.0284950580593602,0.109238902681774,
-0.409735249571959));
#49686=CARTESIAN_POINT('Ctrl Pts',(-0.106887039546414,0.0363354797358826,
-0.402659620115318));
#49687=CARTESIAN_POINT('Ctrl Pts',(-0.0891677688863871,-0.069240271962092,
-0.395583990658674));
#49688=CARTESIAN_POINT('Ctrl Pts',(0.00872984600194528,-0.112556190631666,
-0.388508361202033));
#49689=CARTESIAN_POINT('Ctrl Pts',(0.0987777120733966,-0.054663240617283,
-0.38143273174539));
#49690=CARTESIAN_POINT('Ctrl Pts',(0.100006114225775,0.0523820903322742,
-0.374357102288749));
#49691=CARTESIAN_POINT('Ctrl Pts',(0.0113104914411958,0.112326217122388,
-0.367281472832106));
#49692=CARTESIAN_POINT('Ctrl Pts',(-0.0875553586799717,0.0712682638930122,
-0.360205843375464));
#49693=CARTESIAN_POINT('Ctrl Pts',(-0.107692719823917,-0.0338730625668669,
-0.353130213918822));
#49694=CARTESIAN_POINT('Ctrl Pts',(-0.0309943734581772,-0.108556230059475,
-0.34605458446218));
#49695=CARTESIAN_POINT('Ctrl Pts',(0.0735736570237532,-0.0856272343546855,
-0.338978955005538));
#49696=CARTESIAN_POINT('Ctrl Pts',(0.111985338737018,0.0142965093240165,
-0.331903325548895));
#49697=CARTESIAN_POINT('Ctrl Pts',(0.0497014532331962,0.101365042383611,
-0.324827696092254));
#49698=CARTESIAN_POINT('Ctrl Pts',(-0.0572732469911756,0.0972876222859135,
-0.317752066635611));
#49699=CARTESIAN_POINT('Ctrl Pts',(-0.112748687069072,0.00573060512783594,
-0.310676437178969));
#49700=CARTESIAN_POINT('Ctrl Pts',(-0.0668421683520032,-0.0909792877579244,
-0.303600807722327));
#49701=CARTESIAN_POINT('Ctrl Pts',(0.0391678436633201,-0.105881945078975,
-0.296525178265685));
#49702=CARTESIAN_POINT('Ctrl Pts',(0.109958707539584,-0.02557711686569,
-0.289449548809043));
#49703=CARTESIAN_POINT('Ctrl Pts',(0.0818763211215267,0.07772627812099,
-0.2823739193524));
#49704=CARTESIAN_POINT('Ctrl Pts',(-0.0198280473347807,0.111139348611692,
-0.275298289895759));
#49705=CARTESIAN_POINT('Ctrl Pts',(-0.103703327664771,0.0446175537450222,
-0.268222660439116));
#49706=CARTESIAN_POINT('Ctrl Pts',(-0.0943301031515697,-0.0620236883000746,
-0.261147030982475));
#49707=CARTESIAN_POINT('Ctrl Pts',(-0.000136639224089264,-0.112894143340924,
-0.254071401525832));
#49708=CARTESIAN_POINT('Ctrl Pts',(0.0941796886812631,-0.0622518474490773,
-0.24699577206919));
#49709=CARTESIAN_POINT('Ctrl Pts',(0.103811027648513,0.0443663927929224,
-0.239920142612548));
#49710=CARTESIAN_POINT('Ctrl Pts',(0.0200970195336817,0.111091026086466,
-0.232844513155906));
#49711=CARTESIAN_POINT('Ctrl Pts',(-0.0816879325475845,0.0779242449234631,
-0.225768883699263));
#49712=CARTESIAN_POINT('Ctrl Pts',(-0.110020298820829,-0.0253108695644216,
-0.218693254242622));
#49713=CARTESIAN_POINT('Ctrl Pts',(-0.0394240328282805,-0.105786822938669,
-0.211617624785979));
#49714=CARTESIAN_POINT('Ctrl Pts',(0.0666217428299838,-0.0911408231911627,
-0.204541995329337));
#49715=CARTESIAN_POINT('Ctrl Pts',(0.112762228567538,0.00545766237499973,
-0.197466365872695));
#49716=CARTESIAN_POINT('Ctrl Pts',(0.0575085792042569,0.0971486983708248,
-0.190390736416053));
#49717=CARTESIAN_POINT('Ctrl Pts',(-0.0494559375846015,0.101485055541974,
-0.183315106959411));
#49718=CARTESIAN_POINT('Ctrl Pts',(-0.111950403671619,0.0145675456862952,
-0.176239477502769));
#49719=CARTESIAN_POINT('Ctrl Pts',(-0.0737807157070053,-0.0854488870635276,
-0.169163848046127));
#49720=CARTESIAN_POINT('Ctrl Pts',(0.0307315052759879,-0.108630938394162,
-0.162088218589485));
#49721=CARTESIAN_POINT('Ctrl Pts',(0.107610409091042,-0.0341336512276352,
-0.155012589132842));
#49722=CARTESIAN_POINT('Ctrl Pts',(0.087727618468951,0.0710561149260017,
-0.147936959676201));
#49723=CARTESIAN_POINT('Ctrl Pts',(-0.0110385554953438,0.112353264263208,
-0.140861330219558));
#49724=CARTESIAN_POINT('Ctrl Pts',(-0.0998790212114998,0.0526240223292122,
-0.133785700762916));
#49725=CARTESIAN_POINT('Ctrl Pts',(-0.0989097454024145,-0.054423982807721,
-0.126710071306274));
#49726=CARTESIAN_POINT('Ctrl Pts',(-0.00900227708678451,-0.112534711150002,
-0.119634441849632));
#49727=CARTESIAN_POINT('Ctrl Pts',(0.0889998943616218,-0.0694559474299769,
-0.11255881239299));
#49728=CARTESIAN_POINT('Ctrl Pts',(0.106974694106382,0.0360767003792724,
-0.105483182936348));
#49729=CARTESIAN_POINT('Ctrl Pts',(0.0287593818097131,0.109169484310085,
-0.0984075534797054));
#49730=CARTESIAN_POINT('Ctrl Pts',(-0.0753158619846615,0.0840991055108705,
-0.0913319240230634));
#49731=CARTESIAN_POINT('Ctrl Pts',(-0.111668345874976,-0.016592766249281,
-0.0842562945664211));
#49732=CARTESIAN_POINT('Ctrl Pts',(-0.0476100055917889,-0.102363117493165,
-0.0771806651097791));
#49733=CARTESIAN_POINT('Ctrl Pts',(0.0592579954685063,-0.0960930036749314,
-0.0701050356531369));
#49734=CARTESIAN_POINT('Ctrl Pts',(0.112843133809849,-0.00341188826479888,
-0.0630294061964947));
#49735=CARTESIAN_POINT('Ctrl Pts',(0.064959386513852,0.0923265347892355,
-0.0559537767398527));
#49736=CARTESIAN_POINT('Ctrl Pts',(-0.04133108222025,0.105066452432841,
-0.0488781472832105));
#49737=CARTESIAN_POINT('Ctrl Pts',(-0.110464478017885,0.023293869539893,
-0.0418025178265684));
#49738=CARTESIAN_POINT('Ctrl Pts',(-0.0802560572708783,-0.0793513321432661,
-0.0347268883699262));
#49739=CARTESIAN_POINT('Ctrl Pts',(0.022090743255976,-0.110784791206306,
-0.0276512589132841));
#49740=CARTESIAN_POINT('Ctrl Pts',(0.104628794236781,-0.0423248975405764,
-0.0205756294566421));
#49741=CARTESIAN_POINT('Ctrl Pts',(0.0968448185910171,0.0282724219436266,
-0.0158585431522139));
#49742=CARTESIAN_POINT('Ctrl Pts',(0.0789701248920212,0.0542784487576661,
-0.0134999999999998));
#49743=CARTESIAN_POINT('Ctrl Pts',(0.104118029799121,-0.00743748267407433,
-0.553382312107629));
#49744=CARTESIAN_POINT('Ctrl Pts',(0.10656730253505,0.0268501201185417,
-0.551023768955415));
#49745=CARTESIAN_POINT('Ctrl Pts',(0.0749457391685725,0.097461521969475,
-0.546306682650987));
#49746=CARTESIAN_POINT('Ctrl Pts',(-0.0403449112665664,0.116253272811989,
-0.539231053194345));
#49747=CARTESIAN_POINT('Ctrl Pts',(-0.119153490422236,0.030281587869128,
-0.532155423737704));
#49748=CARTESIAN_POINT('Ctrl Pts',(-0.0909231755239786,-0.0828022381126562,
-0.52507979428106));
#49749=CARTESIAN_POINT('Ctrl Pts',(0.0191170648149215,-0.121492377117822,
-0.518004164824419));
#49750=CARTESIAN_POINT('Ctrl Pts',(0.111939613844073,-0.0509063728043841,
-0.510928535367777));
#49751=CARTESIAN_POINT('Ctrl Pts',(0.104122397739233,0.0654370557056445,
-0.503852905911134));
#49752=CARTESIAN_POINT('Ctrl Pts',(0.00267212230931772,0.122949312447366,
-0.496777276454493));
#49753=CARTESIAN_POINT('Ctrl Pts',(-0.101176814274421,0.0699026902600922,
-0.489701646997849));
#49754=CARTESIAN_POINT('Ctrl Pts',(-0.114051193813411,-0.0459969433458333,
-0.482626017541209));
#49755=CARTESIAN_POINT('Ctrl Pts',(-0.024371290591785,-0.120538097358036,
-0.475550388084565));
#49756=CARTESIAN_POINT('Ctrl Pts',(0.0872223236191749,-0.0866924879598705,
-0.468474758627924));
#49757=CARTESIAN_POINT('Ctrl Pts',(0.120387222169918,0.0251053708375774,
-0.461399129171281));
#49758=CARTESIAN_POINT('Ctrl Pts',(0.0453015388010052,0.114329038946442,
-0.454323499714639));
#49759=CARTESIAN_POINT('Ctrl Pts',(-0.0705185342188244,0.100749619601441,
-0.447247870257997));
#49760=CARTESIAN_POINT('Ctrl Pts',(-0.122929425616221,-0.00342232139052918,
-0.440172240801355));
#49761=CARTESIAN_POINT('Ctrl Pts',(-0.0648039639905137,-0.104516988991684,
-0.433096611344713));
#49762=CARTESIAN_POINT('Ctrl Pts',(0.0515922549145764,-0.111631504935852,
-0.426020981888072));
#49763=CARTESIAN_POINT('Ctrl Pts',(0.121597484751588,-0.0183686234574026,
-0.418945352431428));
#49764=CARTESIAN_POINT('Ctrl Pts',(0.0822640437316759,0.0914110577217115,
-0.411869722974788));
#49765=CARTESIAN_POINT('Ctrl Pts',(-0.031040011935954,0.118995260021906,
-0.404794093518143));
#49766=CARTESIAN_POINT('Ctrl Pts',(-0.116433347017861,0.0395806782478192,
-0.397718464061503));
#49767=CARTESIAN_POINT('Ctrl Pts',(-0.0971315308349326,-0.0754242670316685,
-0.390642834604859));
#49768=CARTESIAN_POINT('Ctrl Pts',(0.0095095270041183,-0.122608821971672,
-0.383567205148219));
#49769=CARTESIAN_POINT('Ctrl Pts',(0.107599758364324,-0.0595453302001996,
-0.376491575691576));
#49770=CARTESIAN_POINT('Ctrl Pts',(0.108937871709893,0.0570604455606625,
-0.369415946234934));
#49771=CARTESIAN_POINT('Ctrl Pts',(0.0123206553432845,0.122358309042094,
-0.362340316778292));
#49772=CARTESIAN_POINT('Ctrl Pts',(-0.09537511286419,0.077633383209312,
-0.35526468732165));
#49773=CARTESIAN_POINT('Ctrl Pts',(-0.117310984304234,-0.0368983373956488,
-0.348189057865008));
#49774=CARTESIAN_POINT('Ctrl Pts',(-0.0337625464768359,-0.118251616464473,
-0.341113428408365));
#49775=CARTESIAN_POINT('Ctrl Pts',(0.0801446758743825,-0.0932747836791719,
-0.334037798951723));
#49776=CARTESIAN_POINT('Ctrl Pts',(0.121986986087476,0.0155733607959493,
-0.326962169495081));
#49777=CARTESIAN_POINT('Ctrl Pts',(0.0541403950951408,0.11041816861441,
-0.319886540038439));
#49778=CARTESIAN_POINT('Ctrl Pts',(-0.0623884417611494,0.105976585507727,
-0.312810910581797));
#49779=CARTESIAN_POINT('Ctrl Pts',(-0.122818510672858,0.00624241758685821,
-0.305735281125155));
#49780=CARTESIAN_POINT('Ctrl Pts',(-0.0728119837183407,-0.0991048402866123,
-0.298659651668513));
#49781=CARTESIAN_POINT('Ctrl Pts',(0.0426660065855064,-0.115338485438668,
-0.29158402221187));
#49782=CARTESIAN_POINT('Ctrl Pts',(0.119779352173304,-0.0278614632454685,
-0.284508392755229));
#49783=CARTESIAN_POINT('Ctrl Pts',(0.0891888684553656,0.0846681763408569,
-0.277432763298586));
#49784=CARTESIAN_POINT('Ctrl Pts',(-0.021598932160662,0.121065438795552,
-0.270357133841944));
#49785=CARTESIAN_POINT('Ctrl Pts',(-0.112965291097392,0.048602441795822,
-0.263281504385302));
#49786=CARTESIAN_POINT('Ctrl Pts',(-0.102754924087013,-0.0675631550262395,
-0.25620587492866));
#49787=CARTESIAN_POINT('Ctrl Pts',(-0.000148842762062005,-0.122976957951858,
-0.249130245472017));
#49788=CARTESIAN_POINT('Ctrl Pts',(0.102591075782372,-0.0678116915511916,
-0.242054616015376));
#49789=CARTESIAN_POINT('Ctrl Pts',(0.113082609994372,0.0483288491281101,
-0.234978986558733));
#49790=CARTESIAN_POINT('Ctrl Pts',(0.0218919268352818,0.12101280048344,
-0.227903357102091));
#49791=CARTESIAN_POINT('Ctrl Pts',(-0.0889836544996118,0.0848838239769811,
-0.220827727645449));
#49792=CARTESIAN_POINT('Ctrl Pts',(-0.119846444302087,-0.0275714368348496,
-0.213752098188807));
#49793=CARTESIAN_POINT('Ctrl Pts',(-0.0429450765463997,-0.115234867738913,
-0.206676468732164));
#49794=CARTESIAN_POINT('Ctrl Pts',(0.0725718715269475,-0.0992808027908956,
-0.199600839275523));
#49795=CARTESIAN_POINT('Ctrl Pts',(0.122833261591181,0.00594509773973707,
-0.19252520981888));
#49796=CARTESIAN_POINT('Ctrl Pts',(0.0626447919916975,0.105825254004083,
-0.185449580362239));
#49797=CARTESIAN_POINT('Ctrl Pts',(-0.0538729519249248,0.110548900401667,
-0.178373950905596));
#49798=CARTESIAN_POINT('Ctrl Pts',(-0.12194893089753,0.015868603988742,
-0.171298321448954));
#49799=CARTESIAN_POINT('Ctrl Pts',(-0.0803702274063793,-0.0930805078143962,
-0.164222691992312));
#49800=CARTESIAN_POINT('Ctrl Pts',(0.033476200981565,-0.118332997158473,
-0.15714706253567));
#49801=CARTESIAN_POINT('Ctrl Pts',(0.117221322225793,-0.0371821997806217,
-0.150071433079028));
#49802=CARTESIAN_POINT('Ctrl Pts',(0.095562757539098,0.077402286769553,
-0.142995803622386));
#49803=CARTESIAN_POINT('Ctrl Pts',(-0.012024432223208,0.12238777182024,
-0.135920174165744));
#49804=CARTESIAN_POINT('Ctrl Pts',(-0.108799427749825,0.0573239850157162,
-0.128844544709101));
#49805=CARTESIAN_POINT('Ctrl Pts',(-0.107743583869089,-0.05928470376985,
-0.121768915252459));
#49806=CARTESIAN_POINT('Ctrl Pts',(-0.00980628948509182,-0.12258542411209,
-0.114693285795817));
#49807=CARTESIAN_POINT('Ctrl Pts',(0.0969486630814565,-0.0756592049315504,
-0.107617656339175));
#49808=CARTESIAN_POINT('Ctrl Pts',(0.11652883019189,0.0392987867597841,
-0.100542026882533));
#49809=CARTESIAN_POINT('Ctrl Pts',(0.0313279429992586,0.118919641748685,
-0.093466397425891));
#49810=CARTESIAN_POINT('Ctrl Pts',(-0.0820424808435396,0.0916101744177033,
-0.0863907679692487));
#49811=CARTESIAN_POINT('Ctrl Pts',(-0.121641681922771,-0.0180747012817188,
-0.0793151385126067));
#49812=CARTESIAN_POINT('Ctrl Pts',(-0.0518621558433564,-0.111505383922027,
-0.0722395090559645));
#49813=CARTESIAN_POINT('Ctrl Pts',(0.0645504523209409,-0.104675272983059,
-0.0651638795993224));
#49814=CARTESIAN_POINT('Ctrl Pts',(0.122921392651723,-0.00371661121879128,
-0.0580882501426802));
#49815=CARTESIAN_POINT('Ctrl Pts',(0.0707610466538411,0.100572412798501,
-0.0510126206860381));
#49816=CARTESIAN_POINT('Ctrl Pts',(-0.0450224485512517,0.114450159420278,
-0.043936991229396));
#49817=CARTESIAN_POINT('Ctrl Pts',(-0.120330294082271,0.0253742942739985,
-0.0368613617727538));
#49818=CARTESIAN_POINT('Ctrl Pts',(-0.0874238954148212,-0.086438367373384,
-0.0297857323161117));
#49819=CARTESIAN_POINT('Ctrl Pts',(0.0240637142381377,-0.120679215118723,
-0.0227101028594695));
#49820=CARTESIAN_POINT('Ctrl Pts',(0.113973413045475,-0.0461050236188597,
-0.0156344734028275));
#49821=CARTESIAN_POINT('Ctrl Pts',(0.10549423407871,0.0307974917180502,
-0.0109173870983993));
#49822=CARTESIAN_POINT('Ctrl Pts',(0.0860231136966225,0.0591261717661117,
-0.0085588439461853));
#49823=CARTESIAN_POINT('Ctrl Pts',(0.112654611038439,-0.00804727787655577,
-0.548441156053815));
#49824=CARTESIAN_POINT('Ctrl Pts',(0.11530469832808,0.0290515470195264,
-0.546082612901601));
#49825=CARTESIAN_POINT('Ctrl Pts',(0.0810904999961417,0.105452339713579,
-0.541365526597172));
#49826=CARTESIAN_POINT('Ctrl Pts',(-0.0436527688324896,0.125784816096191,
-0.534289897140531));
#49827=CARTESIAN_POINT('Ctrl Pts',(-0.128922820987751,0.0327643589645776,
-0.527214267683888));
#49828=CARTESIAN_POINT('Ctrl Pts',(-0.0983779177611759,-0.0895911490612184,
-0.520138638227246));
#49829=CARTESIAN_POINT('Ctrl Pts',(0.0206844626725709,-0.131453471744998,
-0.513063008770604));
#49830=CARTESIAN_POINT('Ctrl Pts',(0.121117482550592,-0.0550801589188749,
-0.505987379313962));
#49831=CARTESIAN_POINT('Ctrl Pts',(0.112659337103611,0.0708022046925269,
-0.49891174985732));
#49832=CARTESIAN_POINT('Ctrl Pts',(0.00289120817964168,0.133029860418262,
-0.491836120400678));
#49833=CARTESIAN_POINT('Ctrl Pts',(-0.10947224683548,0.0756339742212229,
-0.484760490944035));
#49834=CARTESIAN_POINT('Ctrl Pts',(-0.123402189825416,-0.0497682079806857,
-0.477684861487394));
#49835=CARTESIAN_POINT('Ctrl Pts',(-0.0263694795936829,-0.130420951101186,
-0.470609232030751));
#49836=CARTESIAN_POINT('Ctrl Pts',(0.0943736350000536,-0.0938003584001382,
-0.463533602574109));
#49837=CARTESIAN_POINT('Ctrl Pts',(0.130257705737577,0.0271637466838317,
-0.456457973117467));
#49838=CARTESIAN_POINT('Ctrl Pts',(0.0490157875914125,0.123702815331401,
-0.449382343660825));
#49839=CARTESIAN_POINT('Ctrl Pts',(-0.0763003108947565,0.109010026701128,
-0.442306714204182));
#49840=CARTESIAN_POINT('Ctrl Pts',(-0.133008343076533,-0.00370291567985249,
-0.435231084747541));
#49841=CARTESIAN_POINT('Ctrl Pts',(-0.0701172061283284,-0.113086280680527,
-0.428155455290898));
#49842=CARTESIAN_POINT('Ctrl Pts',(0.0558222761342205,-0.120784111958774,
-0.421079825834257));
#49843=CARTESIAN_POINT('Ctrl Pts',(0.1315671970971,-0.0198746570108724,
-0.414004196377613));
#49844=CARTESIAN_POINT('Ctrl Pts',(0.0890088284125349,0.0989058011577798,
-0.406928566920972));
#49845=CARTESIAN_POINT('Ctrl Pts',(-0.0335849658125481,0.128751617362039,
-0.39985293746433));
#49846=CARTESIAN_POINT('Ctrl Pts',(-0.125979654489307,0.0428258767597559,
-0.392777308007688));
#49847=CARTESIAN_POINT('Ctrl Pts',(-0.105095292783478,-0.081608262101245,
-0.385701678551046));
#49848=CARTESIAN_POINT('Ctrl Pts',(0.0102892080062914,-0.132661453311677,
-0.378626049094403));
#49849=CARTESIAN_POINT('Ctrl Pts',(0.116421804655251,-0.0644274197831163,
-0.371550419637762));
#49850=CARTESIAN_POINT('Ctrl Pts',(0.117869629194011,0.0617388007890509,
-0.364474790181119));
#49851=CARTESIAN_POINT('Ctrl Pts',(0.0133308192453733,0.132390400961799,
-0.357399160724477));
#49852=CARTESIAN_POINT('Ctrl Pts',(-0.103194867048408,0.0839985025256118,
-0.350323531267834));
#49853=CARTESIAN_POINT('Ctrl Pts',(-0.126929248784551,-0.0399236122244308,
-0.343247901811194));
#49854=CARTESIAN_POINT('Ctrl Pts',(-0.0365307194954948,-0.127947002869472,
-0.33617227235455));
#49855=CARTESIAN_POINT('Ctrl Pts',(0.0867156947250119,-0.100922333003658,
-0.329096642897909));
#49856=CARTESIAN_POINT('Ctrl Pts',(0.131988633437934,0.0168502122678822,
-0.322021013441266));
#49857=CARTESIAN_POINT('Ctrl Pts',(0.0585793369570855,0.11947129484521,
-0.314945383984625));
#49858=CARTESIAN_POINT('Ctrl Pts',(-0.0675036365311233,0.114665548729541,
-0.307869754527982));
#49859=CARTESIAN_POINT('Ctrl Pts',(-0.132888334276644,0.00675423004588044,
-0.30079412507134));
#49860=CARTESIAN_POINT('Ctrl Pts',(-0.0787817990846783,-0.1072303928153,
-0.293718495614698));
#49861=CARTESIAN_POINT('Ctrl Pts',(0.0461641695076928,-0.124795025798362,
-0.286642866158056));
#49862=CARTESIAN_POINT('Ctrl Pts',(0.129599996807024,-0.0301458096252471,
-0.279567236701414));
#49863=CARTESIAN_POINT('Ctrl Pts',(0.0965014157892046,0.0916100745607239,
-0.272491607244771));
#49864=CARTESIAN_POINT('Ctrl Pts',(-0.0233698169865435,0.130991528979412,
-0.26541597778813));
#49865=CARTESIAN_POINT('Ctrl Pts',(-0.122227254530014,0.0525873298466217,
-0.258340348331487));
#49866=CARTESIAN_POINT('Ctrl Pts',(-0.111179745022457,-0.0731026217524041,
-0.251264718874846));
#49867=CARTESIAN_POINT('Ctrl Pts',(-0.000161046300034822,-0.133059772562792,
-0.244189089418203));
#49868=CARTESIAN_POINT('Ctrl Pts',(0.111002462883481,-0.0733715356533056,
-0.237113459961561));
#49869=CARTESIAN_POINT('Ctrl Pts',(0.122354192340231,0.0522913054632976,
-0.230037830504919));
#49870=CARTESIAN_POINT('Ctrl Pts',(0.023686834136882,0.130934574880413,
-0.222962201048277));
#49871=CARTESIAN_POINT('Ctrl Pts',(-0.0962793764516391,0.0918434030304992,
-0.215886571591634));
#49872=CARTESIAN_POINT('Ctrl Pts',(-0.129672589783346,-0.0298320041052777,
-0.208810942134993));
#49873=CARTESIAN_POINT('Ctrl Pts',(-0.0464661202645189,-0.124682912539157,
-0.20173531267835));
#49874=CARTESIAN_POINT('Ctrl Pts',(0.0785220002239111,-0.107420782390629,
-0.194659683221709));
#49875=CARTESIAN_POINT('Ctrl Pts',(0.132904294614823,0.00643253310447447,
-0.187584053765066));
#49876=CARTESIAN_POINT('Ctrl Pts',(0.0677810047791383,0.114501809637341,
-0.180508424308424));
#49877=CARTESIAN_POINT('Ctrl Pts',(-0.0582899662652481,0.119612745261361,
-0.173432794851782));
#49878=CARTESIAN_POINT('Ctrl Pts',(-0.13194745812344,0.0171696622911887,
-0.16635716539514));
#49879=CARTESIAN_POINT('Ctrl Pts',(-0.0869597391057534,-0.100712128565265,
-0.159281535938498));
#49880=CARTESIAN_POINT('Ctrl Pts',(0.036220896687142,-0.128035055922783,
-0.152205906481855));
#49881=CARTESIAN_POINT('Ctrl Pts',(0.126832235360543,-0.0402307483336081,
-0.145130277025213));
#49882=CARTESIAN_POINT('Ctrl Pts',(0.103397896609245,0.0837484586131044,
-0.138054647568571));
#49883=CARTESIAN_POINT('Ctrl Pts',(-0.0130103089510719,0.132422279377272,
-0.130979018111929));
#49884=CARTESIAN_POINT('Ctrl Pts',(-0.117719834288151,0.0620239477022202,
-0.123903388655287));
#49885=CARTESIAN_POINT('Ctrl Pts',(-0.116577422335763,-0.0641454247319789,
-0.116827759198645));
#49886=CARTESIAN_POINT('Ctrl Pts',(-0.0106103018833993,-0.132636137074179,
-0.109752129742003));
#49887=CARTESIAN_POINT('Ctrl Pts',(0.104897431801291,-0.0818624624331239,
-0.102676500285361));
#49888=CARTESIAN_POINT('Ctrl Pts',(0.126082966277398,0.0425208731402957,
-0.0956008708287183));
#49889=CARTESIAN_POINT('Ctrl Pts',(0.0338965041888041,0.128669799187284,
-0.0885252413720764));
#49890=CARTESIAN_POINT('Ctrl Pts',(-0.0887690997024177,0.099121243324536,
-0.0814496119154342));
#49891=CARTESIAN_POINT('Ctrl Pts',(-0.131615017970567,-0.0195566363141564,
-0.0743739824587921));
#49892=CARTESIAN_POINT('Ctrl Pts',(-0.0561143060949239,-0.120647650350888,
-0.0672983530021499));
#49893=CARTESIAN_POINT('Ctrl Pts',(0.0698429091733757,-0.113257542291187,
-0.0602227235455079));
#49894=CARTESIAN_POINT('Ctrl Pts',(0.132999651493598,-0.00402133417278372,
-0.0531470940888656));
#49895=CARTESIAN_POINT('Ctrl Pts',(0.0765627067938301,0.108818290807766,
-0.0460714646322236));
#49896=CARTESIAN_POINT('Ctrl Pts',(-0.0487138148822533,0.123833866407714,
-0.0389958351755814));
#49897=CARTESIAN_POINT('Ctrl Pts',(-0.130196110146656,0.027454719008104,
-0.0319202057189393));
#49898=CARTESIAN_POINT('Ctrl Pts',(-0.094591733558764,-0.0935254026035021,
-0.0248445762622972));
#49899=CARTESIAN_POINT('Ctrl Pts',(0.0260366852202995,-0.13057363903114,
-0.017768946805655));
#49900=CARTESIAN_POINT('Ctrl Pts',(0.123318031854169,-0.0498851496971432,
-0.010693317349013));
#49901=CARTESIAN_POINT('Ctrl Pts',(0.114143649566402,0.0333225614924737,
-0.00597623104458479));
#49902=CARTESIAN_POINT('Ctrl Pts',(0.0930761025012238,0.0639738947745574,
-0.00361768789237075));
#49903=CARTESIAN_POINT('Ctrl Pts',(0.121191192277757,-0.00865707307903722,
-0.5435));
#49904=CARTESIAN_POINT('Ctrl Pts',(0.124042094121111,0.0312529739205111,
-0.541141456847786));
#49905=CARTESIAN_POINT('Ctrl Pts',(0.0872352608237108,0.113443157457683,
-0.536424370543358));
#49906=CARTESIAN_POINT('Ctrl Pts',(-0.0469606263984128,0.135316359380393,
-0.529348741086716));
#49907=CARTESIAN_POINT('Ctrl Pts',(-0.138692151553265,0.0352471300600274,
-0.522273111630074));
#49908=CARTESIAN_POINT('Ctrl Pts',(-0.105832659998373,-0.0963800600097806,
-0.515197482173431));
#49909=CARTESIAN_POINT('Ctrl Pts',(0.02225186053022,-0.141414566372174,
-0.50812185271679));
#49910=CARTESIAN_POINT('Ctrl Pts',(0.130295351257111,-0.0592539450333656,
-0.501046223260147));
#49911=CARTESIAN_POINT('Ctrl Pts',(0.121196276467989,0.0761673536794093,
-0.493970593803505));
#49912=CARTESIAN_POINT('Ctrl Pts',(0.00311029404996583,0.143110408389158,
-0.486894964346863));
#49913=CARTESIAN_POINT('Ctrl Pts',(-0.117767679396539,0.0813652581823536,
-0.479819334890221));
#49914=CARTESIAN_POINT('Ctrl Pts',(-0.132753185837421,-0.0535394726155382,
-0.472743705433579));
#49915=CARTESIAN_POINT('Ctrl Pts',(-0.0283676685955808,-0.140303804844337,
-0.465668075976936));
#49916=CARTESIAN_POINT('Ctrl Pts',(0.101524946380932,-0.100908228840406,
-0.458592446520295));
#49917=CARTESIAN_POINT('Ctrl Pts',(0.140128189305237,0.0292221225300861,
-0.451516817063652));
#49918=CARTESIAN_POINT('Ctrl Pts',(0.0527300363818198,0.13307659171636,
-0.444441187607011));
#49919=CARTESIAN_POINT('Ctrl Pts',(-0.0820820875706887,0.117270433800816,
-0.437365558150368));
#49920=CARTESIAN_POINT('Ctrl Pts',(-0.143087260536844,-0.00398350996917575,
-0.430289928693726));
#49921=CARTESIAN_POINT('Ctrl Pts',(-0.0754304482661432,-0.121655572369371,
-0.423214299237084));
#49922=CARTESIAN_POINT('Ctrl Pts',(0.0600522973538647,-0.129936718981696,
-0.416138669780442));
#49923=CARTESIAN_POINT('Ctrl Pts',(0.141536909442611,-0.0213806905643422,
-0.409063040323799));
#49924=CARTESIAN_POINT('Ctrl Pts',(0.0957536130933939,0.106400544593848,
-0.401987410867158));
#49925=CARTESIAN_POINT('Ctrl Pts',(-0.036129919689142,0.138507974702171,
-0.394911781410515));
#49926=CARTESIAN_POINT('Ctrl Pts',(-0.135525961960754,0.0460710752716928,
-0.387836151953873));
#49927=CARTESIAN_POINT('Ctrl Pts',(-0.113059054732024,-0.0877922571708217,
-0.380760522497231));
#49928=CARTESIAN_POINT('Ctrl Pts',(0.0110688890084644,-0.142714084651682,
-0.373684893040588));
#49929=CARTESIAN_POINT('Ctrl Pts',(0.125243850946179,-0.0693095093660329,
-0.366609263583947));
#49930=CARTESIAN_POINT('Ctrl Pts',(0.126801386678129,0.0664171560174392,
-0.359533634127304));
#49931=CARTESIAN_POINT('Ctrl Pts',(0.014340983147462,0.142422492881504,
-0.352458004670663));
#49932=CARTESIAN_POINT('Ctrl Pts',(-0.111014621232627,0.0903636218419115,
-0.34538237521402));
#49933=CARTESIAN_POINT('Ctrl Pts',(-0.136547513264868,-0.0429488870532126,
-0.338306745757379));
#49934=CARTESIAN_POINT('Ctrl Pts',(-0.0392988925141536,-0.13764238927447,
-0.331231116300736));
#49935=CARTESIAN_POINT('Ctrl Pts',(0.0932867135756414,-0.108569882328145,
-0.324155486844094));
#49936=CARTESIAN_POINT('Ctrl Pts',(0.141990280788392,0.0181270637398149,
-0.317079857387452));
#49937=CARTESIAN_POINT('Ctrl Pts',(0.0630182788190301,0.12852442107601,
-0.31000422793081));
#49938=CARTESIAN_POINT('Ctrl Pts',(-0.0726188313010971,0.123354511951355,
-0.302928598474168));
#49939=CARTESIAN_POINT('Ctrl Pts',(-0.14295815788043,0.00726604250490275,
-0.295852969017526));
#49940=CARTESIAN_POINT('Ctrl Pts',(-0.0847516144510158,-0.115355945343988,
-0.288777339560883));
#49941=CARTESIAN_POINT('Ctrl Pts',(0.0496623324298792,-0.134251566158055,
-0.281701710104241));
#49942=CARTESIAN_POINT('Ctrl Pts',(0.139420641440745,-0.0324301560050256,
-0.274626080647599));
#49943=CARTESIAN_POINT('Ctrl Pts',(0.103813963123044,0.0985519727805908,
-0.267550451190957));
#49944=CARTESIAN_POINT('Ctrl Pts',(-0.0251407018124249,0.140917619163273,
-0.260474821734315));
#49945=CARTESIAN_POINT('Ctrl Pts',(-0.131489217962636,0.0565722178974215,
-0.253399192277673));
#49946=CARTESIAN_POINT('Ctrl Pts',(-0.119604565957901,-0.0786420884785688,
-0.246323562821031));
#49947=CARTESIAN_POINT('Ctrl Pts',(-0.000173249838007723,-0.143142587173726,
-0.239247933364388));
#49948=CARTESIAN_POINT('Ctrl Pts',(0.11941384998459,-0.0789313797554197,
-0.232172303907747));
#49949=CARTESIAN_POINT('Ctrl Pts',(0.131625774686089,0.0562537617984851,
-0.225096674451104));
#49950=CARTESIAN_POINT('Ctrl Pts',(0.0254817414384823,0.140856349277387,
-0.218021044994462));
#49951=CARTESIAN_POINT('Ctrl Pts',(-0.103575098403667,0.0988029820840171,
-0.21094541553782));
#49952=CARTESIAN_POINT('Ctrl Pts',(-0.139498735264605,-0.0320925713757056,
-0.203869786081178));
#49953=CARTESIAN_POINT('Ctrl Pts',(-0.0499871639826382,-0.134130957339402,
-0.196794156624536));
#49954=CARTESIAN_POINT('Ctrl Pts',(0.0844721289208749,-0.115560761990362,
-0.189718527167894));
#49955=CARTESIAN_POINT('Ctrl Pts',(0.142975327638465,0.0069199684692118,
-0.182642897711252));
#49956=CARTESIAN_POINT('Ctrl Pts',(0.0729172175665789,0.123178365270598,
-0.175567268254609));
#49957=CARTESIAN_POINT('Ctrl Pts',(-0.0627069806055713,0.128676590121054,
-0.168491638797968));
#49958=CARTESIAN_POINT('Ctrl Pts',(-0.141945985349352,0.0184707205936354,
-0.161416009341325));
#49959=CARTESIAN_POINT('Ctrl Pts',(-0.0935492508051274,-0.108343749316133,
-0.154340379884683));
#49960=CARTESIAN_POINT('Ctrl Pts',(0.0389655923927191,-0.137737114687094,
-0.147264750428041));
#49961=CARTESIAN_POINT('Ctrl Pts',(0.136443148495294,-0.0432792968865944,
-0.140189120971399));
#49962=CARTESIAN_POINT('Ctrl Pts',(0.111233035679392,0.0900946304566556,
-0.133113491514757));
#49963=CARTESIAN_POINT('Ctrl Pts',(-0.0139961856789359,0.142456786934305,
-0.126037862058115));
#49964=CARTESIAN_POINT('Ctrl Pts',(-0.126640240826477,0.0667239103887243,
-0.118962232601472));
#49965=CARTESIAN_POINT('Ctrl Pts',(-0.125411260802437,-0.0690061456941079,
-0.11188660314483));
#49966=CARTESIAN_POINT('Ctrl Pts',(-0.0114143142817069,-0.142686850036267,
-0.104810973688188));
#49967=CARTESIAN_POINT('Ctrl Pts',(0.112846200521126,-0.0880657199346974,
-0.097735344231546));
#49968=CARTESIAN_POINT('Ctrl Pts',(0.135637102362906,0.0457429595208074,
-0.0906597147749039));
#49969=CARTESIAN_POINT('Ctrl Pts',(0.0364650653783499,0.138419956625884,
-0.0835840853182618));
#49970=CARTESIAN_POINT('Ctrl Pts',(-0.0954957185612961,0.106632312231369,
-0.0765084558616196));
#49971=CARTESIAN_POINT('Ctrl Pts',(-0.141588354018362,-0.0210385713465942,
-0.0694328264049776));
#49972=CARTESIAN_POINT('Ctrl Pts',(-0.0603664563464917,-0.129789916779749,
-0.0623571969483353));
#49973=CARTESIAN_POINT('Ctrl Pts',(0.0751353660258105,-0.121839811599314,
-0.0552815674916933));
#49974=CARTESIAN_POINT('Ctrl Pts',(0.143077910335472,-0.00432605712677605,
-0.0482059380350511));
#49975=CARTESIAN_POINT('Ctrl Pts',(0.0823643669338191,0.117064168817031,
-0.041130308578409));
#49976=CARTESIAN_POINT('Ctrl Pts',(-0.0524051812132549,0.13321757339515,
-0.0340546791217669));
#49977=CARTESIAN_POINT('Ctrl Pts',(-0.140061926211041,0.0295351437422096,
-0.0269790496651247));
#49978=CARTESIAN_POINT('Ctrl Pts',(-0.101759571702707,-0.10061243783362,
-0.0199034202084826));
#49979=CARTESIAN_POINT('Ctrl Pts',(0.0280096562024612,-0.140468062943556,
-0.0128277907518404));
#49980=CARTESIAN_POINT('Ctrl Pts',(0.132662650662863,-0.0536652757754266,
-0.00575216129519843));
#49981=CARTESIAN_POINT('Ctrl Pts',(0.122793065054095,0.0358476312668972,
-0.00103507499077024));
#49982=CARTESIAN_POINT('Ctrl Pts',(0.100129091305825,0.068821617783003,
0.0013234681614438));
#49983=CARTESIAN_POINT('Ctrl Pts',(-0.121526217441981,0.000102663445846418,
-0.0254892650149941));
#49984=CARTESIAN_POINT('Ctrl Pts',(-0.121242244193571,-0.0314487625136614,
-0.0236273167461569));
#49985=CARTESIAN_POINT('Ctrl Pts',(-0.10862906823349,-0.0631956500232495,
-0.0217653684773198));
#49986=CARTESIAN_POINT('Ctrl Pts',(-0.0865150928032345,-0.0855637784226379,
-0.0199034202084826));
#49987=CARTESIAN_POINT('Ctrl Pts',(-0.0611643925841885,-0.111205830856965,
-0.017768946805655));
#49988=CARTESIAN_POINT('Ctrl Pts',(-0.0233281783799959,-0.124522749137967,
-0.0156344734028274));
#49989=CARTESIAN_POINT('Ctrl Pts',(0.0125914725202458,-0.12102200839196,
-0.0134999999999998));
#49990=CARTESIAN_POINT('',(-0.0397408188803946,0.087195744963362,-0.5435));
#49991=CARTESIAN_POINT('Ctrl Pts',(-0.0397589391997285,0.0873393895763303,
-0.5435));
#49992=CARTESIAN_POINT('Ctrl Pts',(-0.0371904915887145,0.0889602232112557,
-0.5435));
#49993=CARTESIAN_POINT('Ctrl Pts',(-0.034547455834076,0.0904480486342698,
-0.5435));
#49994=CARTESIAN_POINT('Ctrl Pts',(-0.0318374226014847,0.0917946820255231,
-0.5435));
#49995=CARTESIAN_POINT('Ctrl Pts',(-0.0281424054768352,0.0936307604106386,
-0.5435));
#49996=CARTESIAN_POINT('Ctrl Pts',(-0.0243229557383007,0.0952045898844149,
-0.5435));
#49997=CARTESIAN_POINT('Ctrl Pts',(-0.0204062890282129,0.0965240534970721,
-0.5435));
#49998=CARTESIAN_POINT('Ctrl Pts',(-0.0167937500951651,0.0977410612294859,
-0.5435));
#49999=CARTESIAN_POINT('Ctrl Pts',(-0.0130965167986539,0.0987413727747821,
-0.5435));
#50000=CARTESIAN_POINT('Ctrl Pts',(-0.00935615524967915,0.0995254364772876,
-0.5435));
#50001=CARTESIAN_POINT('Ctrl Pts',(-0.00502742217475035,0.100432836052822,
-0.5435));
#50002=CARTESIAN_POINT('Ctrl Pts',(-0.000635102360800403,0.101053058129917,
-0.5435));
#50003=CARTESIAN_POINT('Ctrl Pts',(0.00378981819427666,0.101393852742248,
-0.5435));
#50004=CARTESIAN_POINT('Ctrl Pts',(0.00811702703254377,0.101727121880114,
-0.5435));
#50005=CARTESIAN_POINT('Ctrl Pts',(0.0124815444740136,0.101792241042985,
-0.5435));
#50006=CARTESIAN_POINT('Ctrl Pts',(0.0168220483608817,0.101595391107322,
-0.5435));
#50007=CARTESIAN_POINT('Ctrl Pts',(0.0249746128899566,0.101225657121392,
-0.5435));
#50008=CARTESIAN_POINT('Ctrl Pts',(0.033059285085718,0.0999386418970613,
-0.5435));
#50009=CARTESIAN_POINT('Ctrl Pts',(0.0408991675195905,0.0977672662931198,
-0.5435));
#50010=CARTESIAN_POINT('Ctrl Pts',(0.0440182920238849,0.0969033769540376,
-0.5435));
#50011=CARTESIAN_POINT('Ctrl Pts',(0.0470988160191229,0.095898938611735,
-0.5435));
#50012=CARTESIAN_POINT('Ctrl Pts',(0.0501296723833096,0.0947537415835819,
-0.5435));
#50013=CARTESIAN_POINT('Ctrl Pts',(0.0526395802787472,0.0938053828633346,
-0.5435));
#50014=CARTESIAN_POINT('Ctrl Pts',(0.0551067701615479,0.0927636927312978,
-0.5435));
#50015=CARTESIAN_POINT('Ctrl Pts',(0.0575242429130301,0.0916305982235789,
-0.5435));
#50016=CARTESIAN_POINT('Ctrl Pts',(0.060635351146661,0.0901723895838809,
-0.5435));
#50017=CARTESIAN_POINT('Ctrl Pts',(0.0636646925010064,0.0885626376171208,
-0.5435));
#50018=CARTESIAN_POINT('Ctrl Pts',(0.0665996639859203,0.0868033222099646,
-0.5435));
#50019=CARTESIAN_POINT('Ctrl Pts',(0.0716119961421378,0.0837987706381539,
-0.5435));
#50020=CARTESIAN_POINT('Ctrl Pts',(0.0763495113381208,0.0803587684725567,
-0.5435));
#50021=CARTESIAN_POINT('Ctrl Pts',(0.0807934344329792,0.0765390108759656,
-0.5435));
#50022=CARTESIAN_POINT('Ctrl Pts',(0.083948765500447,0.0738268577721766,
-0.5435));
#50023=CARTESIAN_POINT('Ctrl Pts',(0.0869599760588301,0.0709177615381115,
-0.5435));
#50024=CARTESIAN_POINT('Ctrl Pts',(0.0897953293542451,0.0678555190520308,
-0.5435));
#50025=CARTESIAN_POINT('Ctrl Pts',(0.0945610893247136,0.0627083958756595,
-0.5435));
#50026=CARTESIAN_POINT('Ctrl Pts',(0.0988428232231053,0.0571219441198984,
-0.5435));
#50027=CARTESIAN_POINT('Ctrl Pts',(0.102610261682682,0.0511883432169625,
-0.5435));
#50028=CARTESIAN_POINT('Ctrl Pts',(0.104979073270572,0.0474575370664183,
-0.5435));
#50029=CARTESIAN_POINT('Ctrl Pts',(0.107144374825992,0.043589008576509,
-0.5435));
#50030=CARTESIAN_POINT('Ctrl Pts',(0.109095735641908,0.0396020278398452,
-0.5435));
#50031=CARTESIAN_POINT('Ctrl Pts',(0.110444498668307,0.0368462626524366,
-0.5435));
#50032=CARTESIAN_POINT('Ctrl Pts',(0.111691464616707,0.0340318757008926,
-0.5435));
#50033=CARTESIAN_POINT('Ctrl Pts',(0.112826566212854,0.031181703065903,
-0.5435));
#50034=CARTESIAN_POINT('Ctrl Pts',(0.11614493200818,0.0228494838048033,
-0.5435));
#50035=CARTESIAN_POINT('Ctrl Pts',(0.118525049958407,0.0141867394355863,
-0.5435));
#50036=CARTESIAN_POINT('Ctrl Pts',(0.119892735971079,0.00535510104883141,
-0.5435));
#50037=CARTESIAN_POINT('Ctrl Pts',(0.120609853674274,0.000724415221322913,
-0.5435));
#50038=CARTESIAN_POINT('Ctrl Pts',(0.12104799608301,-0.00395328391685804,
-0.5435));
#50039=CARTESIAN_POINT('Ctrl Pts',(0.121191192277757,-0.00865707307903657,
-0.5435));
#50040=CARTESIAN_POINT('Ctrl Pts',(-0.0397589391997287,0.0873393895763303,
-0.5435));
#50041=CARTESIAN_POINT('Ctrl Pts',(-0.0655870913757108,0.0753780187149155,
-0.541365526597173));
#50042=CARTESIAN_POINT('Ctrl Pts',(-0.091691234429318,0.0444812340450679,
-0.538636437655985));
#50043=CARTESIAN_POINT('Ctrl Pts',(-0.0958680473392353,0.00803042275043827,
-0.535907348714798));
#50044=CARTESIAN_POINT('Ctrl Pts',(-0.0957990153585407,7.37030635558182E-5,
-0.535312733176438));
#50045=CARTESIAN_POINT('Origin',(-1.13809670924099E-17,0.,-0.5435));
#50046=CARTESIAN_POINT('Ctrl Pts',(0.0681458046084942,-0.100801883029112,
-0.5435));
#50047=CARTESIAN_POINT('Ctrl Pts',(0.0648149048055578,-0.102615870197094,
-0.5435));
#50048=CARTESIAN_POINT('Ctrl Pts',(0.0614014517271168,-0.104260638022271,
-0.5435));
#50049=CARTESIAN_POINT('Ctrl Pts',(0.0579117686900797,-0.10572438322058,
-0.5435));
#50050=CARTESIAN_POINT('Ctrl Pts',(0.0518504450541602,-0.10826680133515,
-0.5435));
#50051=CARTESIAN_POINT('Ctrl Pts',(0.0455589824493805,-0.110263892026136,
-0.5435));
#50052=CARTESIAN_POINT('Ctrl Pts',(0.0391120749818753,-0.111718567430527,
-0.5435));
#50053=CARTESIAN_POINT('Ctrl Pts',(0.0353625795407656,-0.112564600792189,
-0.5435));
#50054=CARTESIAN_POINT('Ctrl Pts',(0.0315690566392495,-0.113224785984647,
-0.5435));
#50055=CARTESIAN_POINT('Ctrl Pts',(0.0277522696084378,-0.11369985104087,
-0.5435));
#50056=CARTESIAN_POINT('Ctrl Pts',(0.0229866093069774,-0.114293019761256,
-0.5435));
#50057=CARTESIAN_POINT('Ctrl Pts',(0.0181817399541562,-0.11459835491698,
-0.5435));
#50058=CARTESIAN_POINT('Ctrl Pts',(0.0133675253247798,-0.11461584389042,
-0.5435));
#50059=CARTESIAN_POINT('Ctrl Pts',(0.00911690029736573,-0.114631285467901,
-0.5435));
#50060=CARTESIAN_POINT('Ctrl Pts',(0.00485415397265722,-0.114421235647892,
-0.5435));
#50061=CARTESIAN_POINT('Ctrl Pts',(0.000630336365389325,-0.113987583954121,
-0.5435));
#50062=CARTESIAN_POINT('Ctrl Pts',(-0.00785120378156423,-0.113116799608654,
-0.5435));
#50063=CARTESIAN_POINT('Ctrl Pts',(-0.0161985641326431,-0.111349438130382,
-0.5435));
#50064=CARTESIAN_POINT('Ctrl Pts',(-0.0242378739522401,-0.108679541554347,
-0.5435));
#50065=CARTESIAN_POINT('Ctrl Pts',(-0.0274386034479911,-0.107616562652764,
-0.5435));
#50066=CARTESIAN_POINT('Ctrl Pts',(-0.0305902132968484,-0.10641002520364,
-0.5435));
#50067=CARTESIAN_POINT('Ctrl Pts',(-0.0336801620372295,-0.105057687860788,
-0.5435));
#50068=CARTESIAN_POINT('Ctrl Pts',(-0.0359790613319563,-0.104051558754799,
-0.5435));
#50069=CARTESIAN_POINT('Ctrl Pts',(-0.0382415656149683,-0.102965465891595,
-0.5435));
#50070=CARTESIAN_POINT('Ctrl Pts',(-0.0404552192737468,-0.101802978363352,
-0.5435));
#50071=CARTESIAN_POINT('Ctrl Pts',(-0.0439854985319678,-0.0999490724496493,
-0.5435));
#50072=CARTESIAN_POINT('Ctrl Pts',(-0.0473975398291214,-0.0978984910598355,
-0.5435));
#50073=CARTESIAN_POINT('Ctrl Pts',(-0.0506719957326547,-0.0956497968821656,
-0.5435));
#50074=CARTESIAN_POINT('Ctrl Pts',(-0.054946246470959,-0.0927145053307493,
-0.5435));
#50075=CARTESIAN_POINT('Ctrl Pts',(-0.0589863515765622,-0.0894416590788099,
-0.5435));
#50076=CARTESIAN_POINT('Ctrl Pts',(-0.0627693636876284,-0.0858685577421909,
-0.5435));
#50077=CARTESIAN_POINT('Ctrl Pts',(-0.0648837750791162,-0.0838714702501929,
-0.5435));
#50078=CARTESIAN_POINT('Ctrl Pts',(-0.0669188095625019,-0.0817793079138408,
-0.5435));
#50079=CARTESIAN_POINT('Ctrl Pts',(-0.0688660649399109,-0.0796019918163136,
-0.5435));
#50080=CARTESIAN_POINT('Ctrl Pts',(-0.0742047958657111,-0.0736325104016171,
-0.5435));
#50081=CARTESIAN_POINT('Ctrl Pts',(-0.0788451394315893,-0.0670732251057521,
-0.5435));
#50082=CARTESIAN_POINT('Ctrl Pts',(-0.0827070282539586,-0.0600679424715311,
-0.5435));
#50083=CARTESIAN_POINT('Ctrl Pts',(-0.0845348325968156,-0.0567523923325412,
-0.5435));
#50084=CARTESIAN_POINT('Ctrl Pts',(-0.0861875716311489,-0.0533366354792091,
-0.5435));
#50085=CARTESIAN_POINT('Ctrl Pts',(-0.0876527120283092,-0.0498353171887534,
-0.5435));
#50086=CARTESIAN_POINT('Ctrl Pts',(-0.0888770503705417,-0.0469094554490365,
-0.5435));
#50087=CARTESIAN_POINT('Ctrl Pts',(-0.0899703462593087,-0.0439221864599506,
-0.5435));
#50088=CARTESIAN_POINT('Ctrl Pts',(-0.0909189876323078,-0.040902363707549,
-0.5435));
#50089=CARTESIAN_POINT('Ctrl Pts',(-0.0931572896503075,-0.0337771469996449,
-0.5435));
#50090=CARTESIAN_POINT('Ctrl Pts',(-0.0946051988332896,-0.026445709106482,
-0.5435));
#50091=CARTESIAN_POINT('Ctrl Pts',(-0.0951682868431173,-0.0190266560863368,
-0.5435));
#50092=CARTESIAN_POINT('Ctrl Pts',(-0.0954163614839278,-0.0157581103510265,
-0.5435));
#50093=CARTESIAN_POINT('Ctrl Pts',(-0.0954920586844475,-0.0124726380609223,
-0.5435));
#50094=CARTESIAN_POINT('Ctrl Pts',(-0.0953841396803774,-0.00918131376406761,
-0.5435));
#50095=CARTESIAN_POINT('Origin',(0.,0.,-0.5435));
#50096=CARTESIAN_POINT('Origin',(0.,0.,-0.656687266823562));
#50097=CARTESIAN_POINT('Ctrl Pts',(-0.120941017178877,-0.0116413213914294,
-0.558323468161444));
#50098=CARTESIAN_POINT('Ctrl Pts',(-0.11710735835321,-0.0514689820412212,
-0.55596492500923));
#50099=CARTESIAN_POINT('Ctrl Pts',(-0.0671300264001348,-0.126383894366809,
-0.551247838704802));
#50100=CARTESIAN_POINT('Ctrl Pts',(0.0688344370813445,-0.125609043089213,
-0.544172209248159));
#50101=CARTESIAN_POINT('Ctrl Pts',(0.142624820499317,-0.0116638107424766,
-0.537096579791518));
#50102=CARTESIAN_POINT('Ctrl Pts',(0.0883088191683241,0.112655311145294,
-0.530020950334875));
#50103=CARTESIAN_POINT('Ctrl Pts',(-0.0454858975362832,0.135735984585036,
-0.522945320878234));
#50104=CARTESIAN_POINT('Ctrl Pts',(-0.138342174559802,0.0367335649717563,
-0.51586969142159));
#50105=CARTESIAN_POINT('Ctrl Pts',(-0.10682330188696,-0.0952826647968933,
-0.50879406196495));
#50106=CARTESIAN_POINT('Ctrl Pts',(0.0207600900262283,-0.141630796899509,
-0.501718432508306));
#50107=CARTESIAN_POINT('Ctrl Pts',(0.129670744621718,-0.0606220370298399,
-0.494642803051665));
#50108=CARTESIAN_POINT('Ctrl Pts',(0.121986308252591,0.0748947619158391,
-0.487567173595023));
#50109=CARTESIAN_POINT('Ctrl Pts',(0.00461203604021712,0.143068559645755,
-0.48049154413838));
#50110=CARTESIAN_POINT('Ctrl Pts',(-0.116908498038604,0.0825965493599512,
-0.473415914681739));
#50111=CARTESIAN_POINT('Ctrl Pts',(-0.133307060630641,-0.052144710735923,
-0.466340285225096));
#50112=CARTESIAN_POINT('Ctrl Pts',(-0.0298376523318702,-0.139998399680144,
-0.459264655768454));
#50113=CARTESIAN_POINT('Ctrl Pts',(0.100461214812515,-0.101967492333341,
-0.452189026311812));
#50114=CARTESIAN_POINT('Ctrl Pts',(0.140426899719575,0.0277510310822455,
-0.445113396855169));
#50115=CARTESIAN_POINT('Ctrl Pts',(0.0541227517773754,0.132516263042559,
-0.438037767398528));
#50116=CARTESIAN_POINT('Ctrl Pts',(-0.0808477600960478,0.118124808842324,
-0.430962137941885));
#50117=CARTESIAN_POINT('Ctrl Pts',(-0.143121165975879,-0.00248272619463574,
-0.423886508485243));
#50118=CARTESIAN_POINT('Ctrl Pts',(-0.0767021225665899,-0.120857834339742,
-0.416810879028602));
#50119=CARTESIAN_POINT('Ctrl Pts',(0.0586863372203009,-0.130559355827306,
-0.409735249571959));
#50120=CARTESIAN_POINT('Ctrl Pts',(0.141304908270695,-0.0228638285875853,
-0.402659620115317));
#50121=CARTESIAN_POINT('Ctrl Pts',(0.0968641863105561,0.105390517142955,
-0.395583990658675));
#50122=CARTESIAN_POINT('Ctrl Pts',(-0.0346753849482346,0.138879261798831,
-0.388508361202033));
#50123=CARTESIAN_POINT('Ctrl Pts',(-0.135035360971776,0.047489819885674,
-0.38143273174539));
#50124=CARTESIAN_POINT('Ctrl Pts',(-0.113973529173592,-0.0866017686993902,
-0.374357102288749));
#50125=CARTESIAN_POINT('Ctrl Pts',(0.00957162134612276,-0.142822322338734,
-0.367281472832107));
#50126=CARTESIAN_POINT('Ctrl Pts',(0.124510110955252,-0.0706191473108742,
-0.360205843375464));
#50127=CARTESIAN_POINT('Ctrl Pts',(0.127490942623884,0.0650837248780568,
-0.353130213918822));
#50128=CARTESIAN_POINT('Ctrl Pts',(0.0158337964415146,0.142264270234911,
-0.34605458446218));
#50129=CARTESIAN_POINT('Ctrl Pts',(-0.110060866297358,0.0915228791372047,
-0.338978955005538));
#50130=CARTESIAN_POINT('Ctrl Pts',(-0.13699041908937,-0.0415145368890392,
-0.331903325548895));
#50131=CARTESIAN_POINT('Ctrl Pts',(-0.0407402046988056,-0.137222692789984,
-0.324827696092254));
#50132=CARTESIAN_POINT('Ctrl Pts',(0.0921430017160038,-0.109542224417149,
-0.317752066635611));
#50133=CARTESIAN_POINT('Ctrl Pts',(0.142172578114354,0.0166369987607558,
-0.31067643717897));
#50134=CARTESIAN_POINT('Ctrl Pts',(0.0643626662592367,0.127856477690649,
-0.303600807722327));
#50135=CARTESIAN_POINT('Ctrl Pts',(-0.0713212071316596,0.124109295013498,
-0.296525178265685));
#50136=CARTESIAN_POINT('Ctrl Pts',(-0.142874101523106,0.0087648622021492,
-0.289449548809043));
#50137=CARTESIAN_POINT('Ctrl Pts',(-0.08595670814417,-0.114460805608188,
-0.282373919352401));
#50138=CARTESIAN_POINT('Ctrl Pts',(0.0482516911858636,-0.134765002850031,
-0.275298289895759));
#50139=CARTESIAN_POINT('Ctrl Pts',(0.13907288047591,-0.0338904944134862,
-0.268222660439116));
#50140=CARTESIAN_POINT('Ctrl Pts',(0.10484178397496,0.0974578474438835,
-0.261147030982475));
#50141=CARTESIAN_POINT('Ctrl Pts',(-0.0236615005155487,0.14117352828645,
-0.254071401525832));
#50142=CARTESIAN_POINT('Ctrl Pts',(-0.130888712240556,0.0579480517657311,
-0.24699577206919));
#50143=CARTESIAN_POINT('Ctrl Pts',(-0.120422721711377,-0.0773834594148965,
-0.239920142612548));
#50144=CARTESIAN_POINT('Ctrl Pts',(-0.00167439346369711,-0.143132903632313,
-0.232844513155906));
#50145=CARTESIAN_POINT('Ctrl Pts',(0.118579524725311,-0.0801793490316698,
-0.225768883699263));
#50146=CARTESIAN_POINT('Ctrl Pts',(0.132208480778061,0.0548702952924991,
-0.218693254242622));
#50147=CARTESIAN_POINT('Ctrl Pts',(0.0269575181460965,0.140581378256179,
-0.211617624785979));
#50148=CARTESIAN_POINT('Ctrl Pts',(-0.102533247759778,0.0998837564234286,
-0.204541995329338));
#50149=CARTESIAN_POINT('Ctrl Pts',(-0.139827627438852,-0.0306278680121232,
-0.197466365872695));
#50150=CARTESIAN_POINT('Ctrl Pts',(-0.051391063975439,-0.133599364702921,
-0.190390736416053));
#50151=CARTESIAN_POINT('Ctrl Pts',(0.0832555873046201,-0.116440280236949,
-0.183315106959411));
#50152=CARTESIAN_POINT('Ctrl Pts',(0.143040040704376,0.00542018897790831,
-0.176239477502769));
#50153=CARTESIAN_POINT('Ctrl Pts',(0.0742049962749289,0.122406904572045,
-0.169163848046126));
#50154=CARTESIAN_POINT('Ctrl Pts',(-0.0613540878947369,0.129327133537324,
-0.162088218589485));
#50155=CARTESIAN_POINT('Ctrl Pts',(-0.141744479849913,0.0199583105394808,
-0.155012589132842));
#50156=CARTESIAN_POINT('Ctrl Pts',(-0.0946803232670462,-0.107356734608036,
-0.1479369596762));
#50157=CARTESIAN_POINT('Ctrl Pts',(0.0375189856164575,-0.138138178990805,
-0.140861330219558));
#50158=CARTESIAN_POINT('Ctrl Pts',(0.135981775009837,-0.0447078191806976,
-0.133785700762916));
#50159=CARTESIAN_POINT('Ctrl Pts',(0.112171755540986,0.0889231755496423,
-0.126710071306274));
#50160=CARTESIAN_POINT('Ctrl Pts',(-0.0125014551897662,0.14259571800196,
-0.119634441849632));
#50161=CARTESIAN_POINT('Ctrl Pts',(-0.125933540022816,0.068048371817411,
-0.11255881239299));
#50162=CARTESIAN_POINT('Ctrl Pts',(-0.126128043361885,-0.0676872214632633,
-0.105483182936348));
#50163=CARTESIAN_POINT('Ctrl Pts',(-0.0129100623071776,-0.142559170771431,
-0.0984075534797053));
#50164=CARTESIAN_POINT('Ctrl Pts',(0.111916446224502,-0.0892445667815422,
-0.0913319240230634));
#50165=CARTESIAN_POINT('Ctrl Pts',(0.136109354430927,0.0443184882404931,
-0.0842562945664211));
#50166=CARTESIAN_POINT('Ctrl Pts',(0.037914698287885,0.138029015203821,
-0.077180665109779));
#50167=CARTESIAN_POINT('Ctrl Pts',(-0.0943722248490409,0.107629675951055,
-0.070105035653137));
#50168=CARTESIAN_POINT('Ctrl Pts',(-0.141801168750683,-0.0195558834566498,
-0.0630294061964947));
#50169=CARTESIAN_POINT('Ctrl Pts',(-0.0617243330219531,-0.129143403898395,
-0.0559537767398526));
#50170=CARTESIAN_POINT('Ctrl Pts',(0.0738536247947097,-0.122633056272086,
-0.0488781472832105));
#50171=CARTESIAN_POINT('Ctrl Pts',(0.143024424514937,-0.00580350448589463,
-0.0418025178265684));
#50172=CARTESIAN_POINT('Ctrl Pts',(0.0835879551182714,0.116150495748595,
-0.0347268883699262));
#50173=CARTESIAN_POINT('Ctrl Pts',(-0.0510057890185001,0.133844017127003,
-0.0276512589132841));
#50174=CARTESIAN_POINT('Ctrl Pts',(-0.139745887278106,0.0308288207471279,
-0.020575629456642));
#50175=CARTESIAN_POINT('Ctrl Pts',(-0.115110781316278,-0.0557915541778742,
-0.0158585431522139));
#50176=CARTESIAN_POINT('Ctrl Pts',(-0.0872731800879813,-0.0845318995251544,
-0.0134999999999998));
#50177=CARTESIAN_POINT('Ctrl Pts',(-0.112422058012711,-0.0108213188489747,
-0.553382312107629));
#50178=CARTESIAN_POINT('Ctrl Pts',(-0.108858438118042,-0.0478435606038874,
-0.551023768955415));
#50179=CARTESIAN_POINT('Ctrl Pts',(-0.0624014573251726,-0.117481544605856,
-0.546306682650987));
#50180=CARTESIAN_POINT('Ctrl Pts',(0.0639858110948882,-0.116761273044451,
-0.539231053194346));
#50181=CARTESIAN_POINT('Ctrl Pts',(0.132578476833144,-0.0108422240735788,
-0.532155423737702));
#50182=CARTESIAN_POINT('Ctrl Pts',(0.0820884380101708,0.104719988474086,
-0.525079794281062));
#50183=CARTESIAN_POINT('Ctrl Pts',(-0.0422819183339681,0.126174883338888,
-0.518004164824418));
#50184=CARTESIAN_POINT('Ctrl Pts',(-0.128597496008848,0.0341460909507685,
-0.510928535367777));
#50185=CARTESIAN_POINT('Ctrl Pts',(-0.0992987798678985,-0.0885710532230661,
-0.503852905911134));
#50186=CARTESIAN_POINT('Ctrl Pts',(0.0192977709276737,-0.131654471219413,
-0.496777276454492));
#50187=CARTESIAN_POINT('Ctrl Pts',(0.120536872555428,-0.0563518839413863,
-0.48970164699785));
#50188=CARTESIAN_POINT('Ctrl Pts',(0.113393719872933,0.0696192529660752,
-0.482626017541208));
#50189=CARTESIAN_POINT('Ctrl Pts',(0.0042871690297017,0.132990959456715,
-0.475550388084567));
#50190=CARTESIAN_POINT('Ctrl Pts',(-0.108673585316681,0.0767785345319212,
-0.468474758627923));
#50191=CARTESIAN_POINT('Ctrl Pts',(-0.123917050255629,-0.0484716916737979,
-0.461399129171282));
#50192=CARTESIAN_POINT('Ctrl Pts',(-0.0277359192080814,-0.130137058358367,
-0.454323499714639));
#50193=CARTESIAN_POINT('Ctrl Pts',(0.09338483157435,-0.0947850084769385,
-0.447247870257998));
#50194=CARTESIAN_POINT('Ctrl Pts',(0.130535375301742,0.0257962773839288,
-0.440172240801355));
#50195=CARTESIAN_POINT('Ctrl Pts',(0.0503104015664444,0.123181955625226,
-0.433096611344713));
#50196=CARTESIAN_POINT('Ctrl Pts',(-0.0751529281606134,0.109804220455419,
-0.426020981888071));
#50197=CARTESIAN_POINT('Ctrl Pts',(-0.133039860251789,-0.00230784554978795,
-0.418945352431429));
#50198=CARTESIAN_POINT('Ctrl Pts',(-0.0712993050168028,-0.112344734486044,
-0.411869722974787));
#50199=CARTESIAN_POINT('Ctrl Pts',(0.0545525328084189,-0.121362890914093,
-0.404794093518144));
#50200=CARTESIAN_POINT('Ctrl Pts',(0.131351537845866,-0.0212533243379652,
-0.397718464061502));
#50201=CARTESIAN_POINT('Ctrl Pts',(0.0900411740100795,0.09796691898755,
-0.39064283460486));
#50202=CARTESIAN_POINT('Ctrl Pts',(-0.0322328869824028,0.129096751382686,
-0.383567205148218));
#50203=CARTESIAN_POINT('Ctrl Pts',(-0.12552361092253,0.0441446864822037,
-0.376491575691576));
#50204=CARTESIAN_POINT('Ctrl Pts',(-0.105945352598744,-0.0805016303966285,
-0.369415946234934));
#50205=CARTESIAN_POINT('Ctrl Pts',(0.00889740631714755,-0.132762066848893,
-0.362340316778292));
#50206=CARTESIAN_POINT('Ctrl Pts',(0.115739748544344,-0.065644808196452,
-0.355264687321649));
#50207=CARTESIAN_POINT('Ctrl Pts',(0.118510613537825,0.0604992951489926,
-0.348189057865007));
#50208=CARTESIAN_POINT('Ctrl Pts',(0.0147184803272866,0.13224332335348,
-0.341113428408366));
#50209=CARTESIAN_POINT('Ctrl Pts',(-0.102308293616468,0.0850761029455781,
-0.334037798951723));
#50210=CARTESIAN_POINT('Ctrl Pts',(-0.127340956784515,-0.0385902961904772,
-0.326962169495081));
#50211=CARTESIAN_POINT('Ctrl Pts',(-0.0378705071524625,-0.127556869367809,
-0.319886540038439));
#50212=CARTESIAN_POINT('Ctrl Pts',(0.0856525447364202,-0.101826184329603,
-0.312810910581796));
#50213=CARTESIAN_POINT('Ctrl Pts',(0.132158089930304,0.0154651059125196,
-0.305735281125155));
#50214=CARTESIAN_POINT('Ctrl Pts',(0.0598290271475602,0.118850400695567,
-0.298659651668512));
#50215=CARTESIAN_POINT('Ctrl Pts',(-0.0662974156553768,0.115367165659667,
-0.291584022211871));
#50216=CARTESIAN_POINT('Ctrl Pts',(-0.132810198761499,0.0081474744462084,
-0.284508392755229));
#50217=CARTESIAN_POINT('Ctrl Pts',(-0.0799020072344259,-0.106398305789285,
-0.277432763298586));
#50218=CARTESIAN_POINT('Ctrl Pts',(0.0448528923622785,-0.125272296545025,
-0.270357133841945));
#50219=CARTESIAN_POINT('Ctrl Pts',(0.129276731762003,-0.0315032833186536,
-0.263281504385301));
#50220=CARTESIAN_POINT('Ctrl Pts',(0.0974568380118396,0.0905930182720822,
-0.256205874928661));
#50221=CARTESIAN_POINT('Ctrl Pts',(-0.0219948090869163,0.131229412130745,
-0.249130245472017));
#50222=CARTESIAN_POINT('Ctrl Pts',(-0.121669047804956,0.0538662514115874,
-0.242054616015376));
#50223=CARTESIAN_POINT('Ctrl Pts',(-0.111940270737605,-0.0719326492078258,
-0.234978986558733));
#50224=CARTESIAN_POINT('Ctrl Pts',(-0.00155645093370914,-0.133050771119941,
-0.227903357102092));
#50225=CARTESIAN_POINT('Ctrl Pts',(0.110226906625662,-0.0745315992747744,
-0.220827727645449));
#50226=CARTESIAN_POINT('Ctrl Pts',(0.122895853222569,0.051005288895696,
-0.213752098188807));
#50227=CARTESIAN_POINT('Ctrl Pts',(0.0250586586717446,0.130678972531276,
-0.206676468732165));
#50228=CARTESIAN_POINT('Ctrl Pts',(-0.0953109126809523,0.0928480487521756,
-0.199600839275523));
#50229=CARTESIAN_POINT('Ctrl Pts',(-0.129978315135717,-0.0284704729196375,
-0.192525209818881));
#50230=CARTESIAN_POINT('Ctrl Pts',(-0.0477711310054264,-0.124188764733792,
-0.185449580362238));
#50231=CARTESIAN_POINT('Ctrl Pts',(0.0773911505308316,-0.108238348288846,
-0.178373950905597));
#50232=CARTESIAN_POINT('Ctrl Pts',(0.132964449359835,0.0050383965169822,
-0.171298321448954));
#50233=CARTESIAN_POINT('Ctrl Pts',(0.0689780736978123,0.113784689826127,
-0.164222691992312));
#50234=CARTESIAN_POINT('Ctrl Pts',(-0.0570323699065417,0.120217465077596,
-0.15714706253567));
#50235=CARTESIAN_POINT('Ctrl Pts',(-0.131760146461308,0.018552467952097,
-0.150071433079028));
#50236=CARTESIAN_POINT('Ctrl Pts',(-0.0880111400026247,-0.0997946381442195,
-0.142995803622385));
#50237=CARTESIAN_POINT('Ctrl Pts',(0.0348761873840781,-0.12840786967506,
-0.135920174165744));
#50238=CARTESIAN_POINT('Ctrl Pts',(0.126403360542409,-0.0415586470065835,
-0.128844544709101));
#50239=CARTESIAN_POINT('Ctrl Pts',(0.104270494022426,0.0826595197684713,
-0.121768915252459));
#50240=CARTESIAN_POINT('Ctrl Pts',(-0.0116208657192668,0.132551424285361,
-0.114693285795817));
#50241=CARTESIAN_POINT('Ctrl Pts',(-0.117062912752348,0.0632551154486533,
-0.107617656339175));
#50242=CARTESIAN_POINT('Ctrl Pts',(-0.117243715478986,-0.062919404148945,
-0.100542026882533));
#50243=CARTESIAN_POINT('Ctrl Pts',(-0.0120006909773092,-0.132517451403649,
-0.0934663974258908));
#50244=CARTESIAN_POINT('Ctrl Pts',(0.104033168428031,-0.0829582725370532,
-0.0863907679692488));
#50245=CARTESIAN_POINT('Ctrl Pts',(0.126521953402081,0.0411967401319214,
-0.0793151385126065));
#50246=CARTESIAN_POINT('Ctrl Pts',(0.0352440264674689,0.128306395271426,
-0.0722395090559646));
#50247=CARTESIAN_POINT('Ctrl Pts',(-0.087724743715985,0.100048353783583,
-0.0651638795993223));
#50248=CARTESIAN_POINT('Ctrl Pts',(-0.131812842255007,-0.018178387413442,
-0.0580882501426802));
#50249=CARTESIAN_POINT('Ctrl Pts',(-0.0573765353529852,-0.120046677162891,
-0.0510126206860381));
#50250=CARTESIAN_POINT('Ctrl Pts',(0.0686514524583478,-0.113994911636185,
-0.0439369912293959));
#50251=CARTESIAN_POINT('Ctrl Pts',(0.132949933158501,-0.0053947116802003,
-0.0368613617727538));
#50252=CARTESIAN_POINT('Ctrl Pts',(0.0777001067021897,0.107968975917745,
-0.0297857323161117));
#50253=CARTESIAN_POINT('Ctrl Pts',(-0.0474129944147971,0.124416184096178,
-0.0227101028594696));
#50254=CARTESIAN_POINT('Ctrl Pts',(-0.129902332666679,0.0286572707534853,
-0.0156344734028275));
#50255=CARTESIAN_POINT('Ctrl Pts',(-0.107002497886112,-0.0518616552656198,
-0.0109173870983993));
#50256=CARTESIAN_POINT('Ctrl Pts',(-0.0811257482669688,-0.0785775606491374,
-0.0085588439461853));
#50257=CARTESIAN_POINT('Ctrl Pts',(-0.103903098846544,-0.01000131630652,
-0.548441156053815));
#50258=CARTESIAN_POINT('Ctrl Pts',(-0.100609517882874,-0.0442181391665536,
-0.546082612901601));
#50259=CARTESIAN_POINT('Ctrl Pts',(-0.0576728882502106,-0.108579194844902,
-0.541365526597172));
#50260=CARTESIAN_POINT('Ctrl Pts',(0.059137185108432,-0.107913502999689,
-0.534289897140531));
#50261=CARTESIAN_POINT('Ctrl Pts',(0.122532133166971,-0.0100206374046807,
-0.527214267683888));
#50262=CARTESIAN_POINT('Ctrl Pts',(0.0758680568520174,0.096784665802878,
-0.520138638227247));
#50263=CARTESIAN_POINT('Ctrl Pts',(-0.0390779391316531,0.11661378209274,
-0.513063008770604));
#50264=CARTESIAN_POINT('Ctrl Pts',(-0.118852817457893,0.0315586169297806,
-0.505987379313962));
#50265=CARTESIAN_POINT('Ctrl Pts',(-0.0917742578488372,-0.0818594416492388,
-0.49891174985732));
#50266=CARTESIAN_POINT('Ctrl Pts',(0.017835451829119,-0.121678145539317,
-0.491836120400678));
#50267=CARTESIAN_POINT('Ctrl Pts',(0.111403000489139,-0.0520817308529327,
-0.484760490944035));
#50268=CARTESIAN_POINT('Ctrl Pts',(0.104801131493274,0.0643437440163113,
-0.477684861487394));
#50269=CARTESIAN_POINT('Ctrl Pts',(0.00396230201918651,0.122913359267676,
-0.470609232030751));
#50270=CARTESIAN_POINT('Ctrl Pts',(-0.100438672594758,0.0709605197038912,
-0.46353360257411));
#50271=CARTESIAN_POINT('Ctrl Pts',(-0.114527039880617,-0.0447986726116728,
-0.456457973117467));
#50272=CARTESIAN_POINT('Ctrl Pts',(-0.0256341860842926,-0.12027571703659,
-0.449382343660825));
#50273=CARTESIAN_POINT('Ctrl Pts',(0.086308448336185,-0.0876025246205361,
-0.442306714204183));
#50274=CARTESIAN_POINT('Ctrl Pts',(0.120643850883909,0.0238415236856122,
-0.435231084747541));
#50275=CARTESIAN_POINT('Ctrl Pts',(0.0464980513555134,0.113847648207894,
-0.428155455290898));
#50276=CARTESIAN_POINT('Ctrl Pts',(-0.0694580962251789,0.101483632068514,
-0.421079825834256));
#50277=CARTESIAN_POINT('Ctrl Pts',(-0.1229585545277,-0.00213296490494009,
-0.414004196377614));
#50278=CARTESIAN_POINT('Ctrl Pts',(-0.0658964874670156,-0.103831634632347,
-0.406928566920973));
#50279=CARTESIAN_POINT('Ctrl Pts',(0.0504187283965367,-0.112166426000879,
-0.39985293746433));
#50280=CARTESIAN_POINT('Ctrl Pts',(0.121398167421037,-0.0196428200883453,
-0.392777308007688));
#50281=CARTESIAN_POINT('Ctrl Pts',(0.0832181617096029,0.090543320832145,
-0.385701678551046));
#50282=CARTESIAN_POINT('Ctrl Pts',(-0.0297903890165711,0.11931424096654,
-0.378626049094403));
#50283=CARTESIAN_POINT('Ctrl Pts',(-0.116011860873284,0.0407995530787335,
-0.371550419637762));
#50284=CARTESIAN_POINT('Ctrl Pts',(-0.097917176023896,-0.0744014920938668,
-0.364474790181119));
#50285=CARTESIAN_POINT('Ctrl Pts',(0.00822319128817242,-0.122701811359053,
-0.357399160724477));
#50286=CARTESIAN_POINT('Ctrl Pts',(0.106969386133436,-0.0606704690820297,
-0.350323531267835));
#50287=CARTESIAN_POINT('Ctrl Pts',(0.109530284451767,0.0559148654199285,
-0.343247901811193));
#50288=CARTESIAN_POINT('Ctrl Pts',(0.0136031642130584,0.12222237647205,
-0.336172272354551));
#50289=CARTESIAN_POINT('Ctrl Pts',(-0.0945557209355774,0.0786293267539514,
-0.329096642897909));
#50290=CARTESIAN_POINT('Ctrl Pts',(-0.11769149447966,-0.0356660554919151,
-0.322021013441267));
#50291=CARTESIAN_POINT('Ctrl Pts',(-0.0350008096061194,-0.117891045945634,
-0.314945383984624));
#50292=CARTESIAN_POINT('Ctrl Pts',(0.0791620877568367,-0.0941101442420569,
-0.307869754527982));
#50293=CARTESIAN_POINT('Ctrl Pts',(0.122143601746255,0.0142932130642829,
-0.30079412507134));
#50294=CARTESIAN_POINT('Ctrl Pts',(0.0552953880358837,0.109844323700485,
-0.293718495614698));
#50295=CARTESIAN_POINT('Ctrl Pts',(-0.0612736241790938,0.106625036305835,
-0.286642866158056));
#50296=CARTESIAN_POINT('Ctrl Pts',(-0.122746295999892,0.00753008669026765,
-0.279567236701414));
#50297=CARTESIAN_POINT('Ctrl Pts',(-0.0738473063246818,-0.0983358059703825,
-0.272491607244772));
#50298=CARTESIAN_POINT('Ctrl Pts',(0.0414540935386933,-0.115779590240019,
-0.26541597778813));
#50299=CARTESIAN_POINT('Ctrl Pts',(0.119480583048096,-0.0291160722238209,
-0.258340348331487));
#50300=CARTESIAN_POINT('Ctrl Pts',(0.0900718920487197,0.083728189100281,
-0.251264718874845));
#50301=CARTESIAN_POINT('Ctrl Pts',(-0.0203281176582841,0.121285295975039,
-0.244189089418203));
#50302=CARTESIAN_POINT('Ctrl Pts',(-0.112449383369356,0.0497844510574437,
-0.237113459961561));
#50303=CARTESIAN_POINT('Ctrl Pts',(-0.103457819763834,-0.0664818390007551,
-0.230037830504919));
#50304=CARTESIAN_POINT('Ctrl Pts',(-0.001438508403721,-0.122968638607569,
-0.222962201048277));
#50305=CARTESIAN_POINT('Ctrl Pts',(0.101874288526012,-0.0688838495178792,
-0.215886571591635));
#50306=CARTESIAN_POINT('Ctrl Pts',(0.113583225667077,0.0471402824988931,
-0.208810942134992));
#50307=CARTESIAN_POINT('Ctrl Pts',(0.0231597991973928,0.120776566806372,
-0.20173531267835));
#50308=CARTESIAN_POINT('Ctrl Pts',(-0.0880885776021261,0.0858123410809228,
-0.194659683221708));
#50309=CARTESIAN_POINT('Ctrl Pts',(-0.120129002832582,-0.0263130778271519,
-0.187584053765066));
#50310=CARTESIAN_POINT('Ctrl Pts',(-0.0441511980354138,-0.114778164764663,
-0.180508424308424));
#50311=CARTESIAN_POINT('Ctrl Pts',(0.0715267137570432,-0.100036416340742,
-0.173432794851782));
#50312=CARTESIAN_POINT('Ctrl Pts',(0.122888858015295,0.00465660405605617,
-0.16635716539514));
#50313=CARTESIAN_POINT('Ctrl Pts',(0.0637511511206958,0.105162475080209,
-0.159281535938498));
#50314=CARTESIAN_POINT('Ctrl Pts',(-0.0527106519183466,0.111107796617868,
-0.152205906481856));
#50315=CARTESIAN_POINT('Ctrl Pts',(-0.121775813072703,0.0171466253647131,
-0.145130277025213));
#50316=CARTESIAN_POINT('Ctrl Pts',(-0.0813419567382034,-0.0922325416804027,
-0.138054647568571));
#50317=CARTESIAN_POINT('Ctrl Pts',(0.0322333891516986,-0.118677560359315,
-0.130979018111929));
#50318=CARTESIAN_POINT('Ctrl Pts',(0.116824946074981,-0.0384094748324691,
-0.123903388655287));
#50319=CARTESIAN_POINT('Ctrl Pts',(0.0963692325038669,0.0763958639873,-0.116827759198645));
#50320=CARTESIAN_POINT('Ctrl Pts',(-0.0107402762487675,0.122507130568762,
-0.109752129742003));
#50321=CARTESIAN_POINT('Ctrl Pts',(-0.10819228548188,0.0584618590798953,
-0.10267650028536));
#50322=CARTESIAN_POINT('Ctrl Pts',(-0.108359387596088,-0.0581515868346264,
-0.0956008708287185));
#50323=CARTESIAN_POINT('Ctrl Pts',(-0.0110913196474408,-0.122475732035867,
-0.0885252413720763));
#50324=CARTESIAN_POINT('Ctrl Pts',(0.0961498906315588,-0.0766719782925641,
-0.0814496119154342));
#50325=CARTESIAN_POINT('Ctrl Pts',(0.116934552373236,0.0380749920233496,
-0.0743739824587921));
#50326=CARTESIAN_POINT('Ctrl Pts',(0.0325733546470527,0.118583775339031,
-0.06729835300215));
#50327=CARTESIAN_POINT('Ctrl Pts',(-0.0810772625829288,0.092467031616111,
-0.0602227235455078));
#50328=CARTESIAN_POINT('Ctrl Pts',(-0.121824515759332,-0.0168008913702342,
-0.0531470940888656));
#50329=CARTESIAN_POINT('Ctrl Pts',(-0.053028737684017,-0.110949950427387,
-0.0460714646322235));
#50330=CARTESIAN_POINT('Ctrl Pts',(0.0634492801219856,-0.105356767000284,
-0.0389958351755814));
#50331=CARTESIAN_POINT('Ctrl Pts',(0.122875441802065,-0.00498591887450599,
-0.0319202057189393));
#50332=CARTESIAN_POINT('Ctrl Pts',(0.0718122582861078,0.099787456086894,
-0.0248445762622972));
#50333=CARTESIAN_POINT('Ctrl Pts',(-0.043820199811094,0.114988351065352,
-0.017768946805655));
#50334=CARTESIAN_POINT('Ctrl Pts',(-0.120058778055251,0.0264857207598426,
-0.010693317349013));
#50335=CARTESIAN_POINT('Ctrl Pts',(-0.0988942144559457,-0.0479317563533654,
-0.00597623104458479));
#50336=CARTESIAN_POINT('Ctrl Pts',(-0.0749783164459562,-0.0726232217731204,
-0.00361768789237075));
#50337=CARTESIAN_POINT('Ctrl Pts',(-0.0953841396803776,-0.00918131376406524,
-0.5435));
#50338=CARTESIAN_POINT('Ctrl Pts',(-0.0923605976477055,-0.0405927177292199,
-0.541141456847786));
#50339=CARTESIAN_POINT('Ctrl Pts',(-0.0529443191752485,-0.0996768450839476,
-0.536424370543358));
#50340=CARTESIAN_POINT('Ctrl Pts',(0.0542885591219757,-0.0990657329549278,
-0.529348741086716));
#50341=CARTESIAN_POINT('Ctrl Pts',(0.112485789500799,-0.00919905073578263,
-0.522273111630074));
#50342=CARTESIAN_POINT('Ctrl Pts',(0.0696476756938639,0.0888493431316701,
-0.515197482173432));
#50343=CARTESIAN_POINT('Ctrl Pts',(-0.0358739599293379,0.107052680846593,
-0.508121852716789));
#50344=CARTESIAN_POINT('Ctrl Pts',(-0.109108138906939,0.0289711429087928,
-0.501046223260148));
#50345=CARTESIAN_POINT('Ctrl Pts',(-0.0842497358297758,-0.0751478300754116,
-0.493970593803505));
#50346=CARTESIAN_POINT('Ctrl Pts',(0.0163731327305643,-0.111701819859221,
-0.486894964346863));
#50347=CARTESIAN_POINT('Ctrl Pts',(0.10226912842285,-0.0478115777644791,
-0.479819334890221));
#50348=CARTESIAN_POINT('Ctrl Pts',(0.0962085431136162,0.0590682350665474,
-0.472743705433579));
#50349=CARTESIAN_POINT('Ctrl Pts',(0.00363743500867127,0.112835759078637,
-0.465668075976936));
#50350=CARTESIAN_POINT('Ctrl Pts',(-0.0922037598728345,0.0651425048758612,
-0.458592446520295));
#50351=CARTESIAN_POINT('Ctrl Pts',(-0.105137029505605,-0.0411256535495477,
-0.451516817063652));
#50352=CARTESIAN_POINT('Ctrl Pts',(-0.0235324529605039,-0.110414375714813,
-0.44444118760701));
#50353=CARTESIAN_POINT('Ctrl Pts',(0.07923206509802,-0.0804200407641335,
-0.437365558150368));
#50354=CARTESIAN_POINT('Ctrl Pts',(0.110752326466076,0.0218867699872954,
-0.430289928693726));
#50355=CARTESIAN_POINT('Ctrl Pts',(0.0426857011445824,0.104513340790562,
-0.423214299237084));
#50356=CARTESIAN_POINT('Ctrl Pts',(-0.0637632642897446,0.0931630436816094,
-0.416138669780442));
#50357=CARTESIAN_POINT('Ctrl Pts',(-0.11287724880361,-0.00195808426009219,
-0.409063040323799));
#50358=CARTESIAN_POINT('Ctrl Pts',(-0.0604936699172284,-0.0953185347786495,
-0.401987410867158));
#50359=CARTESIAN_POINT('Ctrl Pts',(0.0462849239846546,-0.102969961087666,
-0.394911781410515));
#50360=CARTESIAN_POINT('Ctrl Pts',(0.111444796996209,-0.0180323158387254,
-0.387836151953873));
#50361=CARTESIAN_POINT('Ctrl Pts',(0.0763951494091263,0.0831197226767399,
-0.380760522497231));
#50362=CARTESIAN_POINT('Ctrl Pts',(-0.0273478910507391,0.109531730550394,
-0.373684893040589));
#50363=CARTESIAN_POINT('Ctrl Pts',(-0.106500110824037,0.0374544196752633,
-0.366609263583947));
#50364=CARTESIAN_POINT('Ctrl Pts',(-0.0898889994490478,-0.0683013537911051,
-0.359533634127305));
#50365=CARTESIAN_POINT('Ctrl Pts',(0.00754897625919715,-0.112641555869212,
-0.352458004670662));
#50366=CARTESIAN_POINT('Ctrl Pts',(0.0981990237225277,-0.0556961299676074,
-0.345382375214021));
#50367=CARTESIAN_POINT('Ctrl Pts',(0.100549955365708,0.0513304356908642,
-0.338306745757378));
#50368=CARTESIAN_POINT('Ctrl Pts',(0.0124878480988304,0.11220142959062,
-0.331231116300736));
#50369=CARTESIAN_POINT('Ctrl Pts',(-0.0868031482546871,0.0721825505623247,
-0.324155486844094));
#50370=CARTESIAN_POINT('Ctrl Pts',(-0.108042032174805,-0.0327418147933531,
-0.317079857387452));
#50371=CARTESIAN_POINT('Ctrl Pts',(-0.0321311120597763,-0.108225222523459,
-0.31000422793081));
#50372=CARTESIAN_POINT('Ctrl Pts',(0.0726716307772531,-0.0863941041545113,
-0.302928598474167));
#50373=CARTESIAN_POINT('Ctrl Pts',(0.112129113562205,0.0131213202160467,
-0.295852969017526));
#50374=CARTESIAN_POINT('Ctrl Pts',(0.050761748924207,0.100838246705403,
-0.288777339560883));
#50375=CARTESIAN_POINT('Ctrl Pts',(-0.0562498327028107,0.0978829069520032,
-0.281701710104242));
#50376=CARTESIAN_POINT('Ctrl Pts',(-0.112682393238285,0.0069126989343267,
-0.274626080647599));
#50377=CARTESIAN_POINT('Ctrl Pts',(-0.0677926054149375,-0.0902733061514795,
-0.267550451190957));
#50378=CARTESIAN_POINT('Ctrl Pts',(0.038055294715108,-0.106286883935013,
-0.260474821734315));
#50379=CARTESIAN_POINT('Ctrl Pts',(0.10968443433419,-0.0267288611289883,
-0.253399192277673));
#50380=CARTESIAN_POINT('Ctrl Pts',(0.0826869460855996,0.0768633599284799,
-0.246323562821031));
#50381=CARTESIAN_POINT('Ctrl Pts',(-0.0186614262296518,0.111341179819334,
-0.239247933364389));
#50382=CARTESIAN_POINT('Ctrl Pts',(-0.103229718933756,0.0457026507033001,
-0.232172303907746));
#50383=CARTESIAN_POINT('Ctrl Pts',(-0.094975368790062,-0.0610310287936844,
-0.225096674451104));
#50384=CARTESIAN_POINT('Ctrl Pts',(-0.00132056587373289,-0.112886506095197,
-0.218021044994462));
#50385=CARTESIAN_POINT('Ctrl Pts',(0.0935216704263627,-0.0632360997609839,
-0.21094541553782));
#50386=CARTESIAN_POINT('Ctrl Pts',(0.104270598111585,0.04327527610209,-0.203869786081178));
#50387=CARTESIAN_POINT('Ctrl Pts',(0.0212609397230408,0.110874161081468,
-0.196794156624536));
#50388=CARTESIAN_POINT('Ctrl Pts',(-0.0808662425232999,0.0787766334096698,
-0.189718527167894));
#50389=CARTESIAN_POINT('Ctrl Pts',(-0.110279690529448,-0.0241556827346662,
-0.182642897711252));
#50390=CARTESIAN_POINT('Ctrl Pts',(-0.040531265065401,-0.105367564795535,
-0.17556726825461));
#50391=CARTESIAN_POINT('Ctrl Pts',(0.0656622769832545,-0.0918344843926382,
-0.168491638797967));
#50392=CARTESIAN_POINT('Ctrl Pts',(0.112813266670755,0.00427481159513008,
-0.161416009341325));
#50393=CARTESIAN_POINT('Ctrl Pts',(0.0585242285435791,0.0965402603342907,
-0.154340379884683));
#50394=CARTESIAN_POINT('Ctrl Pts',(-0.0483889339301513,0.10199812815814,
-0.147264750428041));
#50395=CARTESIAN_POINT('Ctrl Pts',(-0.111791479684098,0.0157407827773292,
-0.140189120971399));
#50396=CARTESIAN_POINT('Ctrl Pts',(-0.0746727734737821,-0.0846704452165861,
-0.133113491514757));
#50397=CARTESIAN_POINT('Ctrl Pts',(0.0295905909193192,-0.108947251043571,
-0.126037862058114));
#50398=CARTESIAN_POINT('Ctrl Pts',(0.107246531607553,-0.0352603026583548,
-0.118962232601472));
#50399=CARTESIAN_POINT('Ctrl Pts',(0.0884679709853073,0.0701322082061288,
-0.11188660314483));
#50400=CARTESIAN_POINT('Ctrl Pts',(-0.00985968677826821,0.112462836852163,
-0.104810973688188));
#50401=CARTESIAN_POINT('Ctrl Pts',(-0.0993216582114113,0.0536686027111373,
-0.097735344231546));
#50402=CARTESIAN_POINT('Ctrl Pts',(-0.0994750597131893,-0.053383769520308,
-0.0906597147749039));
#50403=CARTESIAN_POINT('Ctrl Pts',(-0.0101819483175724,-0.112434012668085,
-0.0835840853182618));
#50404=CARTESIAN_POINT('Ctrl Pts',(0.0882666128350871,-0.0703856840480749,
-0.0765084558616196));
#50405=CARTESIAN_POINT('Ctrl Pts',(0.107347151344391,0.0349532439147777,
-0.0694328264049776));
#50406=CARTESIAN_POINT('Ctrl Pts',(0.0299026828266366,0.108861155406636,
-0.0623571969483354));
#50407=CARTESIAN_POINT('Ctrl Pts',(-0.0744297814498727,0.0848857094486392,
-0.0552815674916933));
#50408=CARTESIAN_POINT('Ctrl Pts',(-0.111836189263656,-0.0154233953270265,
-0.048205938035051));
#50409=CARTESIAN_POINT('Ctrl Pts',(-0.0486809400150489,-0.101853223691883,
-0.041130308578409));
#50410=CARTESIAN_POINT('Ctrl Pts',(0.0582471077856237,-0.0967186223643828,
-0.0340546791217668));
#50411=CARTESIAN_POINT('Ctrl Pts',(0.112800950445628,-0.0045771260688116,
-0.0269790496651248));
#50412=CARTESIAN_POINT('Ctrl Pts',(0.0659244098700261,0.0916059362560433,
-0.0199034202084826));
#50413=CARTESIAN_POINT('Ctrl Pts',(-0.040227405207391,0.105560518034527,
-0.0128277907518405));
#50414=CARTESIAN_POINT('Ctrl Pts',(-0.110215223443824,0.0243141707662,-0.00575216129519839));
#50415=CARTESIAN_POINT('Ctrl Pts',(-0.0907859310257796,-0.044001857441111,
-0.00103507499077024));
#50416=CARTESIAN_POINT('Ctrl Pts',(-0.0688308846249437,-0.0666688828971034,
0.0013234681614438));
#50417=CARTESIAN_POINT('Ctrl Pts',(-0.0872731800879813,-0.0845318995251544,
-0.0134999999999998));
#50418=CARTESIAN_POINT('Ctrl Pts',(-0.108954027555681,-0.0621479649852055,
-0.0153369116616685));
#50419=CARTESIAN_POINT('Ctrl Pts',(-0.121220706757624,-0.0309262392804433,
-0.0171738233233372));
#50420=CARTESIAN_POINT('Ctrl Pts',(-0.121508540285962,0.000130861710946541,
-0.0190107349850059));
#50421=CARTESIAN_POINT('Origin',(0.,0.,-0.29));
#50422=CARTESIAN_POINT('Origin',(0.,0.,-0.0135));
#50423=CARTESIAN_POINT('Origin',(0.228475398698832,-0.0402863772187279,
0.04));
#50424=CARTESIAN_POINT('',(0.221856282657939,-0.0374805262129628,0.04));
#50425=CARTESIAN_POINT('',(0.221295806635937,-0.0406591436868745,0.04));
#50426=CARTESIAN_POINT('Origin',(0.,0.,0.04));
#50427=CARTESIAN_POINT('',(0.215672897909674,-0.0380289509090578,0.04));
#50428=CARTESIAN_POINT('',(0.24249343673166,-0.0356501492573125,0.04));
#50429=CARTESIAN_POINT('',(0.215672897909674,-0.0380289509090578,0.04));
#50430=CARTESIAN_POINT('Origin',(0.215672897909674,-0.0380289509090578,
0.04));
#50431=CARTESIAN_POINT('',(0.221295806635937,-0.0406591436868745,0.235));
#50432=CARTESIAN_POINT('',(0.221295806635937,-0.0406591436868745,0.1175));
#50433=CARTESIAN_POINT('',(0.215672897909674,-0.0380289509090578,0.241));
#50434=CARTESIAN_POINT('',(0.215672897909674,-0.0380289509090578,0.04));
#50435=CARTESIAN_POINT('Ctrl Pts',(0.221295806635937,-0.0406591436868745,
0.235));
#50436=CARTESIAN_POINT('Ctrl Pts',(0.218446359646244,-0.0393262757251279,
0.23804339528899));
#50437=CARTESIAN_POINT('Ctrl Pts',(0.215672897909674,-0.0380289509090578,
0.241));
#50438=CARTESIAN_POINT('Origin',(0.24249343673166,-0.0356501492573125,0.04));
#50439=CARTESIAN_POINT('',(0.221856282657939,-0.0374805262129628,0.235));
#50440=CARTESIAN_POINT('',(0.221856282657939,-0.0374805262129628,0.1175));
#50441=CARTESIAN_POINT('Ctrl Pts',(0.215672897909674,-0.0380289509090578,
0.241));
#50442=CARTESIAN_POINT('Ctrl Pts',(0.218722810657151,-0.0377584441332792,
0.238043395288934));
#50443=CARTESIAN_POINT('Ctrl Pts',(0.221856282657939,-0.0374805262129628,
0.235));
#50444=CARTESIAN_POINT('Origin',(0.218008688022331,-0.0793486732515553,
0.04));
#50445=CARTESIAN_POINT('',(0.211977362141128,-0.0754360519890137,0.04));
#50446=CARTESIAN_POINT('',(0.210873439877438,-0.0784690534813354,0.04));
#50447=CARTESIAN_POINT('Origin',(0.,0.,0.04));
#50448=CARTESIAN_POINT('',(0.205792683952114,-0.0749024113883216,0.04));
#50449=CARTESIAN_POINT('',(0.232618833095827,-0.0772170867692877,0.04));
#50450=CARTESIAN_POINT('',(0.205792683952114,-0.0749024113883216,0.04));
#50451=CARTESIAN_POINT('Origin',(0.205792683952114,-0.0749024113883216,
0.04));
#50452=CARTESIAN_POINT('',(0.210873439877438,-0.0784690534813354,0.235));
#50453=CARTESIAN_POINT('',(0.210873439877438,-0.0784690534813354,0.1175));
#50454=CARTESIAN_POINT('',(0.205792683952114,-0.0749024113883216,0.241));
#50455=CARTESIAN_POINT('',(0.205792683952114,-0.0749024113883216,0.04));
#50456=CARTESIAN_POINT('Ctrl Pts',(0.210873439877438,-0.0784690534813354,
0.235));
#50457=CARTESIAN_POINT('Ctrl Pts',(0.208298732482818,-0.0766616335017468,
0.23804339528899));
#50458=CARTESIAN_POINT('Ctrl Pts',(0.205792683952114,-0.0749024113883216,
0.241));
#50459=CARTESIAN_POINT('Origin',(0.232618833095827,-0.0772170867692877,
0.04));
#50460=CARTESIAN_POINT('',(0.211977362141128,-0.0754360519890138,0.235));
#50461=CARTESIAN_POINT('',(0.211977362141128,-0.0754360519890138,0.1175));
#50462=CARTESIAN_POINT('Ctrl Pts',(0.205792683952114,-0.0749024113883216,
0.241));
#50463=CARTESIAN_POINT('Ctrl Pts',(0.20884323468045,-0.0751656260089308,
0.238043395288983));
#50464=CARTESIAN_POINT('Ctrl Pts',(0.211977362141128,-0.0754360519890137,
0.235));
#50465=CARTESIAN_POINT('Origin',(0.20091789367799,-0.116,0.04));
#50466=CARTESIAN_POINT('',(0.195657616741379,-0.111099491497862,0.04));
#50467=CARTESIAN_POINT('',(0.194043790355372,-0.113894720793023,0.04));
#50468=CARTESIAN_POINT('Origin',(0.,0.,0.04));
#50469=CARTESIAN_POINT('',(0.189659563428792,-0.1095,0.04));
#50470=CARTESIAN_POINT('',(0.215676223927187,-0.116437822173509,0.04));
#50471=CARTESIAN_POINT('',(0.189659563428792,-0.1095,0.04));
#50472=CARTESIAN_POINT('Origin',(0.189659563428792,-0.1095,0.04));
#50473=CARTESIAN_POINT('',(0.194043790355372,-0.113894720793023,0.235));
#50474=CARTESIAN_POINT('',(0.194043790355372,-0.113894720793023,0.1175));
#50475=CARTESIAN_POINT('',(0.189659563428792,-0.1095,0.241));
#50476=CARTESIAN_POINT('',(0.189659563428792,-0.1095,0.04));
#50477=CARTESIAN_POINT('Ctrl Pts',(0.194043790355372,-0.113894720793023,
0.235));
#50478=CARTESIAN_POINT('Ctrl Pts',(0.191822053737127,-0.111667666337054,
0.238043395289017));
#50479=CARTESIAN_POINT('Ctrl Pts',(0.189659563428792,-0.1095,0.241));
#50480=CARTESIAN_POINT('Origin',(0.215676223927187,-0.116437822173509,0.04));
#50481=CARTESIAN_POINT('',(0.195657616741379,-0.111099491497862,0.235));
#50482=CARTESIAN_POINT('',(0.195657616741379,-0.111099491497862,0.1175));
#50483=CARTESIAN_POINT('Ctrl Pts',(0.189659563428792,-0.1095,0.241));
#50484=CARTESIAN_POINT('Ctrl Pts',(0.192618062697872,-0.110288938373955,
0.238043395288922));
#50485=CARTESIAN_POINT('Ctrl Pts',(0.195657616741379,-0.111099491497863,
0.235));
#50486=CARTESIAN_POINT('Origin',(0.177722310803603,-0.149126725447277,0.04));
#50487=CARTESIAN_POINT('',(0.173392913664475,-0.143387229176604,0.04));
#50488=CARTESIAN_POINT('',(0.171318218454253,-0.145859754646924,0.04));
#50489=CARTESIAN_POINT('Origin',(0.,0.,0.04));
#50490=CARTESIAN_POINT('',(0.167763733043056,-0.140770486521352,0.04));
#50491=CARTESIAN_POINT('',(0.192180401831955,-0.152120653271369,0.04));
#50492=CARTESIAN_POINT('',(0.167763733043056,-0.140770486521352,0.04));
#50493=CARTESIAN_POINT('Origin',(0.167763733043056,-0.140770486521352,0.04));
#50494=CARTESIAN_POINT('',(0.171318218454253,-0.145859754646924,0.235));
#50495=CARTESIAN_POINT('',(0.171318218454253,-0.145859754646924,0.1175));
#50496=CARTESIAN_POINT('',(0.167763733043056,-0.140770486521352,0.241));
#50497=CARTESIAN_POINT('',(0.167763733043056,-0.140770486521352,0.04));
#50498=CARTESIAN_POINT('Ctrl Pts',(0.171318218454253,-0.145859754646924,
0.235));
#50499=CARTESIAN_POINT('Ctrl Pts',(0.169516958955325,-0.143280733637328,
0.238043395288973));
#50500=CARTESIAN_POINT('Ctrl Pts',(0.167763733043056,-0.140770486521352,
0.241));
#50501=CARTESIAN_POINT('Origin',(0.192180401831955,-0.152120653271369,0.04));
#50502=CARTESIAN_POINT('',(0.173392913664475,-0.143387229176604,0.235));
#50503=CARTESIAN_POINT('',(0.173392913664475,-0.143387229176604,0.1175));
#50504=CARTESIAN_POINT('Ctrl Pts',(0.167763733043056,-0.140770486521352,
0.241));
#50505=CARTESIAN_POINT('Ctrl Pts',(0.170540288349532,-0.142061177155346,
0.238043395288992));
#50506=CARTESIAN_POINT('Ctrl Pts',(0.173392913664475,-0.143387229176604,
0.235));
#50507=CARTESIAN_POINT('Origin',(0.149126725447277,-0.177722310803603,0.04));
#50508=CARTESIAN_POINT('',(0.145859754646924,-0.171318218454253,0.04));
#50509=CARTESIAN_POINT('',(0.143387229176604,-0.173392913664475,0.04));
#50510=CARTESIAN_POINT('Origin',(0.,0.,0.04));
#50511=CARTESIAN_POINT('',(0.140770486521352,-0.167763733043056,0.04));
#50512=CARTESIAN_POINT('',(0.162845275475035,-0.183181375296344,0.04));
#50513=CARTESIAN_POINT('',(0.140770486521352,-0.167763733043056,0.04));
#50514=CARTESIAN_POINT('Origin',(0.140770486521352,-0.167763733043056,0.04));
#50515=CARTESIAN_POINT('',(0.143387229176604,-0.173392913664475,0.235));
#50516=CARTESIAN_POINT('',(0.143387229176604,-0.173392913664475,0.1175));
#50517=CARTESIAN_POINT('',(0.140770486521352,-0.167763733043056,0.241));
#50518=CARTESIAN_POINT('',(0.140770486521352,-0.167763733043056,0.04));
#50519=CARTESIAN_POINT('Ctrl Pts',(0.143387229176604,-0.173392913664475,
0.235));
#50520=CARTESIAN_POINT('Ctrl Pts',(0.142061177155362,-0.170540288349568,
0.238043395288954));
#50521=CARTESIAN_POINT('Ctrl Pts',(0.140770486521352,-0.167763733043056,
0.241));
#50522=CARTESIAN_POINT('Origin',(0.162845275475035,-0.183181375296344,0.04));
#50523=CARTESIAN_POINT('',(0.145859754646924,-0.171318218454253,0.235));
#50524=CARTESIAN_POINT('',(0.145859754646924,-0.171318218454253,0.1175));
#50525=CARTESIAN_POINT('Ctrl Pts',(0.140770486521352,-0.167763733043056,
0.241));
#50526=CARTESIAN_POINT('Ctrl Pts',(0.143280733637332,-0.169516958955328,
0.238043395288968));
#50527=CARTESIAN_POINT('Ctrl Pts',(0.145859754646923,-0.171318218454253,
0.235));
#50528=CARTESIAN_POINT('Origin',(0.116,-0.20091789367799,0.04));
#50529=CARTESIAN_POINT('',(0.113894720793023,-0.194043790355372,0.04));
#50530=CARTESIAN_POINT('',(0.111099491497862,-0.195657616741379,0.04));
#50531=CARTESIAN_POINT('Origin',(0.,0.,0.04));
#50532=CARTESIAN_POINT('',(0.1095,-0.189659563428792,0.04));
#50533=CARTESIAN_POINT('',(0.128562177826491,-0.208676223927188,0.04));
#50534=CARTESIAN_POINT('',(0.1095,-0.189659563428792,0.04));
#50535=CARTESIAN_POINT('Origin',(0.1095,-0.189659563428792,0.04));
#50536=CARTESIAN_POINT('',(0.111099491497862,-0.195657616741379,0.235));
#50537=CARTESIAN_POINT('',(0.111099491497862,-0.195657616741379,0.1175));
#50538=CARTESIAN_POINT('',(0.1095,-0.189659563428792,0.241));
#50539=CARTESIAN_POINT('',(0.1095,-0.189659563428792,0.04));
#50540=CARTESIAN_POINT('Ctrl Pts',(0.111099491497862,-0.195657616741379,
0.235));
#50541=CARTESIAN_POINT('Ctrl Pts',(0.110288938373936,-0.192618062697803,
0.238043395288991));
#50542=CARTESIAN_POINT('Ctrl Pts',(0.1095,-0.189659563428792,0.241));
#50543=CARTESIAN_POINT('Origin',(0.128562177826491,-0.208676223927188,0.04));
#50544=CARTESIAN_POINT('',(0.113894720793023,-0.194043790355372,0.235));
#50545=CARTESIAN_POINT('',(0.113894720793023,-0.194043790355372,0.1175));
#50546=CARTESIAN_POINT('Ctrl Pts',(0.1095,-0.189659563428792,0.241));
#50547=CARTESIAN_POINT('Ctrl Pts',(0.111667666337076,-0.191822053737149,
0.238043395288987));
#50548=CARTESIAN_POINT('Ctrl Pts',(0.113894720793023,-0.194043790355372,
0.235));
#50549=CARTESIAN_POINT('Origin',(0.079348673251555,-0.218008688022331,0.04));
#50550=CARTESIAN_POINT('',(0.0784690534813351,-0.210873439877438,0.04));
#50551=CARTESIAN_POINT('',(0.0754360519890135,-0.211977362141128,0.04));
#50552=CARTESIAN_POINT('Origin',(0.,0.,0.04));
#50553=CARTESIAN_POINT('',(0.0749024113883213,-0.205792683952114,0.04));
#50554=CARTESIAN_POINT('',(0.0903727834602901,-0.227830551089268,0.04));
#50555=CARTESIAN_POINT('',(0.0749024113883213,-0.205792683952114,0.04));
#50556=CARTESIAN_POINT('Origin',(0.0749024113883213,-0.205792683952114,
0.04));
#50557=CARTESIAN_POINT('',(0.0754360519890135,-0.211977362141128,0.235));
#50558=CARTESIAN_POINT('',(0.0754360519890135,-0.211977362141128,0.1175));
#50559=CARTESIAN_POINT('',(0.0749024113883213,-0.205792683952114,0.241));
#50560=CARTESIAN_POINT('',(0.0749024113883213,-0.205792683952114,0.04));
#50561=CARTESIAN_POINT('Ctrl Pts',(0.0754360519890135,-0.211977362141128,
0.235));
#50562=CARTESIAN_POINT('Ctrl Pts',(0.075165626008936,-0.208843234680514,
0.238043395288922));
#50563=CARTESIAN_POINT('Ctrl Pts',(0.0749024113883213,-0.205792683952114,
0.241));
#50564=CARTESIAN_POINT('Origin',(0.0903727834602901,-0.227830551089268,
0.04));
#50565=CARTESIAN_POINT('',(0.0784690534813351,-0.210873439877438,0.235));
#50566=CARTESIAN_POINT('',(0.0784690534813351,-0.210873439877438,0.1175));
#50567=CARTESIAN_POINT('Ctrl Pts',(0.0749024113883213,-0.205792683952114,
0.241));
#50568=CARTESIAN_POINT('Ctrl Pts',(0.0766616335017888,-0.208298732482879,
0.238043395288919));
#50569=CARTESIAN_POINT('Ctrl Pts',(0.0784690534813351,-0.210873439877438,
0.235));
#50570=CARTESIAN_POINT('Origin',(0.0402863772187278,-0.228475398698832,
0.04));
#50571=CARTESIAN_POINT('',(0.0406591436868744,-0.221295806635937,0.04));
#50572=CARTESIAN_POINT('',(0.0374805262129627,-0.221856282657939,0.04));
#50573=CARTESIAN_POINT('Origin',(0.,0.,0.04));
#50574=CARTESIAN_POINT('',(0.0380289509090577,-0.215672897909674,0.04));
#50575=CARTESIAN_POINT('',(0.0494374577994833,-0.240062362244323,0.04));
#50576=CARTESIAN_POINT('',(0.0380289509090577,-0.215672897909674,0.04));
#50577=CARTESIAN_POINT('Origin',(0.0380289509090577,-0.215672897909674,
0.04));
#50578=CARTESIAN_POINT('',(0.0374805262129627,-0.221856282657939,0.235));
#50579=CARTESIAN_POINT('',(0.0374805262129627,-0.221856282657939,0.1175));
#50580=CARTESIAN_POINT('',(0.0380289509090577,-0.215672897909674,0.241));
#50581=CARTESIAN_POINT('',(0.0380289509090577,-0.215672897909674,0.04));
#50582=CARTESIAN_POINT('Ctrl Pts',(0.0374805262129627,-0.221856282657939,
0.235));
#50583=CARTESIAN_POINT('Ctrl Pts',(0.0377584441332851,-0.218722810657084,
0.238043395288999));
#50584=CARTESIAN_POINT('Ctrl Pts',(0.0380289509090577,-0.215672897909674,
0.241));
#50585=CARTESIAN_POINT('Origin',(0.0494374577994833,-0.240062362244323,
0.04));
#50586=CARTESIAN_POINT('',(0.0406591436868744,-0.221295806635937,0.235));
#50587=CARTESIAN_POINT('',(0.0406591436868744,-0.221295806635937,0.1175));
#50588=CARTESIAN_POINT('Ctrl Pts',(0.0380289509090577,-0.215672897909674,
0.241));
#50589=CARTESIAN_POINT('Ctrl Pts',(0.0393262757251536,-0.218446359646299,
0.238043395288931));
#50590=CARTESIAN_POINT('Ctrl Pts',(0.0406591436868744,-0.221295806635937,
0.235));
#50591=CARTESIAN_POINT('Origin',(-4.16333634234434E-17,-0.232,0.04));
#50592=CARTESIAN_POINT('',(0.00161382638600745,-0.224994212290885,0.04));
#50593=CARTESIAN_POINT('',(-0.00161382638600754,-0.224994212290885,0.04));
#50594=CARTESIAN_POINT('Origin',(0.,0.,0.04));
#50595=CARTESIAN_POINT('',(-4.16333634234434E-17,-0.219,0.04));
#50596=CARTESIAN_POINT('',(0.00699999999999996,-0.245,0.04));
#50597=CARTESIAN_POINT('',(-4.16333634234434E-17,-0.219,0.04));
#50598=CARTESIAN_POINT('Origin',(-4.16333634234434E-17,-0.219,0.04));
#50599=CARTESIAN_POINT('',(-0.00161382638600754,-0.224994212290885,0.235));
#50600=CARTESIAN_POINT('',(-0.00161382638600754,-0.224994212290885,0.1175));
#50601=CARTESIAN_POINT('',(-4.16333634234434E-17,-0.219,0.241));
#50602=CARTESIAN_POINT('',(-4.16333634234434E-17,-0.219,0.04));
#50603=CARTESIAN_POINT('Ctrl Pts',(-0.00161382638600753,-0.224994212290885,
0.235));
#50604=CARTESIAN_POINT('Ctrl Pts',(-0.000796008960679004,-0.221956604711093,
0.238043395288907));
#50605=CARTESIAN_POINT('Ctrl Pts',(-4.16333634234434E-17,-0.219,0.241));
#50606=CARTESIAN_POINT('Origin',(0.00699999999999996,-0.245,0.04));
#50607=CARTESIAN_POINT('',(0.00161382638600745,-0.224994212290885,0.235));
#50608=CARTESIAN_POINT('',(0.00161382638600745,-0.224994212290885,0.1175));
#50609=CARTESIAN_POINT('Ctrl Pts',(-4.16333634234434E-17,-0.219,0.241));
#50610=CARTESIAN_POINT('Ctrl Pts',(0.000796008960667156,-0.22195660471105,
0.23804339528895));
#50611=CARTESIAN_POINT('Ctrl Pts',(0.00161382638600743,-0.224994212290885,
0.235));
#50612=CARTESIAN_POINT('Origin',(-0.0402863772187278,-0.228475398698832,
0.04));
#50613=CARTESIAN_POINT('',(-0.0374805262129628,-0.221856282657939,0.04));
#50614=CARTESIAN_POINT('',(-0.0406591436868745,-0.221295806635937,0.04));
#50615=CARTESIAN_POINT('Origin',(0.,0.,0.04));
#50616=CARTESIAN_POINT('',(-0.0380289509090577,-0.215672897909674,0.04));
#50617=CARTESIAN_POINT('',(-0.0356501492573125,-0.24249343673166,0.04));
#50618=CARTESIAN_POINT('',(-0.0380289509090577,-0.215672897909674,0.04));
#50619=CARTESIAN_POINT('Origin',(-0.0380289509090577,-0.215672897909674,
0.04));
#50620=CARTESIAN_POINT('',(-0.0406591436868745,-0.221295806635937,0.235));
#50621=CARTESIAN_POINT('',(-0.0406591436868745,-0.221295806635937,0.1175));
#50622=CARTESIAN_POINT('',(-0.0380289509090577,-0.215672897909674,0.241));
#50623=CARTESIAN_POINT('',(-0.0380289509090577,-0.215672897909674,0.04));
#50624=CARTESIAN_POINT('Ctrl Pts',(-0.0406591436868745,-0.221295806635937,
0.235));
#50625=CARTESIAN_POINT('Ctrl Pts',(-0.0393262757251577,-0.218446359646308,
0.238043395288922));
#50626=CARTESIAN_POINT('Ctrl Pts',(-0.0380289509090577,-0.215672897909674,
0.241));
#50627=CARTESIAN_POINT('Origin',(-0.0356501492573125,-0.24249343673166,
0.04));
#50628=CARTESIAN_POINT('',(-0.0374805262129628,-0.221856282657939,0.235));
#50629=CARTESIAN_POINT('',(-0.0374805262129628,-0.221856282657939,0.1175));
#50630=CARTESIAN_POINT('Ctrl Pts',(-0.0380289509090577,-0.215672897909674,
0.241));
#50631=CARTESIAN_POINT('Ctrl Pts',(-0.0377584441332853,-0.218722810657082,
0.238043395289));
#50632=CARTESIAN_POINT('Ctrl Pts',(-0.0374805262129628,-0.221856282657939,
0.235));
#50633=CARTESIAN_POINT('Origin',(-0.0793486732515553,-0.218008688022331,
0.04));
#50634=CARTESIAN_POINT('',(-0.0754360519890138,-0.211977362141128,0.04));
#50635=CARTESIAN_POINT('',(-0.0784690534813354,-0.210873439877438,0.04));
#50636=CARTESIAN_POINT('Origin',(0.,0.,0.04));
#50637=CARTESIAN_POINT('',(-0.0749024113883216,-0.205792683952114,0.04));
#50638=CARTESIAN_POINT('',(-0.0772170867692877,-0.232618833095827,0.04));
#50639=CARTESIAN_POINT('',(-0.0749024113883216,-0.205792683952114,0.04));
#50640=CARTESIAN_POINT('Origin',(-0.0749024113883216,-0.205792683952114,
0.04));
#50641=CARTESIAN_POINT('',(-0.0784690534813354,-0.210873439877438,0.235));
#50642=CARTESIAN_POINT('',(-0.0784690534813354,-0.210873439877438,0.1175));
#50643=CARTESIAN_POINT('',(-0.0749024113883216,-0.205792683952114,0.241));
#50644=CARTESIAN_POINT('',(-0.0749024113883216,-0.205792683952114,0.04));
#50645=CARTESIAN_POINT('Ctrl Pts',(-0.0784690534813354,-0.210873439877438,
0.235));
#50646=CARTESIAN_POINT('Ctrl Pts',(-0.0766616335017839,-0.208298732482871,
0.238043395288928));
#50647=CARTESIAN_POINT('Ctrl Pts',(-0.0749024113883216,-0.205792683952114,
0.241));
#50648=CARTESIAN_POINT('Origin',(-0.0772170867692877,-0.232618833095827,
0.04));
#50649=CARTESIAN_POINT('',(-0.0754360519890137,-0.211977362141128,0.235));
#50650=CARTESIAN_POINT('',(-0.0754360519890137,-0.211977362141128,0.1175));
#50651=CARTESIAN_POINT('Ctrl Pts',(-0.0749024113883216,-0.205792683952114,
0.241));
#50652=CARTESIAN_POINT('Ctrl Pts',(-0.0751656260089316,-0.208843234680459,
0.238043395288975));
#50653=CARTESIAN_POINT('Ctrl Pts',(-0.0754360519890138,-0.211977362141128,
0.235));
#50654=CARTESIAN_POINT('Origin',(-0.116,-0.20091789367799,0.04));
#50655=CARTESIAN_POINT('',(-0.111099491497862,-0.195657616741379,0.04));
#50656=CARTESIAN_POINT('',(-0.113894720793023,-0.194043790355372,0.04));
#50657=CARTESIAN_POINT('Origin',(0.,0.,0.04));
#50658=CARTESIAN_POINT('',(-0.1095,-0.189659563428792,0.04));
#50659=CARTESIAN_POINT('',(-0.116437822173509,-0.215676223927187,0.04));
#50660=CARTESIAN_POINT('',(-0.1095,-0.189659563428792,0.04));
#50661=CARTESIAN_POINT('Origin',(-0.1095,-0.189659563428792,0.04));
#50662=CARTESIAN_POINT('',(-0.113894720793023,-0.194043790355372,0.235));
#50663=CARTESIAN_POINT('',(-0.113894720793023,-0.194043790355372,0.1175));
#50664=CARTESIAN_POINT('',(-0.1095,-0.189659563428792,0.241));
#50665=CARTESIAN_POINT('',(-0.1095,-0.189659563428792,0.04));
#50666=CARTESIAN_POINT('Ctrl Pts',(-0.113894720793023,-0.194043790355372,
0.235));
#50667=CARTESIAN_POINT('Ctrl Pts',(-0.111667666337054,-0.191822053737127,
0.238043395289017));
#50668=CARTESIAN_POINT('Ctrl Pts',(-0.1095,-0.189659563428792,0.241));
#50669=CARTESIAN_POINT('Origin',(-0.116437822173509,-0.215676223927187,
0.04));
#50670=CARTESIAN_POINT('',(-0.111099491497862,-0.195657616741379,0.235));
#50671=CARTESIAN_POINT('',(-0.111099491497862,-0.195657616741379,0.1175));
#50672=CARTESIAN_POINT('Ctrl Pts',(-0.1095,-0.189659563428792,0.241));
#50673=CARTESIAN_POINT('Ctrl Pts',(-0.110288938373955,-0.192618062697872,
0.238043395288922));
#50674=CARTESIAN_POINT('Ctrl Pts',(-0.111099491497863,-0.195657616741379,
0.235));
#50675=CARTESIAN_POINT('Origin',(-0.149126725447277,-0.177722310803603,
0.04));
#50676=CARTESIAN_POINT('',(-0.143387229176604,-0.173392913664475,0.04));
#50677=CARTESIAN_POINT('',(-0.145859754646924,-0.171318218454253,0.04));
#50678=CARTESIAN_POINT('Origin',(0.,0.,0.04));
#50679=CARTESIAN_POINT('',(-0.140770486521352,-0.167763733043056,0.04));
#50680=CARTESIAN_POINT('',(-0.152120653271369,-0.192180401831955,0.04));
#50681=CARTESIAN_POINT('',(-0.140770486521352,-0.167763733043056,0.04));
#50682=CARTESIAN_POINT('Origin',(-0.140770486521352,-0.167763733043056,
0.04));
#50683=CARTESIAN_POINT('',(-0.145859754646924,-0.171318218454253,0.235));
#50684=CARTESIAN_POINT('',(-0.145859754646924,-0.171318218454253,0.1175));
#50685=CARTESIAN_POINT('',(-0.140770486521352,-0.167763733043056,0.241));
#50686=CARTESIAN_POINT('',(-0.140770486521352,-0.167763733043056,0.04));
#50687=CARTESIAN_POINT('Ctrl Pts',(-0.145859754646924,-0.171318218454253,
0.235));
#50688=CARTESIAN_POINT('Ctrl Pts',(-0.143280733637303,-0.169516958955308,
0.238043395289003));
#50689=CARTESIAN_POINT('Ctrl Pts',(-0.140770486521352,-0.167763733043056,
0.241));
#50690=CARTESIAN_POINT('Origin',(-0.152120653271369,-0.192180401831955,
0.04));
#50691=CARTESIAN_POINT('',(-0.143387229176604,-0.173392913664475,0.235));
#50692=CARTESIAN_POINT('',(-0.143387229176604,-0.173392913664475,0.1175));
#50693=CARTESIAN_POINT('Ctrl Pts',(-0.140770486521352,-0.167763733043056,
0.241));
#50694=CARTESIAN_POINT('Ctrl Pts',(-0.142061177155329,-0.170540288349497,
0.238043395289029));
#50695=CARTESIAN_POINT('Ctrl Pts',(-0.143387229176604,-0.173392913664475,
0.235));
#50696=CARTESIAN_POINT('Origin',(-0.177722310803603,-0.149126725447277,
0.04));
#50697=CARTESIAN_POINT('',(-0.171318218454253,-0.145859754646924,0.04));
#50698=CARTESIAN_POINT('',(-0.173392913664475,-0.143387229176604,0.04));
#50699=CARTESIAN_POINT('Origin',(0.,0.,0.04));
#50700=CARTESIAN_POINT('',(-0.167763733043056,-0.140770486521352,0.04));
#50701=CARTESIAN_POINT('',(-0.183181375296344,-0.162845275475035,0.04));
#50702=CARTESIAN_POINT('',(-0.167763733043056,-0.140770486521352,0.04));
#50703=CARTESIAN_POINT('Origin',(-0.167763733043056,-0.140770486521352,
0.04));
#50704=CARTESIAN_POINT('',(-0.173392913664475,-0.143387229176604,0.235));
#50705=CARTESIAN_POINT('',(-0.173392913664475,-0.143387229176604,0.1175));
#50706=CARTESIAN_POINT('',(-0.167763733043056,-0.140770486521352,0.241));
#50707=CARTESIAN_POINT('',(-0.167763733043056,-0.140770486521352,0.04));
#50708=CARTESIAN_POINT('Ctrl Pts',(-0.173392913664475,-0.143387229176604,
0.235));
#50709=CARTESIAN_POINT('Ctrl Pts',(-0.170540288349525,-0.142061177155342,
0.238043395288999));
#50710=CARTESIAN_POINT('Ctrl Pts',(-0.167763733043056,-0.140770486521352,
0.241));
#50711=CARTESIAN_POINT('Origin',(-0.183181375296344,-0.162845275475035,
0.04));
#50712=CARTESIAN_POINT('',(-0.171318218454253,-0.145859754646924,0.235));
#50713=CARTESIAN_POINT('',(-0.171318218454253,-0.145859754646924,0.1175));
#50714=CARTESIAN_POINT('Ctrl Pts',(-0.167763733043056,-0.140770486521352,
0.241));
#50715=CARTESIAN_POINT('Ctrl Pts',(-0.169516958955354,-0.14328073363737,
0.238043395288925));
#50716=CARTESIAN_POINT('Ctrl Pts',(-0.171318218454253,-0.145859754646924,
0.235));
#50717=CARTESIAN_POINT('Origin',(-0.20091789367799,-0.116,0.04));
#50718=CARTESIAN_POINT('',(-0.194043790355372,-0.113894720793023,0.04));
#50719=CARTESIAN_POINT('',(-0.195657616741379,-0.111099491497862,0.04));
#50720=CARTESIAN_POINT('Origin',(0.,0.,0.04));
#50721=CARTESIAN_POINT('',(-0.189659563428792,-0.1095,0.04));
#50722=CARTESIAN_POINT('',(-0.208676223927188,-0.128562177826491,0.04));
#50723=CARTESIAN_POINT('',(-0.189659563428792,-0.1095,0.04));
#50724=CARTESIAN_POINT('Origin',(-0.189659563428792,-0.1095,0.04));
#50725=CARTESIAN_POINT('',(-0.195657616741379,-0.111099491497862,0.235));
#50726=CARTESIAN_POINT('',(-0.195657616741379,-0.111099491497862,0.1175));
#50727=CARTESIAN_POINT('',(-0.189659563428792,-0.1095,0.241));
#50728=CARTESIAN_POINT('',(-0.189659563428792,-0.1095,0.04));
#50729=CARTESIAN_POINT('Ctrl Pts',(-0.195657616741379,-0.111099491497862,
0.235));
#50730=CARTESIAN_POINT('Ctrl Pts',(-0.192618062697799,-0.110288938373935,
0.238043395288995));
#50731=CARTESIAN_POINT('Ctrl Pts',(-0.189659563428792,-0.1095,0.241));
#50732=CARTESIAN_POINT('Origin',(-0.208676223927188,-0.128562177826491,
0.04));
#50733=CARTESIAN_POINT('',(-0.194043790355372,-0.113894720793023,0.235));
#50734=CARTESIAN_POINT('',(-0.194043790355372,-0.113894720793023,0.1175));
#50735=CARTESIAN_POINT('Ctrl Pts',(-0.189659563428792,-0.1095,0.241));
#50736=CARTESIAN_POINT('Ctrl Pts',(-0.191822053737133,-0.111667666337059,
0.238043395289009));
#50737=CARTESIAN_POINT('Ctrl Pts',(-0.194043790355372,-0.113894720793023,
0.235));
#50738=CARTESIAN_POINT('Origin',(-0.218008688022331,-0.0793486732515551,
0.04));
#50739=CARTESIAN_POINT('',(-0.210873439877438,-0.0784690534813352,0.04));
#50740=CARTESIAN_POINT('',(-0.211977362141128,-0.0754360519890136,0.04));
#50741=CARTESIAN_POINT('Origin',(0.,0.,0.04));
#50742=CARTESIAN_POINT('',(-0.205792683952114,-0.0749024113883215,0.04));
#50743=CARTESIAN_POINT('',(-0.227830551089268,-0.0903727834602902,0.04));
#50744=CARTESIAN_POINT('',(-0.205792683952114,-0.0749024113883215,0.04));
#50745=CARTESIAN_POINT('Origin',(-0.205792683952114,-0.0749024113883215,
0.04));
#50746=CARTESIAN_POINT('',(-0.211977362141128,-0.0754360519890136,0.235));
#50747=CARTESIAN_POINT('',(-0.211977362141128,-0.0754360519890136,0.1175));
#50748=CARTESIAN_POINT('',(-0.205792683952114,-0.0749024113883215,0.241));
#50749=CARTESIAN_POINT('',(-0.205792683952114,-0.0749024113883215,0.04));
#50750=CARTESIAN_POINT('Ctrl Pts',(-0.211977362141128,-0.0754360519890136,
0.235));
#50751=CARTESIAN_POINT('Ctrl Pts',(-0.208843234680406,-0.0751656260089268,
0.238043395289026));
#50752=CARTESIAN_POINT('Ctrl Pts',(-0.205792683952114,-0.0749024113883215,
0.241));
#50753=CARTESIAN_POINT('Origin',(-0.227830551089268,-0.0903727834602902,
0.04));
#50754=CARTESIAN_POINT('',(-0.210873439877438,-0.0784690534813352,0.235));
#50755=CARTESIAN_POINT('',(-0.210873439877438,-0.0784690534813352,0.1175));
#50756=CARTESIAN_POINT('Ctrl Pts',(-0.205792683952114,-0.0749024113883215,
0.241));
#50757=CARTESIAN_POINT('Ctrl Pts',(-0.208298732482853,-0.0766616335017707,
0.23804339528895));
#50758=CARTESIAN_POINT('Ctrl Pts',(-0.210873439877438,-0.0784690534813352,
0.235));
#50759=CARTESIAN_POINT('Origin',(-0.228475398698832,-0.0402863772187278,
0.04));
#50760=CARTESIAN_POINT('',(-0.221295806635937,-0.0406591436868744,0.04));
#50761=CARTESIAN_POINT('',(-0.221856282657939,-0.0374805262129627,0.04));
#50762=CARTESIAN_POINT('Origin',(0.,0.,0.04));
#50763=CARTESIAN_POINT('',(-0.215672897909674,-0.0380289509090577,0.04));
#50764=CARTESIAN_POINT('',(-0.240062362244323,-0.0494374577994833,0.04));
#50765=CARTESIAN_POINT('',(-0.215672897909674,-0.0380289509090577,0.04));
#50766=CARTESIAN_POINT('Origin',(-0.215672897909674,-0.0380289509090577,
0.04));
#50767=CARTESIAN_POINT('',(-0.221856282657939,-0.0374805262129627,0.235));
#50768=CARTESIAN_POINT('',(-0.221856282657939,-0.0374805262129627,0.1175));
#50769=CARTESIAN_POINT('',(-0.215672897909674,-0.0380289509090577,0.241));
#50770=CARTESIAN_POINT('',(-0.215672897909674,-0.0380289509090577,0.04));
#50771=CARTESIAN_POINT('Ctrl Pts',(-0.221856282657939,-0.0374805262129627,
0.235));
#50772=CARTESIAN_POINT('Ctrl Pts',(-0.218722810657085,-0.037758444133285,
0.238043395288998));
#50773=CARTESIAN_POINT('Ctrl Pts',(-0.215672897909674,-0.0380289509090577,
0.241));
#50774=CARTESIAN_POINT('Origin',(-0.240062362244323,-0.0494374577994833,
0.04));
#50775=CARTESIAN_POINT('',(-0.221295806635937,-0.0406591436868744,0.235));
#50776=CARTESIAN_POINT('',(-0.221295806635937,-0.0406591436868744,0.1175));
#50777=CARTESIAN_POINT('Ctrl Pts',(-0.215672897909674,-0.0380289509090577,
0.241));
#50778=CARTESIAN_POINT('Ctrl Pts',(-0.218446359646305,-0.0393262757251562,
0.238043395288925));
#50779=CARTESIAN_POINT('Ctrl Pts',(-0.221295806635937,-0.0406591436868744,
0.235));
#50780=CARTESIAN_POINT('Origin',(-0.232,2.77555756156289E-17,0.04));
#50781=CARTESIAN_POINT('',(-0.224994212290885,-0.00161382638600747,0.04));
#50782=CARTESIAN_POINT('',(-0.225,-2.75545529808154E-17,0.04));
#50783=CARTESIAN_POINT('Origin',(0.,0.,0.04));
#50784=CARTESIAN_POINT('',(-0.219,2.77555756156289E-17,0.04));
#50785=CARTESIAN_POINT('',(-0.245,-0.00699999999999998,0.04));
#50786=CARTESIAN_POINT('',(-0.224994212290885,0.00161382638600753,0.04));
#50787=CARTESIAN_POINT('',(-0.219,2.77555756156289E-17,0.04));
#50788=CARTESIAN_POINT('Origin',(0.,0.,0.04));
#50789=CARTESIAN_POINT('Origin',(-0.219,2.77555756156289E-17,0.04));
#50790=CARTESIAN_POINT('',(-0.224994212290885,0.00161382638600753,0.235));
#50791=CARTESIAN_POINT('',(-0.224994212290885,0.00161382638600753,0.1175));
#50792=CARTESIAN_POINT('',(-0.219,2.77555756156289E-17,0.241));
#50793=CARTESIAN_POINT('',(-0.219,2.77555756156289E-17,0.04));
#50794=CARTESIAN_POINT('Ctrl Pts',(-0.224994212290885,0.00161382638600752,
0.235));
#50795=CARTESIAN_POINT('Ctrl Pts',(-0.221956604711078,0.000796008960674882,
0.238043395288922));
#50796=CARTESIAN_POINT('Ctrl Pts',(-0.219,2.77555756156289E-17,0.241));
#50797=CARTESIAN_POINT('Origin',(-0.245,-0.00699999999999998,0.04));
#50798=CARTESIAN_POINT('',(-0.224994212290885,-0.00161382638600747,0.235));
#50799=CARTESIAN_POINT('',(-0.224994212290885,-0.00161382638600747,0.1175));
#50800=CARTESIAN_POINT('Ctrl Pts',(-0.219,2.77555756156289E-17,0.241));
#50801=CARTESIAN_POINT('Ctrl Pts',(-0.221956604711001,-0.000796008960654102,
0.238043395288999));
#50802=CARTESIAN_POINT('Ctrl Pts',(-0.224994212290885,-0.00161382638600745,
0.235));
#50803=CARTESIAN_POINT('Origin',(-0.228475398698832,0.0402863772187279,
0.04));
#50804=CARTESIAN_POINT('',(-0.221856282657939,0.0374805262129629,0.04));
#50805=CARTESIAN_POINT('',(-0.221295806635937,0.0406591436868746,0.04));
#50806=CARTESIAN_POINT('Origin',(0.,0.,0.04));
#50807=CARTESIAN_POINT('',(-0.215672897909674,0.0380289509090578,0.04));
#50808=CARTESIAN_POINT('',(-0.24249343673166,0.0356501492573126,0.04));
#50809=CARTESIAN_POINT('',(-0.215672897909674,0.0380289509090578,0.04));
#50810=CARTESIAN_POINT('Origin',(-0.215672897909674,0.0380289509090578,
0.04));
#50811=CARTESIAN_POINT('',(-0.221295806635937,0.0406591436868746,0.235));
#50812=CARTESIAN_POINT('',(-0.221295806635937,0.0406591436868746,0.1175));
#50813=CARTESIAN_POINT('',(-0.215672897909674,0.0380289509090578,0.241));
#50814=CARTESIAN_POINT('',(-0.215672897909674,0.0380289509090578,0.04));
#50815=CARTESIAN_POINT('Ctrl Pts',(-0.221295806635937,0.0406591436868746,
0.235));
#50816=CARTESIAN_POINT('Ctrl Pts',(-0.218446359646237,0.0393262757251244,
0.238043395288998));
#50817=CARTESIAN_POINT('Ctrl Pts',(-0.215672897909674,0.0380289509090578,
0.241));
#50818=CARTESIAN_POINT('Origin',(-0.24249343673166,0.0356501492573126,0.04));
#50819=CARTESIAN_POINT('',(-0.221856282657939,0.0374805262129629,0.235));
#50820=CARTESIAN_POINT('',(-0.221856282657939,0.0374805262129629,0.1175));
#50821=CARTESIAN_POINT('Ctrl Pts',(-0.215672897909674,0.0380289509090578,
0.241));
#50822=CARTESIAN_POINT('Ctrl Pts',(-0.218722810657132,0.037758444133281,
0.238043395288953));
#50823=CARTESIAN_POINT('Ctrl Pts',(-0.221856282657939,0.0374805262129629,
0.235));
#50824=CARTESIAN_POINT('Origin',(-0.218008688022331,0.0793486732515552,
0.04));
#50825=CARTESIAN_POINT('',(-0.211977362141128,0.0754360519890136,0.04));
#50826=CARTESIAN_POINT('',(-0.210873439877438,0.0784690534813353,0.04));
#50827=CARTESIAN_POINT('Origin',(0.,0.,0.04));
#50828=CARTESIAN_POINT('',(-0.205792683952114,0.0749024113883215,0.04));
#50829=CARTESIAN_POINT('',(-0.232618833095827,0.0772170867692875,0.04));
#50830=CARTESIAN_POINT('',(-0.205792683952114,0.0749024113883215,0.04));
#50831=CARTESIAN_POINT('Origin',(-0.205792683952114,0.0749024113883215,
0.04));
#50832=CARTESIAN_POINT('',(-0.210873439877438,0.0784690534813353,0.235));
#50833=CARTESIAN_POINT('',(-0.210873439877438,0.0784690534813353,0.1175));
#50834=CARTESIAN_POINT('',(-0.205792683952114,0.0749024113883215,0.241));
#50835=CARTESIAN_POINT('',(-0.205792683952114,0.0749024113883215,0.04));
#50836=CARTESIAN_POINT('Ctrl Pts',(-0.210873439877438,0.0784690534813352,
0.235));
#50837=CARTESIAN_POINT('Ctrl Pts',(-0.208298732482843,0.0766616335017642,
0.238043395288961));
#50838=CARTESIAN_POINT('Ctrl Pts',(-0.205792683952114,0.0749024113883215,
0.241));
#50839=CARTESIAN_POINT('Origin',(-0.232618833095827,0.0772170867692875,
0.04));
#50840=CARTESIAN_POINT('',(-0.211977362141128,0.0754360519890136,0.235));
#50841=CARTESIAN_POINT('',(-0.211977362141128,0.0754360519890136,0.1175));
#50842=CARTESIAN_POINT('Ctrl Pts',(-0.205792683952114,0.0749024113883215,
0.241));
#50843=CARTESIAN_POINT('Ctrl Pts',(-0.208843234680461,0.0751656260089316,
0.238043395288973));
#50844=CARTESIAN_POINT('Ctrl Pts',(-0.211977362141128,0.0754360519890136,
0.235));
#50845=CARTESIAN_POINT('Origin',(-0.20091789367799,0.116,0.04));
#50846=CARTESIAN_POINT('',(-0.195657616741379,0.111099491497862,0.04));
#50847=CARTESIAN_POINT('',(-0.194043790355372,0.113894720793023,0.04));
#50848=CARTESIAN_POINT('Origin',(0.,0.,0.04));
#50849=CARTESIAN_POINT('',(-0.189659563428792,0.1095,0.04));
#50850=CARTESIAN_POINT('',(-0.215676223927188,0.116437822173509,0.04));
#50851=CARTESIAN_POINT('',(-0.189659563428792,0.1095,0.04));
#50852=CARTESIAN_POINT('Origin',(-0.189659563428792,0.1095,0.04));
#50853=CARTESIAN_POINT('',(-0.194043790355372,0.113894720793023,0.235));
#50854=CARTESIAN_POINT('',(-0.194043790355372,0.113894720793023,0.1175));
#50855=CARTESIAN_POINT('',(-0.189659563428792,0.1095,0.241));
#50856=CARTESIAN_POINT('',(-0.189659563428792,0.1095,0.04));
#50857=CARTESIAN_POINT('Ctrl Pts',(-0.194043790355372,0.113894720793023,
0.235));
#50858=CARTESIAN_POINT('Ctrl Pts',(-0.19182205373716,0.111667666337086,
0.238043395288973));
#50859=CARTESIAN_POINT('Ctrl Pts',(-0.189659563428792,0.1095,0.241));
#50860=CARTESIAN_POINT('Origin',(-0.215676223927188,0.116437822173509,0.04));
#50861=CARTESIAN_POINT('',(-0.195657616741379,0.111099491497862,0.235));
#50862=CARTESIAN_POINT('',(-0.195657616741379,0.111099491497862,0.1175));
#50863=CARTESIAN_POINT('Ctrl Pts',(-0.189659563428792,0.1095,0.241));
#50864=CARTESIAN_POINT('Ctrl Pts',(-0.192618062697796,0.110288938373934,
0.238043395288998));
#50865=CARTESIAN_POINT('Ctrl Pts',(-0.195657616741379,0.111099491497862,
0.235));
#50866=CARTESIAN_POINT('Origin',(-0.177722310803603,0.149126725447277,0.04));
#50867=CARTESIAN_POINT('',(-0.173392913664475,0.143387229176604,0.04));
#50868=CARTESIAN_POINT('',(-0.171318218454253,0.145859754646924,0.04));
#50869=CARTESIAN_POINT('Origin',(0.,0.,0.04));
#50870=CARTESIAN_POINT('',(-0.167763733043056,0.140770486521352,0.04));
#50871=CARTESIAN_POINT('',(-0.192180401831955,0.152120653271369,0.04));
#50872=CARTESIAN_POINT('',(-0.167763733043056,0.140770486521352,0.04));
#50873=CARTESIAN_POINT('Origin',(-0.167763733043056,0.140770486521352,0.04));
#50874=CARTESIAN_POINT('',(-0.171318218454253,0.145859754646924,0.235));
#50875=CARTESIAN_POINT('',(-0.171318218454253,0.145859754646924,0.1175));
#50876=CARTESIAN_POINT('',(-0.167763733043056,0.140770486521352,0.241));
#50877=CARTESIAN_POINT('',(-0.167763733043056,0.140770486521352,0.04));
#50878=CARTESIAN_POINT('Ctrl Pts',(-0.171318218454253,0.145859754646924,
0.235));
#50879=CARTESIAN_POINT('Ctrl Pts',(-0.169516958955308,0.143280733637303,
0.238043395289003));
#50880=CARTESIAN_POINT('Ctrl Pts',(-0.167763733043056,0.140770486521352,
0.241));
#50881=CARTESIAN_POINT('Origin',(-0.192180401831955,0.152120653271369,0.04));
#50882=CARTESIAN_POINT('',(-0.173392913664475,0.143387229176604,0.235));
#50883=CARTESIAN_POINT('',(-0.173392913664475,0.143387229176604,0.1175));
#50884=CARTESIAN_POINT('Ctrl Pts',(-0.167763733043056,0.140770486521352,
0.241));
#50885=CARTESIAN_POINT('Ctrl Pts',(-0.170540288349497,0.142061177155329,
0.238043395289029));
#50886=CARTESIAN_POINT('Ctrl Pts',(-0.173392913664475,0.143387229176604,
0.235));
#50887=CARTESIAN_POINT('Origin',(-0.149126725447277,0.177722310803603,0.04));
#50888=CARTESIAN_POINT('',(-0.145859754646924,0.171318218454253,0.04));
#50889=CARTESIAN_POINT('',(-0.143387229176604,0.173392913664475,0.04));
#50890=CARTESIAN_POINT('Origin',(0.,0.,0.04));
#50891=CARTESIAN_POINT('',(-0.140770486521352,0.167763733043056,0.04));
#50892=CARTESIAN_POINT('',(-0.162845275475035,0.183181375296344,0.04));
#50893=CARTESIAN_POINT('',(-0.140770486521352,0.167763733043056,0.04));
#50894=CARTESIAN_POINT('Origin',(-0.140770486521352,0.167763733043056,0.04));
#50895=CARTESIAN_POINT('',(-0.143387229176604,0.173392913664475,0.235));
#50896=CARTESIAN_POINT('',(-0.143387229176604,0.173392913664475,0.1175));
#50897=CARTESIAN_POINT('',(-0.140770486521352,0.167763733043056,0.241));
#50898=CARTESIAN_POINT('',(-0.140770486521352,0.167763733043056,0.04));
#50899=CARTESIAN_POINT('Ctrl Pts',(-0.143387229176604,0.173392913664475,
0.235));
#50900=CARTESIAN_POINT('Ctrl Pts',(-0.14206117715533,0.170540288349499,
0.238043395289028));
#50901=CARTESIAN_POINT('Ctrl Pts',(-0.140770486521352,0.167763733043056,
0.241));
#50902=CARTESIAN_POINT('Origin',(-0.162845275475035,0.183181375296344,0.04));
#50903=CARTESIAN_POINT('',(-0.145859754646924,0.171318218454253,0.235));
#50904=CARTESIAN_POINT('',(-0.145859754646924,0.171318218454253,0.1175));
#50905=CARTESIAN_POINT('Ctrl Pts',(-0.140770486521352,0.167763733043056,
0.241));
#50906=CARTESIAN_POINT('Ctrl Pts',(-0.143280733637291,0.169516958955299,
0.238043395289017));
#50907=CARTESIAN_POINT('Ctrl Pts',(-0.145859754646924,0.171318218454253,
0.235));
#50908=CARTESIAN_POINT('Origin',(-0.116,0.20091789367799,0.04));
#50909=CARTESIAN_POINT('',(-0.113894720793023,0.194043790355372,0.04));
#50910=CARTESIAN_POINT('',(-0.111099491497862,0.195657616741379,0.04));
#50911=CARTESIAN_POINT('Origin',(0.,0.,0.04));
#50912=CARTESIAN_POINT('',(-0.1095,0.189659563428792,0.04));
#50913=CARTESIAN_POINT('',(-0.128562177826491,0.208676223927188,0.04));
#50914=CARTESIAN_POINT('',(-0.1095,0.189659563428792,0.04));
#50915=CARTESIAN_POINT('Origin',(-0.1095,0.189659563428792,0.04));
#50916=CARTESIAN_POINT('',(-0.111099491497862,0.195657616741379,0.235));
#50917=CARTESIAN_POINT('',(-0.111099491497862,0.195657616741379,0.1175));
#50918=CARTESIAN_POINT('',(-0.1095,0.189659563428792,0.241));
#50919=CARTESIAN_POINT('',(-0.1095,0.189659563428792,0.04));
#50920=CARTESIAN_POINT('Ctrl Pts',(-0.111099491497862,0.195657616741379,
0.235));
#50921=CARTESIAN_POINT('Ctrl Pts',(-0.110288938373934,0.192618062697795,
0.238043395288999));
#50922=CARTESIAN_POINT('Ctrl Pts',(-0.1095,0.189659563428792,0.241));
#50923=CARTESIAN_POINT('Origin',(-0.128562177826491,0.208676223927188,0.04));
#50924=CARTESIAN_POINT('',(-0.113894720793023,0.194043790355372,0.235));
#50925=CARTESIAN_POINT('',(-0.113894720793023,0.194043790355372,0.1175));
#50926=CARTESIAN_POINT('Ctrl Pts',(-0.1095,0.189659563428792,0.241));
#50927=CARTESIAN_POINT('Ctrl Pts',(-0.111667666337081,0.191822053737154,
0.23804339528898));
#50928=CARTESIAN_POINT('Ctrl Pts',(-0.113894720793023,0.194043790355372,
0.235));
#50929=CARTESIAN_POINT('Origin',(-0.0793486732515551,0.218008688022331,
0.04));
#50930=CARTESIAN_POINT('',(-0.0784690534813352,0.210873439877438,0.04));
#50931=CARTESIAN_POINT('',(-0.0754360519890136,0.211977362141128,0.04));
#50932=CARTESIAN_POINT('Origin',(0.,0.,0.04));
#50933=CARTESIAN_POINT('',(-0.0749024113883215,0.205792683952114,0.04));
#50934=CARTESIAN_POINT('',(-0.0903727834602902,0.227830551089268,0.04));
#50935=CARTESIAN_POINT('',(-0.0749024113883215,0.205792683952114,0.04));
#50936=CARTESIAN_POINT('Origin',(-0.0749024113883215,0.205792683952114,
0.04));
#50937=CARTESIAN_POINT('',(-0.0754360519890136,0.211977362141128,0.235));
#50938=CARTESIAN_POINT('',(-0.0754360519890136,0.211977362141128,0.1175));
#50939=CARTESIAN_POINT('',(-0.0749024113883215,0.205792683952114,0.241));
#50940=CARTESIAN_POINT('',(-0.0749024113883215,0.205792683952114,0.04));
#50941=CARTESIAN_POINT('Ctrl Pts',(-0.0754360519890136,0.211977362141128,
0.235));
#50942=CARTESIAN_POINT('Ctrl Pts',(-0.0751656260089268,0.208843234680406,
0.238043395289026));
#50943=CARTESIAN_POINT('Ctrl Pts',(-0.0749024113883215,0.205792683952114,
0.241));
#50944=CARTESIAN_POINT('Origin',(-0.0903727834602902,0.227830551089268,
0.04));
#50945=CARTESIAN_POINT('',(-0.0784690534813352,0.210873439877438,0.235));
#50946=CARTESIAN_POINT('',(-0.0784690534813352,0.210873439877438,0.1175));
#50947=CARTESIAN_POINT('Ctrl Pts',(-0.0749024113883215,0.205792683952114,
0.241));
#50948=CARTESIAN_POINT('Ctrl Pts',(-0.0766616335017707,0.208298732482853,
0.23804339528895));
#50949=CARTESIAN_POINT('Ctrl Pts',(-0.0784690534813352,0.210873439877438,
0.235));
#50950=CARTESIAN_POINT('Origin',(-0.0402863772187278,0.228475398698832,
0.04));
#50951=CARTESIAN_POINT('',(-0.0406591436868745,0.221295806635937,0.04));
#50952=CARTESIAN_POINT('',(-0.0374805262129628,0.221856282657939,0.04));
#50953=CARTESIAN_POINT('Origin',(0.,0.,0.04));
#50954=CARTESIAN_POINT('',(-0.0380289509090578,0.215672897909674,0.04));
#50955=CARTESIAN_POINT('',(-0.0494374577994834,0.240062362244323,0.04));
#50956=CARTESIAN_POINT('',(-0.0380289509090578,0.215672897909674,0.04));
#50957=CARTESIAN_POINT('Origin',(-0.0380289509090578,0.215672897909674,
0.04));
#50958=CARTESIAN_POINT('',(-0.0374805262129628,0.221856282657939,0.235));
#50959=CARTESIAN_POINT('',(-0.0374805262129628,0.221856282657939,0.1175));
#50960=CARTESIAN_POINT('',(-0.0380289509090578,0.215672897909674,0.241));
#50961=CARTESIAN_POINT('',(-0.0380289509090578,0.215672897909674,0.04));
#50962=CARTESIAN_POINT('Ctrl Pts',(-0.0374805262129628,0.221856282657939,
0.235));
#50963=CARTESIAN_POINT('Ctrl Pts',(-0.037758444133279,0.218722810657154,
0.238043395288931));
#50964=CARTESIAN_POINT('Ctrl Pts',(-0.0380289509090578,0.215672897909674,
0.241));
#50965=CARTESIAN_POINT('Origin',(-0.0494374577994834,0.240062362244323,
0.04));
#50966=CARTESIAN_POINT('',(-0.0406591436868745,0.221295806635937,0.235));
#50967=CARTESIAN_POINT('',(-0.0406591436868745,0.221295806635937,0.1175));
#50968=CARTESIAN_POINT('Ctrl Pts',(-0.0380289509090578,0.215672897909674,
0.241));
#50969=CARTESIAN_POINT('Ctrl Pts',(-0.0393262757251606,0.218446359646314,
0.238043395288915));
#50970=CARTESIAN_POINT('Ctrl Pts',(-0.0406591436868745,0.221295806635937,
0.235));
#50971=CARTESIAN_POINT('Origin',(1.38777878078145E-17,0.232,0.04));
#50972=CARTESIAN_POINT('',(-0.00161382638600747,0.224994212290885,0.04));
#50973=CARTESIAN_POINT('',(0.0016138263860075,0.224994212290885,0.04));
#50974=CARTESIAN_POINT('Origin',(0.,0.,0.04));
#50975=CARTESIAN_POINT('',(1.38777878078145E-17,0.219,0.04));
#50976=CARTESIAN_POINT('',(-0.00699999999999999,0.245,0.04));
#50977=CARTESIAN_POINT('',(1.38777878078145E-17,0.219,0.04));
#50978=CARTESIAN_POINT('Origin',(1.38777878078145E-17,0.219,0.04));
#50979=CARTESIAN_POINT('',(0.00161382638600752,0.224994212290885,0.235));
#50980=CARTESIAN_POINT('',(0.00161382638600752,0.224994212290885,0.1175));
#50981=CARTESIAN_POINT('',(1.38777878078145E-17,0.219,0.241));
#50982=CARTESIAN_POINT('',(1.38777878078145E-17,0.219,0.04));
#50983=CARTESIAN_POINT('Ctrl Pts',(0.00161382638600749,0.224994212290885,
0.235));
#50984=CARTESIAN_POINT('Ctrl Pts',(0.000796008960674862,0.221956604711078,
0.238043395288922));
#50985=CARTESIAN_POINT('Ctrl Pts',(1.38777878078145E-17,0.219,0.241));
#50986=CARTESIAN_POINT('Origin',(-0.00699999999999999,0.245,0.04));
#50987=CARTESIAN_POINT('',(-0.00161382638600748,0.224994212290885,0.235));
#50988=CARTESIAN_POINT('',(-0.00161382638600748,0.224994212290885,0.1175));
#50989=CARTESIAN_POINT('Ctrl Pts',(1.38777878078145E-17,0.219,0.241));
#50990=CARTESIAN_POINT('Ctrl Pts',(-0.000796008960647555,0.221956604710977,
0.238043395289023));
#50991=CARTESIAN_POINT('Ctrl Pts',(-0.00161382638600747,0.224994212290885,
0.235));
#50992=CARTESIAN_POINT('Origin',(0.0402863772187279,0.228475398698832,0.04));
#50993=CARTESIAN_POINT('',(0.0374805262129628,0.221856282657939,0.04));
#50994=CARTESIAN_POINT('',(0.0406591436868745,0.221295806635937,0.04));
#50995=CARTESIAN_POINT('Origin',(0.,0.,0.04));
#50996=CARTESIAN_POINT('',(0.0380289509090578,0.215672897909674,0.04));
#50997=CARTESIAN_POINT('',(0.0356501492573125,0.24249343673166,0.04));
#50998=CARTESIAN_POINT('',(0.0380289509090578,0.215672897909674,0.04));
#50999=CARTESIAN_POINT('Origin',(0.0380289509090578,0.215672897909674,0.04));
#51000=CARTESIAN_POINT('',(0.0406591436868745,0.221295806635937,0.235));
#51001=CARTESIAN_POINT('',(0.0406591436868745,0.221295806635937,0.1175));
#51002=CARTESIAN_POINT('',(0.0380289509090578,0.215672897909674,0.241));
#51003=CARTESIAN_POINT('',(0.0380289509090578,0.215672897909674,0.04));
#51004=CARTESIAN_POINT('Ctrl Pts',(0.0406591436868745,0.221295806635937,
0.235));
#51005=CARTESIAN_POINT('Ctrl Pts',(0.0393262757251286,0.218446359646246,
0.238043395288988));
#51006=CARTESIAN_POINT('Ctrl Pts',(0.0380289509090578,0.215672897909674,
0.241));
#51007=CARTESIAN_POINT('Origin',(0.0356501492573125,0.24249343673166,0.04));
#51008=CARTESIAN_POINT('',(0.0374805262129628,0.221856282657939,0.235));
#51009=CARTESIAN_POINT('',(0.0374805262129628,0.221856282657939,0.1175));
#51010=CARTESIAN_POINT('Ctrl Pts',(0.0380289509090578,0.215672897909674,
0.241));
#51011=CARTESIAN_POINT('Ctrl Pts',(0.0377584441332792,0.218722810657151,
0.238043395288934));
#51012=CARTESIAN_POINT('Ctrl Pts',(0.0374805262129628,0.221856282657939,
0.235));
#51013=CARTESIAN_POINT('Origin',(0.0793486732515552,0.218008688022331,0.04));
#51014=CARTESIAN_POINT('',(0.0754360519890136,0.211977362141128,0.04));
#51015=CARTESIAN_POINT('',(0.0784690534813353,0.210873439877438,0.04));
#51016=CARTESIAN_POINT('Origin',(0.,0.,0.04));
#51017=CARTESIAN_POINT('',(0.0749024113883215,0.205792683952114,0.04));
#51018=CARTESIAN_POINT('',(0.0772170867692875,0.232618833095827,0.04));
#51019=CARTESIAN_POINT('',(0.0749024113883215,0.205792683952114,0.04));
#51020=CARTESIAN_POINT('Origin',(0.0749024113883215,0.205792683952114,0.04));
#51021=CARTESIAN_POINT('',(0.0784690534813353,0.210873439877438,0.235));
#51022=CARTESIAN_POINT('',(0.0784690534813353,0.210873439877438,0.1175));
#51023=CARTESIAN_POINT('',(0.0749024113883215,0.205792683952114,0.241));
#51024=CARTESIAN_POINT('',(0.0749024113883215,0.205792683952114,0.04));
#51025=CARTESIAN_POINT('Ctrl Pts',(0.0784690534813352,0.210873439877438,
0.235));
#51026=CARTESIAN_POINT('Ctrl Pts',(0.0766616335017642,0.208298732482843,
0.238043395288961));
#51027=CARTESIAN_POINT('Ctrl Pts',(0.0749024113883215,0.205792683952114,
0.241));
#51028=CARTESIAN_POINT('Origin',(0.0772170867692875,0.232618833095827,0.04));
#51029=CARTESIAN_POINT('',(0.0754360519890136,0.211977362141128,0.235));
#51030=CARTESIAN_POINT('',(0.0754360519890136,0.211977362141128,0.1175));
#51031=CARTESIAN_POINT('Ctrl Pts',(0.0749024113883215,0.205792683952114,
0.241));
#51032=CARTESIAN_POINT('Ctrl Pts',(0.0751656260089316,0.208843234680461,
0.238043395288973));
#51033=CARTESIAN_POINT('Ctrl Pts',(0.0754360519890136,0.211977362141128,
0.235));
#51034=CARTESIAN_POINT('Origin',(0.116,0.20091789367799,0.04));
#51035=CARTESIAN_POINT('',(0.111099491497862,0.195657616741379,0.04));
#51036=CARTESIAN_POINT('',(0.113894720793023,0.194043790355372,0.04));
#51037=CARTESIAN_POINT('Origin',(0.,0.,0.04));
#51038=CARTESIAN_POINT('',(0.1095,0.189659563428792,0.04));
#51039=CARTESIAN_POINT('',(0.116437822173509,0.215676223927188,0.04));
#51040=CARTESIAN_POINT('',(0.1095,0.189659563428792,0.04));
#51041=CARTESIAN_POINT('Origin',(0.1095,0.189659563428792,0.04));
#51042=CARTESIAN_POINT('',(0.113894720793023,0.194043790355372,0.235));
#51043=CARTESIAN_POINT('',(0.113894720793023,0.194043790355372,0.1175));
#51044=CARTESIAN_POINT('',(0.1095,0.189659563428792,0.241));
#51045=CARTESIAN_POINT('',(0.1095,0.189659563428792,0.04));
#51046=CARTESIAN_POINT('Ctrl Pts',(0.113894720793023,0.194043790355372,
0.235));
#51047=CARTESIAN_POINT('Ctrl Pts',(0.111667666337037,0.19182205373711,0.23804339528904));
#51048=CARTESIAN_POINT('Ctrl Pts',(0.1095,0.189659563428792,0.241));
#51049=CARTESIAN_POINT('Origin',(0.116437822173509,0.215676223927188,0.04));
#51050=CARTESIAN_POINT('',(0.111099491497862,0.195657616741379,0.235));
#51051=CARTESIAN_POINT('',(0.111099491497862,0.195657616741379,0.1175));
#51052=CARTESIAN_POINT('Ctrl Pts',(0.1095,0.189659563428792,0.241));
#51053=CARTESIAN_POINT('Ctrl Pts',(0.110288938373932,0.192618062697786,
0.238043395289008));
#51054=CARTESIAN_POINT('Ctrl Pts',(0.111099491497862,0.195657616741379,
0.235));
#51055=CARTESIAN_POINT('Origin',(0.149126725447277,0.177722310803603,0.04));
#51056=CARTESIAN_POINT('',(0.143387229176604,0.173392913664475,0.04));
#51057=CARTESIAN_POINT('',(0.145859754646924,0.171318218454253,0.04));
#51058=CARTESIAN_POINT('Origin',(0.,0.,0.04));
#51059=CARTESIAN_POINT('',(0.140770486521352,0.167763733043056,0.04));
#51060=CARTESIAN_POINT('',(0.152120653271369,0.192180401831955,0.04));
#51061=CARTESIAN_POINT('',(0.140770486521352,0.167763733043056,0.04));
#51062=CARTESIAN_POINT('Origin',(0.140770486521352,0.167763733043056,0.04));
#51063=CARTESIAN_POINT('',(0.145859754646924,0.171318218454253,0.235));
#51064=CARTESIAN_POINT('',(0.145859754646924,0.171318218454253,0.1175));
#51065=CARTESIAN_POINT('',(0.140770486521352,0.167763733043056,0.241));
#51066=CARTESIAN_POINT('',(0.140770486521352,0.167763733043056,0.04));
#51067=CARTESIAN_POINT('Ctrl Pts',(0.145859754646924,0.171318218454253,
0.235));
#51068=CARTESIAN_POINT('Ctrl Pts',(0.143280733637348,0.169516958955339,
0.23804339528895));
#51069=CARTESIAN_POINT('Ctrl Pts',(0.140770486521352,0.167763733043056,
0.241));
#51070=CARTESIAN_POINT('Origin',(0.152120653271369,0.192180401831955,0.04));
#51071=CARTESIAN_POINT('',(0.143387229176604,0.173392913664475,0.235));
#51072=CARTESIAN_POINT('',(0.143387229176604,0.173392913664475,0.1175));
#51073=CARTESIAN_POINT('Ctrl Pts',(0.140770486521352,0.167763733043056,
0.241));
#51074=CARTESIAN_POINT('Ctrl Pts',(0.142061177155356,0.170540288349555,
0.238043395288967));
#51075=CARTESIAN_POINT('Ctrl Pts',(0.143387229176604,0.173392913664475,
0.235));
#51076=CARTESIAN_POINT('Origin',(0.177722310803603,0.149126725447277,0.04));
#51077=CARTESIAN_POINT('',(0.171318218454253,0.145859754646924,0.04));
#51078=CARTESIAN_POINT('',(0.173392913664475,0.143387229176604,0.04));
#51079=CARTESIAN_POINT('Origin',(0.,0.,0.04));
#51080=CARTESIAN_POINT('',(0.167763733043056,0.140770486521352,0.04));
#51081=CARTESIAN_POINT('',(0.183181375296344,0.162845275475035,0.04));
#51082=CARTESIAN_POINT('',(0.167763733043056,0.140770486521352,0.04));
#51083=CARTESIAN_POINT('Origin',(0.167763733043056,0.140770486521352,0.04));
#51084=CARTESIAN_POINT('',(0.173392913664475,0.143387229176604,0.235));
#51085=CARTESIAN_POINT('',(0.173392913664475,0.143387229176604,0.1175));
#51086=CARTESIAN_POINT('',(0.167763733043056,0.140770486521352,0.241));
#51087=CARTESIAN_POINT('',(0.167763733043056,0.140770486521352,0.04));
#51088=CARTESIAN_POINT('Ctrl Pts',(0.173392913664475,0.143387229176604,
0.235));
#51089=CARTESIAN_POINT('Ctrl Pts',(0.170540288349525,0.142061177155342,
0.238043395288999));
#51090=CARTESIAN_POINT('Ctrl Pts',(0.167763733043056,0.140770486521352,
0.241));
#51091=CARTESIAN_POINT('Origin',(0.183181375296344,0.162845275475035,0.04));
#51092=CARTESIAN_POINT('',(0.171318218454253,0.145859754646924,0.235));
#51093=CARTESIAN_POINT('',(0.171318218454253,0.145859754646924,0.1175));
#51094=CARTESIAN_POINT('Ctrl Pts',(0.167763733043056,0.140770486521352,
0.241));
#51095=CARTESIAN_POINT('Ctrl Pts',(0.169516958955354,0.14328073363737,0.238043395288925));
#51096=CARTESIAN_POINT('Ctrl Pts',(0.171318218454253,0.145859754646924,
0.235));
#51097=CARTESIAN_POINT('Origin',(0.20091789367799,0.116,0.04));
#51098=CARTESIAN_POINT('',(0.194043790355372,0.113894720793023,0.04));
#51099=CARTESIAN_POINT('',(0.195657616741379,0.111099491497862,0.04));
#51100=CARTESIAN_POINT('Origin',(0.,0.,0.04));
#51101=CARTESIAN_POINT('',(0.189659563428792,0.1095,0.04));
#51102=CARTESIAN_POINT('',(0.208676223927188,0.128562177826491,0.04));
#51103=CARTESIAN_POINT('',(0.189659563428792,0.1095,0.04));
#51104=CARTESIAN_POINT('Origin',(0.189659563428792,0.1095,0.04));
#51105=CARTESIAN_POINT('',(0.195657616741379,0.111099491497862,0.235));
#51106=CARTESIAN_POINT('',(0.195657616741379,0.111099491497862,0.1175));
#51107=CARTESIAN_POINT('',(0.189659563428792,0.1095,0.241));
#51108=CARTESIAN_POINT('',(0.189659563428792,0.1095,0.04));
#51109=CARTESIAN_POINT('Ctrl Pts',(0.195657616741379,0.111099491497862,
0.235));
#51110=CARTESIAN_POINT('Ctrl Pts',(0.192618062697788,0.110288938373932,
0.238043395289006));
#51111=CARTESIAN_POINT('Ctrl Pts',(0.189659563428792,0.1095,0.241));
#51112=CARTESIAN_POINT('Origin',(0.208676223927188,0.128562177826491,0.04));
#51113=CARTESIAN_POINT('',(0.194043790355372,0.113894720793023,0.235));
#51114=CARTESIAN_POINT('',(0.194043790355372,0.113894720793023,0.1175));
#51115=CARTESIAN_POINT('Ctrl Pts',(0.189659563428792,0.1095,0.241));
#51116=CARTESIAN_POINT('Ctrl Pts',(0.191822053737141,0.111667666337067,
0.238043395288999));
#51117=CARTESIAN_POINT('Ctrl Pts',(0.194043790355372,0.113894720793023,
0.235));
#51118=CARTESIAN_POINT('Origin',(0.218008688022331,0.0793486732515551,0.04));
#51119=CARTESIAN_POINT('',(0.210873439877438,0.0784690534813352,0.04));
#51120=CARTESIAN_POINT('',(0.211977362141128,0.0754360519890136,0.04));
#51121=CARTESIAN_POINT('Origin',(0.,0.,0.04));
#51122=CARTESIAN_POINT('',(0.205792683952114,0.0749024113883215,0.04));
#51123=CARTESIAN_POINT('',(0.227830551089268,0.0903727834602902,0.04));
#51124=CARTESIAN_POINT('',(0.205792683952114,0.0749024113883215,0.04));
#51125=CARTESIAN_POINT('Origin',(0.205792683952114,0.0749024113883215,0.04));
#51126=CARTESIAN_POINT('',(0.211977362141128,0.0754360519890136,0.235));
#51127=CARTESIAN_POINT('',(0.211977362141128,0.0754360519890136,0.1175));
#51128=CARTESIAN_POINT('',(0.205792683952114,0.0749024113883215,0.241));
#51129=CARTESIAN_POINT('',(0.205792683952114,0.0749024113883215,0.04));
#51130=CARTESIAN_POINT('Ctrl Pts',(0.211977362141128,0.0754360519890136,
0.235));
#51131=CARTESIAN_POINT('Ctrl Pts',(0.208843234680406,0.0751656260089268,
0.238043395289026));
#51132=CARTESIAN_POINT('Ctrl Pts',(0.205792683952114,0.0749024113883215,
0.241));
#51133=CARTESIAN_POINT('Origin',(0.227830551089268,0.0903727834602902,0.04));
#51134=CARTESIAN_POINT('',(0.210873439877438,0.0784690534813352,0.235));
#51135=CARTESIAN_POINT('',(0.210873439877438,0.0784690534813352,0.1175));
#51136=CARTESIAN_POINT('Ctrl Pts',(0.205792683952114,0.0749024113883215,
0.241));
#51137=CARTESIAN_POINT('Ctrl Pts',(0.208298732482853,0.0766616335017707,
0.23804339528895));
#51138=CARTESIAN_POINT('Ctrl Pts',(0.210873439877438,0.0784690534813352,
0.235));
#51139=CARTESIAN_POINT('Origin',(0.228475398698832,0.0402863772187278,0.04));
#51140=CARTESIAN_POINT('',(0.221295806635937,0.0406591436868745,0.04));
#51141=CARTESIAN_POINT('',(0.221856282657939,0.0374805262129628,0.04));
#51142=CARTESIAN_POINT('Origin',(0.,0.,0.04));
#51143=CARTESIAN_POINT('',(0.215672897909674,0.0380289509090578,0.04));
#51144=CARTESIAN_POINT('',(0.240062362244323,0.0494374577994834,0.04));
#51145=CARTESIAN_POINT('',(0.215672897909674,0.0380289509090578,0.04));
#51146=CARTESIAN_POINT('Origin',(0.215672897909674,0.0380289509090578,0.04));
#51147=CARTESIAN_POINT('',(0.221856282657939,0.0374805262129628,0.235));
#51148=CARTESIAN_POINT('',(0.221856282657939,0.0374805262129628,0.1175));
#51149=CARTESIAN_POINT('',(0.215672897909674,0.0380289509090578,0.241));
#51150=CARTESIAN_POINT('',(0.215672897909674,0.0380289509090578,0.04));
#51151=CARTESIAN_POINT('Ctrl Pts',(0.221856282657939,0.0374805262129628,
0.235));
#51152=CARTESIAN_POINT('Ctrl Pts',(0.218722810657102,0.0377584441332836,
0.238043395288982));
#51153=CARTESIAN_POINT('Ctrl Pts',(0.215672897909674,0.0380289509090578,
0.241));
#51154=CARTESIAN_POINT('Origin',(0.240062362244323,0.0494374577994834,0.04));
#51155=CARTESIAN_POINT('',(0.221295806635937,0.0406591436868745,0.235));
#51156=CARTESIAN_POINT('',(0.221295806635937,0.0406591436868745,0.1175));
#51157=CARTESIAN_POINT('Ctrl Pts',(0.215672897909674,0.0380289509090578,
0.241));
#51158=CARTESIAN_POINT('Ctrl Pts',(0.218446359646296,0.0393262757251521,
0.238043395288935));
#51159=CARTESIAN_POINT('Ctrl Pts',(0.221295806635937,0.0406591436868745,
0.235));
#51160=CARTESIAN_POINT('Origin',(0.,0.,0.1175));
#51161=CARTESIAN_POINT('Origin',(0.,0.,0.235));
#51162=CARTESIAN_POINT('Origin',(0.,0.,0.235));
#51163=CARTESIAN_POINT('Origin',(0.,0.,0.235));
#51164=CARTESIAN_POINT('Origin',(0.,0.,0.235));
#51165=CARTESIAN_POINT('Origin',(0.,0.,0.235));
#51166=CARTESIAN_POINT('Origin',(0.,0.,0.235));
#51167=CARTESIAN_POINT('Origin',(0.,0.,0.235));
#51168=CARTESIAN_POINT('Origin',(0.,0.,0.235));
#51169=CARTESIAN_POINT('Origin',(0.,0.,0.235));
#51170=CARTESIAN_POINT('Origin',(0.,0.,0.235));
#51171=CARTESIAN_POINT('Origin',(0.,0.,0.235));
#51172=CARTESIAN_POINT('Origin',(0.,0.,0.235));
#51173=CARTESIAN_POINT('Origin',(0.,0.,0.235));
#51174=CARTESIAN_POINT('Origin',(0.,0.,0.235));
#51175=CARTESIAN_POINT('Origin',(0.,0.,0.235));
#51176=CARTESIAN_POINT('Origin',(0.,0.,0.235));
#51177=CARTESIAN_POINT('Origin',(0.,0.,0.235));
#51178=CARTESIAN_POINT('',(-0.225,-2.75545529808154E-17,1.38777878078145E-17));
#51179=CARTESIAN_POINT('',(-0.225,-2.75545529808154E-17,0.1175));
#51180=CARTESIAN_POINT('Origin',(0.,0.,0.));
#51181=CARTESIAN_POINT('Origin',(0.,0.,0.235));
#51182=CARTESIAN_POINT('Origin',(0.,0.,0.235));
#51183=CARTESIAN_POINT('Origin',(0.,0.,0.235));
#51184=CARTESIAN_POINT('Origin',(0.,0.,0.235));
#51185=CARTESIAN_POINT('Origin',(0.,0.,0.235));
#51186=CARTESIAN_POINT('Origin',(0.,0.,0.235));
#51187=CARTESIAN_POINT('Origin',(0.,0.,0.235));
#51188=CARTESIAN_POINT('Origin',(0.,0.,0.235));
#51189=CARTESIAN_POINT('Origin',(0.,0.,0.235));
#51190=CARTESIAN_POINT('Origin',(0.,0.,0.235));
#51191=CARTESIAN_POINT('Origin',(0.,0.,0.235));
#51192=CARTESIAN_POINT('Origin',(0.,0.,0.235));
#51193=CARTESIAN_POINT('Origin',(0.,0.,0.235));
#51194=CARTESIAN_POINT('Origin',(0.,0.,0.235));
#51195=CARTESIAN_POINT('Origin',(0.,0.,0.235));
#51196=CARTESIAN_POINT('Origin',(0.,0.,0.235));
#51197=CARTESIAN_POINT('Origin',(0.,0.,0.235));
#51198=CARTESIAN_POINT('',(0.224994212290885,0.0016138263860075,0.235));
#51199=CARTESIAN_POINT('Origin',(0.,0.,0.235));
#51200=CARTESIAN_POINT('',(0.224994212290885,0.0016138263860075,0.04));
#51201=CARTESIAN_POINT('',(0.224994212290885,0.0016138263860075,0.1175));
#51202=CARTESIAN_POINT('',(0.224994212290885,-0.0016138263860075,0.04));
#51203=CARTESIAN_POINT('Origin',(0.,0.,0.04));
#51204=CARTESIAN_POINT('',(0.224994212290885,-0.0016138263860075,0.235));
#51205=CARTESIAN_POINT('',(0.224994212290885,-0.0016138263860075,0.1175));
#51206=CARTESIAN_POINT('Origin',(0.,0.,0.235));
#51207=CARTESIAN_POINT('Origin',(0.219,0.,0.04));
#51208=CARTESIAN_POINT('',(0.219,0.,0.04));
#51209=CARTESIAN_POINT('',(0.219,0.,0.04));
#51210=CARTESIAN_POINT('',(0.219,0.,0.241));
#51211=CARTESIAN_POINT('',(0.219,0.,0.04));
#51212=CARTESIAN_POINT('Ctrl Pts',(0.224994212290885,-0.0016138263860075,
0.235));
#51213=CARTESIAN_POINT('Ctrl Pts',(0.221956604710985,-0.000796008960649803,
0.238043395289015));
#51214=CARTESIAN_POINT('Ctrl Pts',(0.219,0.,0.241));
#51215=CARTESIAN_POINT('Origin',(0.245,0.007,0.04));
#51216=CARTESIAN_POINT('Ctrl Pts',(0.219,0.,0.241));
#51217=CARTESIAN_POINT('Ctrl Pts',(0.221956604710993,0.00079600896065191,
0.238043395289007));
#51218=CARTESIAN_POINT('Ctrl Pts',(0.224994212290885,0.00161382638600749,
0.235));
#51219=CARTESIAN_POINT('',(0.245,0.007,0.04));
#51220=CARTESIAN_POINT('Origin',(0.232,0.,0.04));
#51221=CARTESIAN_POINT('Origin',(0.,0.,0.2425));
#51222=CARTESIAN_POINT('',(-0.21,-2.57175827820944E-17,0.25));
#51223=CARTESIAN_POINT('Origin',(0.,0.,0.25));
#51224=CARTESIAN_POINT('',(-0.2175,-2.66360678814549E-17,0.2425));
#51225=CARTESIAN_POINT('Origin',(0.,0.,0.111632486540519));
#51226=CARTESIAN_POINT('',(0.,0.,0.0822649730810374));
#51227=CARTESIAN_POINT('',(-0.0908032840555568,1.11201951170706E-17,0.14));
#51228=CARTESIAN_POINT('',(-0.0461880215351701,-5.6564012731995E-18,0.111632486540519));
#51229=CARTESIAN_POINT('Origin',(0.,0.,0.14));
#51230=CARTESIAN_POINT('Origin',(1.38777878078145E-17,0.115470053837925,
0.25));
#51231=CARTESIAN_POINT('',(7.07050159149938E-18,0.115470053837925,0.25));
#51232=CARTESIAN_POINT('',(0.1,0.0577350269189626,0.25));
#51233=CARTESIAN_POINT('',(0.025,0.101036297108185,0.25));
#51234=CARTESIAN_POINT('',(1.38777878078145E-17,0.115470053837925,0.14));
#51235=CARTESIAN_POINT('',(7.07050159149938E-18,0.115470053837925,0.25));
#51236=CARTESIAN_POINT('',(0.1,0.0577350269189626,0.14));
#51237=CARTESIAN_POINT('',(0.1,0.0577350269189626,0.14));
#51238=CARTESIAN_POINT('',(0.1,0.0577350269189626,0.25));
#51239=CARTESIAN_POINT('Origin',(-0.1,0.0577350269189626,0.25));
#51240=CARTESIAN_POINT('',(-0.1,0.0577350269189626,0.25));
#51241=CARTESIAN_POINT('',(-0.075,0.0721687836487032,0.25));
#51242=CARTESIAN_POINT('',(-0.1,0.0577350269189626,0.14));
#51243=CARTESIAN_POINT('',(-0.1,0.0577350269189626,0.25));
#51244=CARTESIAN_POINT('',(7.07050159149938E-18,0.115470053837925,0.14));
#51245=CARTESIAN_POINT('Origin',(-0.1,-0.0577350269189626,0.25));
#51246=CARTESIAN_POINT('',(-0.1,-0.0577350269189626,0.25));
#51247=CARTESIAN_POINT('',(-0.1,-0.0288675134594813,0.25));
#51248=CARTESIAN_POINT('',(-0.1,-0.0577350269189626,0.14));
#51249=CARTESIAN_POINT('',(-0.1,-0.0577350269189626,0.25));
#51250=CARTESIAN_POINT('',(-0.1,0.0577350269189626,0.14));
#51251=CARTESIAN_POINT('Origin',(-2.77555756156289E-17,-0.115470053837925,
0.25));
#51252=CARTESIAN_POINT('',(-2.12115047744981E-17,-0.115470053837925,0.25));
#51253=CARTESIAN_POINT('',(-0.025,-0.101036297108185,0.25));
#51254=CARTESIAN_POINT('',(-2.77555756156289E-17,-0.115470053837925,0.14));
#51255=CARTESIAN_POINT('',(-2.12115047744981E-17,-0.115470053837925,0.25));
#51256=CARTESIAN_POINT('',(-0.1,-0.0577350269189626,0.14));
#51257=CARTESIAN_POINT('Origin',(0.1,-0.0577350269189626,0.25));
#51258=CARTESIAN_POINT('',(0.1,-0.0577350269189626,0.25));
#51259=CARTESIAN_POINT('',(0.075,-0.0721687836487033,0.25));
#51260=CARTESIAN_POINT('',(0.1,-0.0577350269189626,0.14));
#51261=CARTESIAN_POINT('',(0.1,-0.0577350269189626,0.25));
#51262=CARTESIAN_POINT('',(-2.12115047744981E-17,-0.115470053837925,0.14));
#51263=CARTESIAN_POINT('Origin',(0.1,0.0577350269189626,0.25));
#51264=CARTESIAN_POINT('',(0.1,0.0288675134594813,0.25));
#51265=CARTESIAN_POINT('',(0.1,-0.0577350269189626,0.14));
#51266=CARTESIAN_POINT('Origin',(0.,0.,0.14));
#51267=CARTESIAN_POINT('Origin',(0.095,0.,-0.6));
#51268=CARTESIAN_POINT('',(-0.095,-1.16341445918999E-17,-0.6));
#51269=CARTESIAN_POINT('Origin',(0.,0.,-0.6));
#51270=CARTESIAN_POINT('Origin',(0.,0.,-0.585));
#51271=CARTESIAN_POINT('',(-0.11,-1.34711147906209E-17,-0.585));
#51272=CARTESIAN_POINT('Origin',(0.,0.,-0.005));
#51273=CARTESIAN_POINT('',(-0.135,-1.65327317884893E-17,0.));
#51274=CARTESIAN_POINT('Origin',(0.,0.,0.));
#51275=CARTESIAN_POINT('',(-0.13,-1.59204083889156E-17,-0.005));
#51276=CARTESIAN_POINT('Origin',(0.225,0.,0.));
#51277=CARTESIAN_POINT('Origin',(0.,0.,0.25));
#51278=CARTESIAN_POINT('',(0.,0.,0.));
#51279=CARTESIAN_POINT('Origin',(0.,0.,-0.1404));
#51280=CARTESIAN_POINT('',(-0.0769107559639177,6.92925783995872E-5,-0.237610382907248));
#51281=CARTESIAN_POINT('',(-0.0768920912054452,6.13296515658117E-5,-0.242639617092752));
#51282=CARTESIAN_POINT('',(-0.076925,-9.42059550244101E-18,-0.1404));
#51283=CARTESIAN_POINT('',(0.0402078774433248,-0.0657264351496036,-0.2608));
#51284=CARTESIAN_POINT('Ctrl Pts',(-0.0769107559639177,6.92925783995872E-5,
-0.237610382907248));
#51285=CARTESIAN_POINT('Ctrl Pts',(-0.0769685167490698,0.00645933324294077,
-0.238073052764717));
#51286=CARTESIAN_POINT('Ctrl Pts',(-0.0762388107008733,0.0128364434973379,
-0.238535722622186));
#51287=CARTESIAN_POINT('Ctrl Pts',(-0.074670594402015,0.019000293291529,
-0.238998392479655));
#51288=CARTESIAN_POINT('Ctrl Pts',(-0.0683908780681301,0.0436826207615176,
-0.240851093196551));
#51289=CARTESIAN_POINT('Ctrl Pts',(-0.0486656758144597,0.0649453233519243,
-0.242703793913448));
#51290=CARTESIAN_POINT('Ctrl Pts',(-0.0245197323996812,0.0730479175280928,
-0.244556494630344));
#51291=CARTESIAN_POINT('Ctrl Pts',(-0.000373788984902864,0.0811505117042614,
-0.246409195347241));
#51292=CARTESIAN_POINT('Ctrl Pts',(0.0281928955909835,0.0760929974661918,
-0.248261896064137));
#51293=CARTESIAN_POINT('Ctrl Pts',(0.0480896295923508,0.0602015617017921,
-0.250114596781034));
#51294=CARTESIAN_POINT('Ctrl Pts',(0.0679863635937181,0.0443101259373923,
-0.25196729749793));
#51295=CARTESIAN_POINT('Ctrl Pts',(0.0792131470205665,0.0175847686466624,
-0.253819998214827));
#51296=CARTESIAN_POINT('Ctrl Pts',(0.0766524840100219,-0.00775899280922349,
-0.255672698931724));
#51297=CARTESIAN_POINT('Ctrl Pts',(0.0742902945731415,-0.0311383931267909,
-0.257381799287816));
#51298=CARTESIAN_POINT('Ctrl Pts',(0.0601951224862113,-0.0533420688434893,
-0.259090899643908));
#51299=CARTESIAN_POINT('Ctrl Pts',(0.0402078774433248,-0.0657264351496036,
-0.2608));
#51300=CARTESIAN_POINT('',(-0.076925,-9.42059550244101E-18,-0.2608));
#51301=CARTESIAN_POINT('Origin',(0.,0.,-0.2608));
#51302=CARTESIAN_POINT('',(-0.076925,-9.42059550244101E-18,-0.283875));
#51303=CARTESIAN_POINT('',(-0.076925,-9.42059550244101E-18,-0.1404));
#51304=CARTESIAN_POINT('Origin',(0.,0.,-0.283875));
#51305=CARTESIAN_POINT('',(0.0763850617480247,-0.00909823976109922,-0.2608));
#51306=CARTESIAN_POINT('Origin',(0.,0.,-0.2608));
#51307=CARTESIAN_POINT('Ctrl Pts',(0.0763850617480247,-0.00909823976109917,
-0.2608));
#51308=CARTESIAN_POINT('Ctrl Pts',(0.0794111003994919,0.0163071304328721,
-0.258947299283103));
#51309=CARTESIAN_POINT('Ctrl Pts',(0.0687417228149469,0.0431206585224096,
-0.257094598566207));
#51310=CARTESIAN_POINT('Ctrl Pts',(0.0491529311664505,0.0593298637717059,
-0.25524189784931));
#51311=CARTESIAN_POINT('Ctrl Pts',(0.029564139517954,0.0755390690210024,
-0.253389197132414));
#51312=CARTESIAN_POINT('Ctrl Pts',(0.00105593380550616,0.0811439514300577,
-0.251536496415517));
#51313=CARTESIAN_POINT('Ctrl Pts',(-0.0232378405355734,0.0734789981937897,
-0.249683795698621));
#51314=CARTESIAN_POINT('Ctrl Pts',(-0.0475316148766529,0.0658140449575217,
-0.247831094981724));
#51315=CARTESIAN_POINT('Ctrl Pts',(-0.0676109578463641,0.0448792560759306,
-0.245978394264828));
#51316=CARTESIAN_POINT('Ctrl Pts',(-0.0743200843287782,0.0203058807031412,
-0.244125693547931));
#51317=CARTESIAN_POINT('Ctrl Pts',(-0.0761139115435399,0.0137356677823074,
-0.243630334729538));
#51318=CARTESIAN_POINT('Ctrl Pts',(-0.0769519372805849,0.00690534191951837,
-0.243134975911145));
#51319=CARTESIAN_POINT('Ctrl Pts',(-0.0768920912054452,6.13296515658117E-5,
-0.242639617092752));
#51320=CARTESIAN_POINT('Origin',(0.,0.,-0.1404));
#51321=CARTESIAN_POINT('',(-0.0768031572226018,-1.95264706120274E-5,-0.202610382907248));
#51322=CARTESIAN_POINT('',(-0.076807157253071,-2.66424230989696E-5,-0.207639617092752));
#51323=CARTESIAN_POINT('',(-0.076925,-9.42059550244101E-18,-0.1404));
#51324=CARTESIAN_POINT('Ctrl Pts',(-0.0768031572226018,-1.95264706120274E-5,
-0.202610382907248));
#51325=CARTESIAN_POINT('Ctrl Pts',(-0.0767712748932385,0.0140231988469081,
-0.203623515130004));
#51326=CARTESIAN_POINT('Ctrl Pts',(-0.0730908430886916,0.0280814791033811,
-0.20463664735276));
#51327=CARTESIAN_POINT('Ctrl Pts',(-0.0658633246280591,0.0399862919354661,
-0.205649779575517));
#51328=CARTESIAN_POINT('Ctrl Pts',(-0.0526464627687379,0.0617564565527937,
-0.207502480292413));
#51329=CARTESIAN_POINT('Ctrl Pts',(-0.0275678150095582,0.0763252268972791,
-0.20935518100931));
#51330=CARTESIAN_POINT('Ctrl Pts',(-0.00210920191325928,0.0770223484917919,
-0.211207881726206));
#51331=CARTESIAN_POINT('Ctrl Pts',(0.0233494111830397,0.0777194700863047,
-0.213060582443103));
#51332=CARTESIAN_POINT('Ctrl Pts',(0.0491879896164579,0.0645449429308449,
-0.214913283159999));
#51333=CARTESIAN_POINT('Ctrl Pts',(0.0635764027686449,0.0435307922368906,
-0.216765983876896));
#51334=CARTESIAN_POINT('Ctrl Pts',(0.0779648159208319,0.0225166415429363,
-0.218618684593793));
#51335=CARTESIAN_POINT('Ctrl Pts',(0.0809030637917877,-0.00633713268951243,
-0.220471385310689));
#51336=CARTESIAN_POINT('Ctrl Pts',(0.0710463837048955,-0.0298206145785707,
-0.222324086027586));
#51337=CARTESIAN_POINT('Ctrl Pts',(0.0611897036180032,-0.0533040964676289,
-0.224176786744482));
#51338=CARTESIAN_POINT('Ctrl Pts',(0.038538095573263,-0.0714172860132967,
-0.226029487461379));
#51339=CARTESIAN_POINT('Ctrl Pts',(0.0134614150354561,-0.0758664580059033,
-0.227882188178275));
#51340=CARTESIAN_POINT('Ctrl Pts',(-0.0116152655023509,-0.0803156299985098,
-0.229734888895172));
#51341=CARTESIAN_POINT('Ctrl Pts',(-0.0391170185332245,-0.0711007844380552,
-0.231587589612069));
#51342=CARTESIAN_POINT('Ctrl Pts',(-0.0564507798416117,-0.0524423854830426,
-0.233440290328965));
#51343=CARTESIAN_POINT('Ctrl Pts',(-0.0694558285841694,-0.038443497212289,
-0.234830321188393));
#51344=CARTESIAN_POINT('Ctrl Pts',(-0.076737221266271,-0.0191287458788749,
-0.23622035204782));
#51345=CARTESIAN_POINT('Ctrl Pts',(-0.0769107559639177,6.92925783995872E-5,
-0.237610382907248));
#51346=CARTESIAN_POINT('Ctrl Pts',(-0.0768920912054452,6.13296515658117E-5,
-0.242639617092752));
#51347=CARTESIAN_POINT('Ctrl Pts',(-0.0767281058634428,-0.018692075476664,
-0.241282275194248));
#51348=CARTESIAN_POINT('Ctrl Pts',(-0.0698226746732161,-0.0375482415536338,
-0.239924933295745));
#51349=CARTESIAN_POINT('Ctrl Pts',(-0.0573676133020383,-0.0514373135287137,
-0.238567591397241));
#51350=CARTESIAN_POINT('Ctrl Pts',(-0.0403671057977673,-0.0703951705237914,
-0.236714890680345));
#51351=CARTESIAN_POINT('Ctrl Pts',(-0.0130271807941084,-0.0800989226499592,
-0.234862189963448));
#51352=CARTESIAN_POINT('Ctrl Pts',(0.0121250371607425,-0.0760933557253033,
-0.233009489246552));
#51353=CARTESIAN_POINT('Ctrl Pts',(0.0372772551155935,-0.0720877888006474,
-0.231156788529655));
#51354=CARTESIAN_POINT('Ctrl Pts',(0.0602417660216363,-0.0543729028251678,
-0.229304087812759));
#51355=CARTESIAN_POINT('Ctrl Pts',(0.070509742362668,-0.0310658065448274,
-0.227451387095862));
#51356=CARTESIAN_POINT('Ctrl Pts',(0.0807777187036996,-0.00775871026448711,
-0.225598686378965));
#51357=CARTESIAN_POINT('Ctrl Pts',(0.0783491604797202,0.0211405963207139,
-0.223745985662069));
#51358=CARTESIAN_POINT('Ctrl Pts',(0.0643332164174167,0.0424043769590272,
-0.221893284945172));
#51359=CARTESIAN_POINT('Ctrl Pts',(0.0503172723551132,0.0636681575973404,
-0.220040584228276));
#51360=CARTESIAN_POINT('Ctrl Pts',(0.0247139424544857,0.0772964122887658,
-0.218187883511379));
#51361=CARTESIAN_POINT('Ctrl Pts',(-0.000753157637863402,0.0770477869535545,
-0.216335182794483));
#51362=CARTESIAN_POINT('Ctrl Pts',(-0.0262202577302126,0.0767991616183431,
-0.214482482077586));
#51363=CARTESIAN_POINT('Ctrl Pts',(-0.0515511280142834,0.0626736562564949,
-0.21262978136069));
#51364=CARTESIAN_POINT('Ctrl Pts',(-0.0651490986593925,0.0411394228871772,
-0.210777080643793));
#51365=CARTESIAN_POINT('Ctrl Pts',(-0.072824944858416,0.0289836779109062,
-0.209731259460113));
#51366=CARTESIAN_POINT('Ctrl Pts',(-0.0767621851696059,0.014467193901455,
-0.208685438276432));
#51367=CARTESIAN_POINT('Ctrl Pts',(-0.076807157253071,-2.66424230989696E-5,
-0.207639617092752));
#51368=CARTESIAN_POINT('Origin',(0.,0.,-0.1404));
#51369=CARTESIAN_POINT('',(-0.0769835019150157,-6.04666404582025E-5,-0.167610382907248));
#51370=CARTESIAN_POINT('',(-0.0769958967773298,-5.59803197837138E-5,-0.172639617092752));
#51371=CARTESIAN_POINT('',(-0.076925,-9.42059550244101E-18,-0.1404));
#51372=CARTESIAN_POINT('Ctrl Pts',(-0.0769835019150157,-6.04666404582025E-5,
-0.167610382907248));
#51373=CARTESIAN_POINT('Ctrl Pts',(-0.0767976431805962,0.0214832714064119,
-0.169173977495292));
#51374=CARTESIAN_POINT('Ctrl Pts',(-0.0673441366562592,0.0431699129578856,
-0.170737572083335));
#51375=CARTESIAN_POINT('Ctrl Pts',(-0.0513089165162116,0.0574828694067931,
-0.172301166671379));
#51376=CARTESIAN_POINT('Ctrl Pts',(-0.0323088099180996,0.0744422685225056,
-0.174153867388276));
#51377=CARTESIAN_POINT('Ctrl Pts',(-0.00406808136104573,0.0810491302208425,
-0.176006568105172));
#51378=CARTESIAN_POINT('Ctrl Pts',(0.0204835983469324,0.0742785807479444,
-0.177859268822069));
#51379=CARTESIAN_POINT('Ctrl Pts',(0.0450352780549104,0.0675080312750463,
-0.179711969538965));
#51380=CARTESIAN_POINT('Ctrl Pts',(0.0658979089138128,0.0473600706309135,
-0.181564670255862));
#51381=CARTESIAN_POINT('Ctrl Pts',(0.073519784037494,0.0230592021375661,
-0.183417370972758));
#51382=CARTESIAN_POINT('Ctrl Pts',(0.0811416591611752,-0.00124166635578134,
-0.185270071689655));
#51383=CARTESIAN_POINT('Ctrl Pts',(0.0755227785496352,-0.0296954426983434,
-0.187122772406551));
#51384=CARTESIAN_POINT('Ctrl Pts',(0.0592356885267185,-0.0492749211921189,
-0.188975473123448));
#51385=CARTESIAN_POINT('Ctrl Pts',(0.0429485985038016,-0.0688543996858945,
-0.190828173840344));
#51386=CARTESIAN_POINT('Ctrl Pts',(0.015993299069508,-0.0795595803308835,
-0.192680874557241));
#51387=CARTESIAN_POINT('Ctrl Pts',(-0.00928907365455888,-0.0764892089010994,
-0.194533575274138));
#51388=CARTESIAN_POINT('Ctrl Pts',(-0.0345714463786257,-0.0734188374713153,
-0.196386275991034));
#51389=CARTESIAN_POINT('Ctrl Pts',(-0.0581808923924657,-0.0565729139667582,
-0.198238976707931));
#51390=CARTESIAN_POINT('Ctrl Pts',(-0.0693080774196544,-0.0336641727693947,
-0.200091677424827));
#51391=CARTESIAN_POINT('Ctrl Pts',(-0.074350464402127,-0.0232828644586075,
-0.200931245918967));
#51392=CARTESIAN_POINT('Ctrl Pts',(-0.0768295776627497,-0.0116565364122966,
-0.201770814413108));
#51393=CARTESIAN_POINT('Ctrl Pts',(-0.0768031572226018,-1.95264706120274E-5,
-0.202610382907248));
#51394=CARTESIAN_POINT('Ctrl Pts',(-0.076807157253071,-2.66424230989696E-5,
-0.207639617092752));
#51395=CARTESIAN_POINT('Ctrl Pts',(-0.0768418544405828,-0.0112090319850631,
-0.206832737559536));
#51396=CARTESIAN_POINT('Ctrl Pts',(-0.0745596622880536,-0.022377940415552,
-0.20602585802632));
#51397=CARTESIAN_POINT('Ctrl Pts',(-0.0698900106134843,-0.0324387856940936,
-0.205218978493103));
#51398=CARTESIAN_POINT('Ctrl Pts',(-0.0591678809163199,-0.0555397995292589,
-0.203366277776207));
#51399=CARTESIAN_POINT('Ctrl Pts',(-0.035858550515844,-0.0727988658228025,
-0.20151357705931));
#51400=CARTESIAN_POINT('Ctrl Pts',(-0.010634123895685,-0.0763138640352252,
-0.199660876342414));
#51401=CARTESIAN_POINT('Ctrl Pts',(0.0145903027244741,-0.079828862247648,
-0.197808175625517));
#51402=CARTESIAN_POINT('Ctrl Pts',(0.0417298255643163,-0.06959979237895,
-0.195955474908621));
#51403=CARTESIAN_POINT('Ctrl Pts',(0.0583590560517694,-0.05031005037711,
-0.194102774191724));
#51404=CARTESIAN_POINT('Ctrl Pts',(0.0749882865392224,-0.03102030837527,
-0.192250073474828));
#51405=CARTESIAN_POINT('Ctrl Pts',(0.0811072246742864,-0.00266989424028812,
-0.190397372757931));
#51406=CARTESIAN_POINT('Ctrl Pts',(0.073914330385439,0.0217613744332338,
-0.188544672041035));
#51407=CARTESIAN_POINT('Ctrl Pts',(0.0667214360965916,0.0461926431067557,
-0.186691971324138));
#51408=CARTESIAN_POINT('Ctrl Pts',(0.0462167093838328,0.0667047663188176,
-0.184839270607242));
#51409=CARTESIAN_POINT('Ctrl Pts',(0.0217880206488223,0.0739064790943958,
-0.182986569890345));
#51410=CARTESIAN_POINT('Ctrl Pts',(-0.00264066808618824,0.0811081918699739,
-0.181133869173448));
#51411=CARTESIAN_POINT('Ctrl Pts',(-0.0309933188434504,0.0749994942090683,
-0.179281168456552));
#51412=CARTESIAN_POINT('Ctrl Pts',(-0.0502890320799736,0.0583771995879325,
-0.177428467739655));
#51413=CARTESIAN_POINT('Ctrl Pts',(-0.066914183311445,0.0440554609456219,
-0.175832184190688));
#51414=CARTESIAN_POINT('Ctrl Pts',(-0.0768159042207944,0.0219289387950761,
-0.17423590064172));
#51415=CARTESIAN_POINT('Ctrl Pts',(-0.0769958967773298,-5.59803197837138E-5,
-0.172639617092752));
#51416=CARTESIAN_POINT('Origin',(0.,0.,-0.1404));
#51417=CARTESIAN_POINT('',(-0.0769940708635155,5.67089128405991E-5,-0.132610382907248));
#51418=CARTESIAN_POINT('',(-0.0769815700716422,6.10755343289724E-5,-0.137639617092752));
#51419=CARTESIAN_POINT('',(-0.076925,-9.42059550244101E-18,-0.1404));
#51420=CARTESIAN_POINT('Ctrl Pts',(-0.0769940708635155,5.67089128405991E-5,
-0.132610382907248));
#51421=CARTESIAN_POINT('Ctrl Pts',(-0.0770238103898011,0.00365647805096637,
-0.132871739143682));
#51422=CARTESIAN_POINT('Ctrl Pts',(-0.0767931990646562,0.0072524177611427,
-0.133133095380117));
#51423=CARTESIAN_POINT('Ctrl Pts',(-0.0762891701184668,0.0108096161986601,
-0.133394451616551));
#51424=CARTESIAN_POINT('Ctrl Pts',(-0.0727162123705239,0.0360258658096909,
-0.135247152333448));
#51425=CARTESIAN_POINT('Ctrl Pts',(-0.0554037427351246,0.0592953273015094,
-0.137099853050345));
#51426=CARTESIAN_POINT('Ctrl Pts',(-0.0322780646014716,0.0699643611084238,
-0.138952553767241));
#51427=CARTESIAN_POINT('Ctrl Pts',(-0.00915238646781869,0.0806333949153382,
-0.140805254484138));
#51428=CARTESIAN_POINT('Ctrl Pts',(0.0197865001640878,0.0787020010373485,
-0.142657955201034));
#51429=CARTESIAN_POINT('Ctrl Pts',(0.0412892785043032,0.065054444597746,
-0.144510655917931));
#51430=CARTESIAN_POINT('Ctrl Pts',(0.0627920568445187,0.0514068881581433,
-0.146363356634827));
#51431=CARTESIAN_POINT('Ctrl Pts',(0.0768587268930429,0.0260431691569276,
-0.148216057351724));
#51432=CARTESIAN_POINT('Ctrl Pts',(0.0770490349640221,0.000575757562533098,
-0.15006875806862));
#51433=CARTESIAN_POINT('Ctrl Pts',(0.0772393430350013,-0.0248916540318611,
-0.151921458785517));
#51434=CARTESIAN_POINT('Ctrl Pts',(0.0635532891284355,-0.0504627582194342,
-0.153774159502413));
#51435=CARTESIAN_POINT('Ctrl Pts',(0.0422568665736587,-0.0644301365446651,
-0.15562686021931));
#51436=CARTESIAN_POINT('Ctrl Pts',(0.0209604440188819,-0.078397514869896,
-0.157479560936207));
#51437=CARTESIAN_POINT('Ctrl Pts',(-0.00794634718410591,-0.0807611673327848,
-0.159332261653103));
#51438=CARTESIAN_POINT('Ctrl Pts',(-0.0312288851198616,-0.0704389240607994,
-0.16118496237));
#51439=CARTESIAN_POINT('Ctrl Pts',(-0.0545114230556172,-0.0601166807888141,
-0.163037663086896));
#51440=CARTESIAN_POINT('Ctrl Pts',(-0.0721697077241406,-0.0371085417819546,
-0.164890363803793));
#51441=CARTESIAN_POINT('Ctrl Pts',(-0.0761191077388172,-0.0119485040119809,
-0.166743064520689));
#51442=CARTESIAN_POINT('Ctrl Pts',(-0.0767353949454457,-0.00802238628819954,
-0.167032170649542));
#51443=CARTESIAN_POINT('Ctrl Pts',(-0.0770178668965988,-0.00404386921512726,
-0.167321276778395));
#51444=CARTESIAN_POINT('Ctrl Pts',(-0.0769835019150157,-6.04666404582025E-5,
-0.167610382907248));
#51445=CARTESIAN_POINT('Ctrl Pts',(-0.0769958967773298,-5.59803197837138E-5,
-0.172639617092752));
#51446=CARTESIAN_POINT('Ctrl Pts',(-0.0770248096741801,-0.0035875024608357,
-0.172383199924823));
#51447=CARTESIAN_POINT('Ctrl Pts',(-0.0768028705500182,-0.00711537078577657,
-0.172126782756894));
#51448=CARTESIAN_POINT('Ctrl Pts',(-0.0763176518415591,-0.0106066485349346,
-0.171870365588966));
#51449=CARTESIAN_POINT('Ctrl Pts',(-0.0728117826508375,-0.0358323104552998,
-0.170017664872069));
#51450=CARTESIAN_POINT('Ctrl Pts',(-0.0555612685536102,-0.0591477427146643,
-0.168164964155173));
#51451=CARTESIAN_POINT('Ctrl Pts',(-0.0324640518946935,-0.0698782528471297,
-0.166312263438276));
#51452=CARTESIAN_POINT('Ctrl Pts',(-0.00936683523577665,-0.0806087629795951,
-0.16445956272138));
#51453=CARTESIAN_POINT('Ctrl Pts',(0.0195770839848297,-0.0787543509851614,
-0.162606862004483));
#51454=CARTESIAN_POINT('Ctrl Pts',(0.0411160872190435,-0.0651640398372977,
-0.160754161287586));
#51455=CARTESIAN_POINT('Ctrl Pts',(0.0626550904532573,-0.0515737286894341,
-0.15890146057069));
#51456=CARTESIAN_POINT('Ctrl Pts',(0.0767891777010786,-0.0262475183881405,
-0.157048759853793));
#51457=CARTESIAN_POINT('Ctrl Pts',(0.0770472279776439,-0.000780704307396157,
-0.155196059136897));
#51458=CARTESIAN_POINT('Ctrl Pts',(0.0773052782542091,0.0246861097733482,
-0.15334335842));
#51459=CARTESIAN_POINT('Ctrl Pts',(0.0636872915595182,0.0502935276335436,
-0.151490657703104));
#51460=CARTESIAN_POINT('Ctrl Pts',(0.0424280979279968,0.0643175040091825,
-0.149637956986207));
#51461=CARTESIAN_POINT('Ctrl Pts',(0.0211689042964752,0.0783414803848215,
-0.14778525626931));
#51462=CARTESIAN_POINT('Ctrl Pts',(-0.00773149627187655,0.080782015275904,
-0.145932555552414));
#51463=CARTESIAN_POINT('Ctrl Pts',(-0.0310414076692225,0.0705217399440169,
-0.144079854835518));
#51464=CARTESIAN_POINT('Ctrl Pts',(-0.0543513190665685,0.0602614646121299,
-0.142227154118621));
#51465=CARTESIAN_POINT('Ctrl Pts',(-0.0720707412929083,0.0373003790572733,
-0.140374453401724));
#51466=CARTESIAN_POINT('Ctrl Pts',(-0.0760870524860517,0.0121509364549594,
-0.138521752684828));
#51467=CARTESIAN_POINT('Ctrl Pts',(-0.0767244878832914,0.00815942679232915,
-0.138227707487469));
#51468=CARTESIAN_POINT('Ctrl Pts',(-0.0770167502794287,0.0041127937516773,
-0.137933662290111));
#51469=CARTESIAN_POINT('Ctrl Pts',(-0.0769815700716422,6.10755343289724E-5,
-0.137639617092752));
#51470=CARTESIAN_POINT('Origin',(0.,0.,-0.1404));
#51471=CARTESIAN_POINT('',(-0.0768065340016711,2.55117277794884E-5,-0.097610382907248));
#51472=CARTESIAN_POINT('',(-0.0768026632099214,1.84305570967413E-5,-0.102639617092752));
#51473=CARTESIAN_POINT('',(-0.076925,-9.42059550244101E-18,-0.1404));
#51474=CARTESIAN_POINT('Ctrl Pts',(-0.0768065340016711,2.55117277794884E-5,
-0.097610382907248));
#51475=CARTESIAN_POINT('Ctrl Pts',(-0.0768400025741158,0.0112766656092284,
-0.0984222015089698));
#51476=CARTESIAN_POINT('Ctrl Pts',(-0.0745285853311949,0.0225147292215057,
-0.0992340201106917));
#51477=CARTESIAN_POINT('Ctrl Pts',(-0.0698034168638814,0.0326246560661289,
-0.100045838712414));
#51478=CARTESIAN_POINT('Ctrl Pts',(-0.059019821873226,0.0556971363875672,
-0.10189853942931));
#51479=CARTESIAN_POINT('Ctrl Pts',(-0.0356647862302525,0.0728939886496841,
-0.103751240146207));
#51480=CARTESIAN_POINT('Ctrl Pts',(-0.0104311268550819,0.0763418424169287,
-0.105603940863103));
#51481=CARTESIAN_POINT('Ctrl Pts',(0.0148025325200884,0.0797896961841732,
-0.10745664158));
#51482=CARTESIAN_POINT('Ctrl Pts',(0.0419148156274558,0.0694885514565458,
-0.109309342296896));
#51483=CARTESIAN_POINT('Ctrl Pts',(0.0584926929014032,0.0501546624534022,
-0.111162043013793));
#51484=CARTESIAN_POINT('Ctrl Pts',(0.0750705701753508,0.0308207734502583,
-0.113014743730689));
#51485=CARTESIAN_POINT('Ctrl Pts',(0.0811140416158781,0.00245414017159807,
-0.114867444447586));
#51486=CARTESIAN_POINT('Ctrl Pts',(0.0738561779002024,-0.0219579200691195,
-0.116720145164483));
#51487=CARTESIAN_POINT('Ctrl Pts',(0.0665983141845268,-0.0463699803098367,
-0.118572845881379));
#51488=CARTESIAN_POINT('Ctrl Pts',(0.0460391153126481,-0.0668274675126116,
-0.120425546598276));
#51489=CARTESIAN_POINT('Ctrl Pts',(0.021591359872017,-0.0739641701402441,
-0.122278247315172));
#51490=CARTESIAN_POINT('Ctrl Pts',(-0.00285639556861437,-0.0811008727678766,
-0.124130948032069));
#51491=CARTESIAN_POINT('Ctrl Pts',(-0.0311927075779979,-0.074916790820367,
-0.125983648748965));
#51492=CARTESIAN_POINT('Ctrl Pts',(-0.0504441406524469,-0.0582432309814905,
-0.127836349465862));
#51493=CARTESIAN_POINT('Ctrl Pts',(-0.0669798182633061,-0.0439217719475156,
-0.129427693946324));
#51494=CARTESIAN_POINT('Ctrl Pts',(-0.0768129929919797,-0.0218615465190703,
-0.131019038426786));
#51495=CARTESIAN_POINT('Ctrl Pts',(-0.0769940708635155,5.67089128405991E-5,
-0.132610382907248));
#51496=CARTESIAN_POINT('Ctrl Pts',(-0.0769815700716422,6.10755343289724E-5,
-0.137639617092752));
#51497=CARTESIAN_POINT('Ctrl Pts',(-0.0767950891308295,-0.0214160069679987,
-0.136080961573214));
#51498=CARTESIAN_POINT('Ctrl Pts',(-0.0674081959306611,-0.0430359716776464,
-0.134522306053676));
#51499=CARTESIAN_POINT('Ctrl Pts',(-0.0514616363966927,-0.0573461837245798,
-0.132963650534138));
#51500=CARTESIAN_POINT('Ctrl Pts',(-0.0325067089542431,-0.0743560616520345,
-0.131110949817242));
#51501=CARTESIAN_POINT('Ctrl Pts',(-0.00428365390939655,-0.0810380178571733,
-0.129258249100345));
#51502=CARTESIAN_POINT('Ctrl Pts',(0.0202859467151432,-0.0743328001131744,
-0.127405548383449));
#51503=CARTESIAN_POINT('Ctrl Pts',(0.0448555473396833,-0.0676275823691754,
-0.125552847666552));
#51504=CARTESIAN_POINT('Ctrl Pts',(0.0657716935439163,-0.0475351906760383,
-0.123700146949655));
#51505=CARTESIAN_POINT('Ctrl Pts',(0.073458182507608,-0.0232546818828749,
-0.121847446232759));
#51506=CARTESIAN_POINT('Ctrl Pts',(0.0811446714712997,0.00102582691028839,
-0.119994745515862));
#51507=CARTESIAN_POINT('Ctrl Pts',(0.0756015031944501,0.0294944528034778,
-0.118142044798966));
#51508=CARTESIAN_POINT('Ctrl Pts',(0.0593665497202859,0.0491171821535752,
-0.116289344082069));
#51509=CARTESIAN_POINT('Ctrl Pts',(0.0431315962461219,0.0687399115036725,
-0.114436643365173));
#51510=CARTESIAN_POINT('Ctrl Pts',(0.016204857574643,0.0795167443106779,
-0.112583942648276));
#51511=CARTESIAN_POINT('Ctrl Pts',(-0.00908558679109352,0.076513638819554,
-0.11073124193138));
#51512=CARTESIAN_POINT('Ctrl Pts',(-0.0343760311568303,0.07351053332843,
-0.108878541214483));
#51513=CARTESIAN_POINT('Ctrl Pts',(-0.058030181216825,0.0567274895391765,
-0.107025840497587));
#51514=CARTESIAN_POINT('Ctrl Pts',(-0.0692182726444968,0.0338484198586954,
-0.10517313978069));
#51515=CARTESIAN_POINT('Ctrl Pts',(-0.0743180859797396,0.0234195647310118,
-0.104328632218044));
#51516=CARTESIAN_POINT('Ctrl Pts',(-0.0768277445635456,0.0117240983276437,
-0.103484124655398));
#51517=CARTESIAN_POINT('Ctrl Pts',(-0.0768026632099214,1.84305570967413E-5,
-0.102639617092752));
#51518=CARTESIAN_POINT('Origin',(0.,0.,-0.1404));
#51519=CARTESIAN_POINT('',(-0.0769006083194561,-6.96495813230711E-5,-0.062610382907248));
#51520=CARTESIAN_POINT('',(-0.0769139474189681,-7.03763467951925E-5,-0.0676396170927522));
#51521=CARTESIAN_POINT('',(-0.076925,-9.42059550244101E-18,-0.1404));
#51522=CARTESIAN_POINT('Ctrl Pts',(-0.0769006083194561,-6.96495813230711E-5,
-0.062610382907248));
#51523=CARTESIAN_POINT('Ctrl Pts',(-0.0767339796246602,0.0187523617936226,
-0.0639726638742573));
#51524=CARTESIAN_POINT('Ctrl Pts',(-0.069766977212752,0.0376847076479654,
-0.0653349448412665));
#51525=CARTESIAN_POINT('Ctrl Pts',(-0.0572276721267053,0.0515933582621614,
-0.0666972258082757));
#51526=CARTESIAN_POINT('Ctrl Pts',(-0.0401742300799402,0.0705091088217225,
-0.0685499265251723));
#51527=CARTESIAN_POINT('Ctrl Pts',(-0.0128142725637799,0.0801330466902033,
-0.0704026272420688));
#51528=CARTESIAN_POINT('Ctrl Pts',(0.0123258579767334,0.0760589202460425,
-0.0722553279589653));
#51529=CARTESIAN_POINT('Ctrl Pts',(0.037465988517247,0.0719847938018817,
-0.0741080286758619));
#51530=CARTESIAN_POINT('Ctrl Pts',(0.0603862920821135,0.0542126030450788,
-0.0759607293927584));
#51531=CARTESIAN_POINT('Ctrl Pts',(0.0705929441493049,0.0308791548460925,
-0.0778134301096549));
#51532=CARTESIAN_POINT('Ctrl Pts',(0.0807995962164963,0.0075457066471062,
-0.0796661308265515));
#51533=CARTESIAN_POINT('Ctrl Pts',(0.0782925967860125,-0.0213489989940634,
-0.0815188315434481));
#51534=CARTESIAN_POINT('Ctrl Pts',(0.064219767501604,-0.0425758865528817,
-0.0833715322603447));
#51535=CARTESIAN_POINT('Ctrl Pts',(0.0501469382171956,-0.0638027741116999,
-0.0852242329772412));
#51536=CARTESIAN_POINT('Ctrl Pts',(0.0245082790788626,-0.0773618435881669,
-0.0870769336941378));
#51537=CARTESIAN_POINT('Ctrl Pts',(-0.000957873902260806,-0.0770452329850995,
-0.0889296344110343));
#51538=CARTESIAN_POINT('Ctrl Pts',(-0.0264240268833843,-0.0767286223820321,
-0.0907823351279308));
#51539=CARTESIAN_POINT('Ctrl Pts',(-0.0517176737072984,-0.0625363316994301,
-0.0926350358448274));
#51540=CARTESIAN_POINT('Ctrl Pts',(-0.0652584199500865,-0.0409661321677492,
-0.0944877365617239));
#51541=CARTESIAN_POINT('Ctrl Pts',(-0.0728658659135372,-0.0288475882990529,
-0.0955286186768986));
#51542=CARTESIAN_POINT('Ctrl Pts',(-0.0767636219048009,-0.0144002784985585,
-0.0965695007920733));
#51543=CARTESIAN_POINT('Ctrl Pts',(-0.0768065340016711,2.55117277794884E-5,
-0.097610382907248));
#51544=CARTESIAN_POINT('Ctrl Pts',(-0.0768026632099214,1.84305570967413E-5,
-0.102639617092752));
#51545=CARTESIAN_POINT('Ctrl Pts',(-0.0767727204952061,-0.013956073206045,
-0.101631423938501));
#51546=CARTESIAN_POINT('Ctrl Pts',(-0.0731302282531401,-0.0279451161113039,
-0.100623230784251));
#51547=CARTESIAN_POINT('Ctrl Pts',(-0.0659694723256156,-0.0398109725683601,
-0.0996150376300002));
#51548=CARTESIAN_POINT('Ctrl Pts',(-0.0528105477837138,-0.0616161997432264,
-0.0977623369131037));
#51549=CARTESIAN_POINT('Ctrl Pts',(-0.027770665904561,-0.0762515585212508,
-0.0959096361962073));
#51550=CARTESIAN_POINT('Ctrl Pts',(-0.00231403248726689,-0.0770164274158603,
-0.0940569354793108));
#51551=CARTESIAN_POINT('Ctrl Pts',(0.0231426009300273,-0.0777812963104697,
-0.0922042347624142));
#51552=CARTESIAN_POINT('Ctrl Pts',(0.0490159858854629,-0.0646756753216641,
-0.0903515340455175));
#51553=CARTESIAN_POINT('Ctrl Pts',(0.0634603097011373,-0.0436998147451068,
-0.0884988333286209));
#51554=CARTESIAN_POINT('Ctrl Pts',(0.0779046335168115,-0.0227239541685498,
-0.0866461326117244));
#51555=CARTESIAN_POINT('Ctrl Pts',(0.0809198961927247,0.00612214599575843,
-0.084793431894828));
#51556=CARTESIAN_POINT('Ctrl Pts',(0.0711255935060718,0.0296316525829691,
-0.0829407311779315));
#51557=CARTESIAN_POINT('Ctrl Pts',(0.0613312908194188,0.05314115917018,
-0.0810880304610349));
#51558=CARTESIAN_POINT('Ctrl Pts',(0.0387274227701992,0.0713140721802931,
-0.0792353297441383));
#51559=CARTESIAN_POINT('Ctrl Pts',(0.0136629006290876,0.0758301399323035,
-0.0773826290272417));
#51560=CARTESIAN_POINT('Ctrl Pts',(-0.0114016215120237,0.0803462076843139,
-0.0755299283103452));
#51561=CARTESIAN_POINT('Ctrl Pts',(-0.038926797745027,0.0712054301782222,
-0.0736772275934487));
#51562=CARTESIAN_POINT('Ctrl Pts',(-0.0563105718570226,0.0525928101208236,
-0.0718245268765522));
#51563=CARTESIAN_POINT('Ctrl Pts',(-0.0693994868118571,0.0385786495911013,
-0.0704295569486189));
#51564=CARTESIAN_POINT('Ctrl Pts',(-0.0767390728503088,0.0191947445603847,
-0.0690345870206855));
#51565=CARTESIAN_POINT('Ctrl Pts',(-0.0769139474189681,-7.03763467951925E-5,
-0.0676396170927522));
#51566=CARTESIAN_POINT('Origin',(0.,0.,-0.1404));
#51567=CARTESIAN_POINT('',(-0.0770493699172285,1.64405594954022E-5,-0.027610382907248));
#51568=CARTESIAN_POINT('',(-0.0770428135801558,2.35063928346054E-5,-0.0326396170927521));
#51569=CARTESIAN_POINT('',(-0.076925,-9.42059550244101E-18,-0.1404));
#51570=CARTESIAN_POINT('Ctrl Pts',(-0.0770493699172285,1.64405594954022E-5,
-0.027610382907248));
#51571=CARTESIAN_POINT('Ctrl Pts',(-0.0770516866976547,0.000841965750576208,
-0.0276704255226481));
#51572=CARTESIAN_POINT('Ctrl Pts',(-0.0770396341883357,0.00166742001064634,
-0.0277304681380481));
#51573=CARTESIAN_POINT('Ctrl Pts',(-0.0770130084973636,0.00249239931151181,
-0.0277905107534482));
#51574=CARTESIAN_POINT('Ctrl Pts',(-0.076191434746402,0.0279483147801234,
-0.0296432114703447));
#51575=CARTESIAN_POINT('Ctrl Pts',(-0.0614944545164623,0.0529520124570084,
-0.0314959121872412));
#51576=CARTESIAN_POINT('Ctrl Pts',(-0.0396580599576723,0.0660601778222555,
-0.0333486129041378));
#51577=CARTESIAN_POINT('Ctrl Pts',(-0.0178216653988821,0.0791683431875028,
-0.0352013136210344));
#51578=CARTESIAN_POINT('Ctrl Pts',(0.0111541434887584,0.0803809762411121,
-0.037054014337931));
#51579=CARTESIAN_POINT('Ctrl Pts',(0.0340069177013224,0.0691406095455749,
-0.0389067150548276));
#51580=CARTESIAN_POINT('Ctrl Pts',(0.0568596919138859,0.057900242850038,
-0.0407594157717241));
#51581=CARTESIAN_POINT('Ctrl Pts',(0.0735894314513733,0.0342068764053553,
-0.0426121164886206));
#51582=CARTESIAN_POINT('Ctrl Pts',(0.0765346405079689,0.00890943025306635,
-0.0444648172055171));
#51583=CARTESIAN_POINT('Ctrl Pts',(0.0794798495645645,-0.0163880158992229,
-0.0463175179224137));
#51584=CARTESIAN_POINT('Ctrl Pts',(0.068640528140268,-0.0432895417591185,
-0.0481702186393103));
#51585=CARTESIAN_POINT('Ctrl Pts',(0.048980375614107,-0.0594792442461057,
-0.0500229193562068));
#51586=CARTESIAN_POINT('Ctrl Pts',(0.0293202230879464,-0.0756689467330926,
-0.0518756200731034));
#51587=CARTESIAN_POINT('Ctrl Pts',(0.000839239459921554,-0.0811468258471716,
-0.0537283207899999));
#51588=CARTESIAN_POINT('Ctrl Pts',(-0.0234234562141086,-0.07340456771045,
-0.0555810215068964));
#51589=CARTESIAN_POINT('Ctrl Pts',(-0.0476861518881389,-0.0656623095737284,
-0.057433722223793));
#51590=CARTESIAN_POINT('Ctrl Pts',(-0.0677305596081746,-0.044699914186206,
-0.0592864229406895));
#51591=CARTESIAN_POINT('Ctrl Pts',(-0.0743793001795075,-0.020114934867124,
-0.0611391236575861));
#51592=CARTESIAN_POINT('Ctrl Pts',(-0.0761392572294086,-0.0136071598667203,
-0.0616295434074734));
#51593=CARTESIAN_POINT('Ctrl Pts',(-0.076960594478556,-0.00684555435751792,
-0.0621199631573607));
#51594=CARTESIAN_POINT('Ctrl Pts',(-0.0769006083194561,-6.96495813230711E-5,
-0.062610382907248));
#51595=CARTESIAN_POINT('Ctrl Pts',(-0.0769139474189681,-7.03763467951925E-5,
-0.0676396170927522));
#51596=CARTESIAN_POINT('Ctrl Pts',(-0.0769713289242459,-0.00639183089268636,
-0.067181886303789));
#51597=CARTESIAN_POINT('Ctrl Pts',(-0.0762572933205676,-0.0127004960742668,
-0.0667241555148257));
#51598=CARTESIAN_POINT('Ctrl Pts',(-0.0747218360399382,-0.0188024656559839,
-0.0662664247258625));
#51599=CARTESIAN_POINT('Ctrl Pts',(-0.0685069541198702,-0.0435006587666868,
-0.0644137240089659));
#51600=CARTESIAN_POINT('Ctrl Pts',(-0.0488348182887464,-0.0648125823793867,
-0.0625610232920694));
#51601=CARTESIAN_POINT('Ctrl Pts',(-0.024712114252781,-0.0729807992742525,
-0.0607083225751728));
#51602=CARTESIAN_POINT('Ctrl Pts',(-0.000589410216815831,-0.0811490161691181,
-0.0588556218582763));
#51603=CARTESIAN_POINT('Ctrl Pts',(0.0279838620239908,-0.07617352634615,
-0.0570029211413797));
#51604=CARTESIAN_POINT('Ctrl Pts',(0.0479258495855115,-0.0603323589270951,
-0.0551502204244832));
#51605=CARTESIAN_POINT('Ctrl Pts',(0.0678678371470326,-0.0444911915080398,
-0.0532975197075866));
#51606=CARTESIAN_POINT('Ctrl Pts',(0.0791785400292676,-0.0177843464928974,
-0.0514448189906901));
#51607=CARTESIAN_POINT('Ctrl Pts',(0.0766793543706361,0.00756088938670773,
-0.0495921182737935));
#51608=CARTESIAN_POINT('Ctrl Pts',(0.0741801687120046,0.0329061252663129,
-0.047739417556897));
#51609=CARTESIAN_POINT('Ctrl Pts',(0.0578710945125066,0.0568897520103807,
-0.0458867168400004));
#51610=CARTESIAN_POINT('Ctrl Pts',(0.0352193012944682,0.0685309362054083,
-0.0440340161231038));
#51611=CARTESIAN_POINT('Ctrl Pts',(0.0125675080764302,0.0801721204004357,
-0.0421813154062073));
#51612=CARTESIAN_POINT('Ctrl Pts',(-0.0164270041601479,0.0794708620464232,
-0.0403286146893108));
#51613=CARTESIAN_POINT('Ctrl Pts',(-0.0384899414196672,0.0667486447887284,
-0.0384759139724143));
#51614=CARTESIAN_POINT('Ctrl Pts',(-0.0605528786791868,0.0540264275310334,
-0.0366232132555177));
#51615=CARTESIAN_POINT('Ctrl Pts',(-0.0756842409616474,0.0292832513696559,
-0.0347705125386211));
#51616=CARTESIAN_POINT('Ctrl Pts',(-0.0769553882282587,0.00384667954290156,
-0.0329178118217246));
#51617=CARTESIAN_POINT('Ctrl Pts',(-0.0770190118284969,0.00257352550336055,
-0.0328250802454004));
#51618=CARTESIAN_POINT('Ctrl Pts',(-0.0770479126307905,0.00129863435962909,
-0.0327323486690763));
#51619=CARTESIAN_POINT('Ctrl Pts',(-0.0770428135801558,2.35063928346054E-5,
-0.0326396170927521));
#51620=CARTESIAN_POINT('Origin',(0.,0.,-0.348563377523455));
#51621=CARTESIAN_POINT('',(-0.0570170345471334,1.21661208853844E-5,-0.0160633775234553));
#51622=CARTESIAN_POINT('',(-0.0568588689186872,3.50203243198108E-5,-0.00918662247654445));
#51623=CARTESIAN_POINT('',(-0.056925,-2.21215249084286E-15,-0.348563377523455));
#51624=CARTESIAN_POINT('',(0.0551371004056302,-0.0145210214852679,-9.0205620750794E-17));
#51625=CARTESIAN_POINT('Ctrl Pts',(-0.0570170345471334,1.21661208853871E-5,
-0.0160633775234553));
#51626=CARTESIAN_POINT('Ctrl Pts',(-0.0569658477122017,-0.0182269476124025,
-0.0142707194219589));
#51627=CARTESIAN_POINT('Ctrl Pts',(-0.0375869816080576,-0.0554112150194986,
-0.0106253606035659));
#51628=CARTESIAN_POINT('Ctrl Pts',(0.0240591212233117,-0.0619826963587815,
-0.00527090142908081));
#51629=CARTESIAN_POINT('Ctrl Pts',(0.0506098361506637,-0.0313215184444117,
-0.00170910035609219));
#51630=CARTESIAN_POINT('Ctrl Pts',(0.0551371004056302,-0.0145210214852679,
-9.23469200414528E-17));
#51631=CARTESIAN_POINT('',(0.00445734406721156,-0.056750222104116,0.));
#51632=CARTESIAN_POINT('Origin',(0.,0.,0.));
#51633=CARTESIAN_POINT('Ctrl Pts',(-0.0568588689186873,3.50203243198116E-5,
-0.00918662247654445));
#51634=CARTESIAN_POINT('Ctrl Pts',(-0.0567637403779411,-0.0123641010103422,
-0.00797711570125951));
#51635=CARTESIAN_POINT('Ctrl Pts',(-0.0466628848186406,-0.0438764064141307,
-0.00491490820907802));
#51636=CARTESIAN_POINT('Ctrl Pts',(-0.0144175559217569,-0.0582327171563943,
-0.0018527007168965));
#51637=CARTESIAN_POINT('Ctrl Pts',(0.00445734406721196,-0.0567502221041159,
5.55111512312578E-17));
#51638=CARTESIAN_POINT('Origin',(0.,0.,-0.348563377523455));
#51639=CARTESIAN_POINT('',(-0.0569069499978555,-5.15411428926268E-5,-0.0510633775234553));
#51640=CARTESIAN_POINT('',(-0.0570121828150844,1.7394883483156E-5,-0.0441866224765445));
#51641=CARTESIAN_POINT('',(-0.056925,-2.21215249084286E-15,-0.348563377523455));
#51642=CARTESIAN_POINT('Ctrl Pts',(-0.0569069499978555,-5.154114289264E-5,
-0.0510633775234553));
#51643=CARTESIAN_POINT('Ctrl Pts',(-0.0569513401454896,-0.00506575471955614,
-0.0505729577735681));
#51644=CARTESIAN_POINT('Ctrl Pts',(-0.0540474263512665,-0.0289720362496396,
-0.0482298373067843));
#51645=CARTESIAN_POINT('Ctrl Pts',(-0.0204550703512412,-0.0641028447178318,
-0.0440340161231039));
#51646=CARTESIAN_POINT('Ctrl Pts',(0.0427732686682708,-0.0519418462686033,
-0.0384759139724143));
#51647=CARTESIAN_POINT('Ctrl Pts',(0.0668367735916919,0.00778006570700472,
-0.0329178118217246));
#51648=CARTESIAN_POINT('Ctrl Pts',(0.0296964255967034,0.0603798012232959,
-0.027359709671035));
#51649=CARTESIAN_POINT('Ctrl Pts',(-0.0346304351480055,0.0576877321985291,
-0.0218016075203453));
#51650=CARTESIAN_POINT('Ctrl Pts',(-0.056734623549977,0.0200822897505687,
-0.0180361634711521));
#51651=CARTESIAN_POINT('Ctrl Pts',(-0.0570187489797074,0.000623060128065452,
-0.0161234201388554));
#51652=CARTESIAN_POINT('Ctrl Pts',(-0.0570170345471334,1.21661208853871E-5,
-0.0160633775234553));
#51653=CARTESIAN_POINT('Ctrl Pts',(-0.0570121828150844,1.73948834831544E-5,
-0.0441866224765445));
#51654=CARTESIAN_POINT('Ctrl Pts',(-0.0569405680998085,-0.017891414583955,
-0.0424266533359722));
#51655=CARTESIAN_POINT('Ctrl Pts',(-0.0381902384809938,-0.0547822163819881,
-0.0388139834785033));
#51656=CARTESIAN_POINT('Ctrl Pts',(0.0246325962628555,-0.0626129044013398,
-0.0333486129041379));
#51657=CARTESIAN_POINT('Ctrl Pts',(0.0659756148843137,-0.0132517004322241,
-0.0277905107534482));
#51658=CARTESIAN_POINT('Ctrl Pts',(0.0468879053916966,0.0482596214522584,
-0.0222324086027585));
#51659=CARTESIAN_POINT('Ctrl Pts',(-0.0150988217618111,0.0655506182074447,
-0.0166743064520689));
#51660=CARTESIAN_POINT('Ctrl Pts',(-0.0528320738248041,0.0321628305059058,
-0.0123257110766642));
#51661=CARTESIAN_POINT('Ctrl Pts',(-0.0569094565651003,0.00662864996470196,
-0.00982981641815606));
#51662=CARTESIAN_POINT('Ctrl Pts',(-0.0568588689186873,3.50203243198116E-5,
-0.00918662247654445));
#51663=CARTESIAN_POINT('Origin',(0.,0.,-0.348563377523455));
#51664=CARTESIAN_POINT('',(-0.0568373343912269,1.88788443762929E-5,-0.0860633775234553));
#51665=CARTESIAN_POINT('',(-0.0569168210181964,-5.20789540658581E-5,-0.0791866224765445));
#51666=CARTESIAN_POINT('',(-0.056925,-2.21215249084286E-15,-0.348563377523455));
#51667=CARTESIAN_POINT('Ctrl Pts',(-0.0568373343912269,1.88788443762919E-5,
-0.0860633775234553));
#51668=CARTESIAN_POINT('Ctrl Pts',(-0.0568055791606208,-0.0106562996884056,
-0.0850224954082807));
#51669=CARTESIAN_POINT('Ctrl Pts',(-0.0487872375507933,-0.0403768531512196,
-0.0821289125762096));
#51670=CARTESIAN_POINT('Ctrl Pts',(-0.000836488591294147,-0.0672820666389896,
-0.0773826290272417));
#51671=CARTESIAN_POINT('Ctrl Pts',(0.0560818346371597,-0.0371806680059875,
-0.0718245268765522));
#51672=CARTESIAN_POINT('Ctrl Pts',(0.0616474222580996,0.0269661419500831,
-0.0662664247258625));
#51673=CARTESIAN_POINT('Ctrl Pts',(0.0107639014093499,0.0664207519792408,
-0.0607083225751728));
#51674=CARTESIAN_POINT('Ctrl Pts',(-0.0446163690890475,0.0469405944497037,
-0.0556406401743705));
#51675=CARTESIAN_POINT('Ctrl Pts',(-0.0567836436806478,0.0138768696145832,
-0.0524256584904646));
#51676=CARTESIAN_POINT('Ctrl Pts',(-0.0569069499978555,-5.154114289264E-5,
-0.0510633775234553));
#51677=CARTESIAN_POINT('Ctrl Pts',(-0.0569168210181964,-5.2078954065865E-5,
-0.0791866224765445));
#51678=CARTESIAN_POINT('Ctrl Pts',(-0.0569592837050722,-0.00472999640645199,
-0.0787288916875813));
#51679=CARTESIAN_POINT('Ctrl Pts',(-0.0542921893886136,-0.0282943746581153,
-0.0764184601817215));
#51680=CARTESIAN_POINT('Ctrl Pts',(-0.0215805745713374,-0.0637326942294381,
-0.0722553279589653));
#51681=CARTESIAN_POINT('Ctrl Pts',(0.0418526469681333,-0.0526870098028222,
-0.0666972258082757));
#51682=CARTESIAN_POINT('Ctrl Pts',(0.0669626279198866,0.0066027069012525,
-0.061139123657586));
#51683=CARTESIAN_POINT('Ctrl Pts',(0.0307561651780042,0.0598468259421123,
-0.0555810215068964));
#51684=CARTESIAN_POINT('Ctrl Pts',(-0.0336122173660539,0.0582900187220077,
-0.0500229193562067));
#51685=CARTESIAN_POINT('Ctrl Pts',(-0.0565672790378523,0.0207533366878344,
-0.0462247863460895));
#51686=CARTESIAN_POINT('Ctrl Pts',(-0.0570159561456971,0.000960997867036193,
-0.0442793540528687));
#51687=CARTESIAN_POINT('Ctrl Pts',(-0.0570121828150844,1.73948834831544E-5,
-0.0441866224765445));
#51688=CARTESIAN_POINT('Origin',(0.,0.,-0.348563377523455));
#51689=CARTESIAN_POINT('',(-0.0569761128879509,4.19649640993781E-5,-0.121063377523455));
#51690=CARTESIAN_POINT('',(-0.0568344699801726,1.36387320454415E-5,-0.114186622476545));
#51691=CARTESIAN_POINT('',(-0.056925,-2.21215249084286E-15,-0.348563377523455));
#51692=CARTESIAN_POINT('Ctrl Pts',(-0.0569761128879509,4.19649640993761E-5,
-0.121063377523455));
#51693=CARTESIAN_POINT('Ctrl Pts',(-0.0568421140860372,-0.0161776865206131,
-0.119472033042993));
#51694=CARTESIAN_POINT('Ctrl Pts',(-0.041093804968909,-0.0515082139267437,
-0.116027987845635));
#51695=CARTESIAN_POINT('Ctrl Pts',(0.0188553037814868,-0.0645914338274078,
-0.110731241931379));
#51696=CARTESIAN_POINT('Ctrl Pts',(0.0644971261714122,-0.0191754133262199,
-0.10517313978069));
#51697=CARTESIAN_POINT('Ctrl Pts',(0.0510805017286943,0.0437990656879258,
-0.0996150376300002));
#51698=CARTESIAN_POINT('Ctrl Pts',(-0.00910929544596579,0.0666678078505591,
-0.0940569354793109));
#51699=CARTESIAN_POINT('Ctrl Pts',(-0.051248083903741,0.0356400444726433,
-0.0895397154437956));
#51700=CARTESIAN_POINT('Ctrl Pts',(-0.0568621013523766,0.00834480584732116,
-0.0868751961251772));
#51701=CARTESIAN_POINT('Ctrl Pts',(-0.0568373343912269,1.88788443762919E-5,
-0.0860633775234553));
#51702=CARTESIAN_POINT('Ctrl Pts',(-0.0568344699801726,1.36387320454363E-5,
-0.114186622476544));
#51703=CARTESIAN_POINT('Ctrl Pts',(-0.0568123121766602,-0.0103275848846827,
-0.113178429322294));
#51704=CARTESIAN_POINT('Ctrl Pts',(-0.0491635321171548,-0.0397028327409722,
-0.110317535451147));
#51705=CARTESIAN_POINT('Ctrl Pts',(-0.00202079792845361,-0.0672569095516575,
-0.105603940863103));
#51706=CARTESIAN_POINT('Ctrl Pts',(0.0554186211910062,-0.038162175403288,
-0.100045838712414));
#51707=CARTESIAN_POINT('Ctrl Pts',(0.0621125631276854,0.0258767294463682,
-0.0944877365617239));
#51708=CARTESIAN_POINT('Ctrl Pts',(0.0119315352940102,0.0662209506917629,
-0.0889296344110343));
#51709=CARTESIAN_POINT('Ctrl Pts',(-0.0441425466064682,0.047599427538858,
-0.0838292630493078));
#51710=CARTESIAN_POINT('Ctrl Pts',(-0.0567874127007329,0.0142042357374033,
-0.0805815924044779));
#51711=CARTESIAN_POINT('Ctrl Pts',(-0.0569168210181964,-5.2078954065865E-5,
-0.0791866224765445));
#51712=CARTESIAN_POINT('Origin',(0.,0.,-0.348563377523455));
#51713=CARTESIAN_POINT('',(-0.0569682917973646,-4.47457069638125E-5,-0.156063377523455));
#51714=CARTESIAN_POINT('',(-0.0569668622207115,4.51962923827109E-5,-0.149186622476545));
#51715=CARTESIAN_POINT('',(-0.056925,-2.21215249084286E-15,-0.348563377523455));
#51716=CARTESIAN_POINT('Ctrl Pts',(-0.0569682917973646,-4.4745706963804E-5,
-0.156063377523455));
#51717=CARTESIAN_POINT('Ctrl Pts',(-0.0569937221071028,-0.00299248950368808,
-0.155774271394602));
#51718=CARTESIAN_POINT('Ctrl Pts',(-0.0554451413155874,-0.0248036997598682,
-0.153632464548853));
#51719=CARTESIAN_POINT('Ctrl Pts',(-0.0272715619458597,-0.0615129069466198,
-0.149637956986207));
#51720=CARTESIAN_POINT('Ctrl Pts',(0.0369020781931099,-0.0562655523889355,
-0.144079854835517));
#51721=CARTESIAN_POINT('Ctrl Pts',(0.0672853847370649,0.000502797531543261,
-0.138521752684828));
#51722=CARTESIAN_POINT('Ctrl Pts',(0.0360571029361317,0.0568107482943974,
-0.132963650534138));
#51723=CARTESIAN_POINT('Ctrl Pts',(-0.0281877896808826,0.0610984803647731,
-0.127405548383449));
#51724=CARTESIAN_POINT('Ctrl Pts',(-0.0556177361256695,0.0242302520899051,
-0.123438790713221));
#51725=CARTESIAN_POINT('Ctrl Pts',(-0.0569981203307044,0.00270581752422716,
-0.12132473375989));
#51726=CARTESIAN_POINT('Ctrl Pts',(-0.0569761128879509,4.19649640993761E-5,
-0.121063377523455));
#51727=CARTESIAN_POINT('Ctrl Pts',(-0.0569668622207115,4.51962923827061E-5,
-0.149186622476545));
#51728=CARTESIAN_POINT('Ctrl Pts',(-0.0568288651124137,-0.0158479843568857,
-0.147627966957007));
#51729=CARTESIAN_POINT('Ctrl Pts',(-0.0416256884202204,-0.0508640579981459,
-0.144216610720572));
#51730=CARTESIAN_POINT('Ctrl Pts',(0.0177153124424513,-0.064913350971688,
-0.138952553767241));
#51731=CARTESIAN_POINT('Ctrl Pts',(0.0641495648705027,-0.0203078496210804,
-0.133394451616552));
#51732=CARTESIAN_POINT('Ctrl Pts',(0.0518436232068167,0.0428930549861271,
-0.127836349465862));
#51733=CARTESIAN_POINT('Ctrl Pts',(-0.00793426170214403,0.0668178339606645,
-0.122278247315172));
#51734=CARTESIAN_POINT('Ctrl Pts',(-0.0509215769942879,0.036317562629813,
-0.117728338318733));
#51735=CARTESIAN_POINT('Ctrl Pts',(-0.0568530303448794,0.00867590896718897,
-0.11503113003919));
#51736=CARTESIAN_POINT('Ctrl Pts',(-0.0568344699801726,1.36387320454363E-5,
-0.114186622476544));
#51737=CARTESIAN_POINT('Origin',(0.,0.,-0.348563377523455));
#51738=CARTESIAN_POINT('',(-0.0568348355527671,-1.44497151729769E-5,-0.191063377523455));
#51739=CARTESIAN_POINT('',(-0.0569774640760416,-4.14258005045076E-5,-0.184186622476544));
#51740=CARTESIAN_POINT('',(-0.056925,-2.21215249084286E-15,-0.348563377523455));
#51741=CARTESIAN_POINT('Ctrl Pts',(-0.056834835552767,-1.44497151729744E-5,
-0.191063377523455));
#51742=CARTESIAN_POINT('Ctrl Pts',(-0.0568543868502049,-0.00862591271069301,
-0.190223809029315));
#51743=CARTESIAN_POINT('Ctrl Pts',(-0.0509714490781074,-0.0362151985657714,
-0.187531539818278));
#51744=CARTESIAN_POINT('Ctrl Pts',(-0.00811195152116181,-0.0667965098284243,
-0.182986569890345));
#51745=CARTESIAN_POINT('Ctrl Pts',(0.0517293388381684,-0.0430308000507443,
-0.177428467739655));
#51746=CARTESIAN_POINT('Ctrl Pts',(0.0642033633612193,0.0201371382645114,
-0.171870365588966));
#51747=CARTESIAN_POINT('Ctrl Pts',(0.0178879160433239,0.0648660037698966,
-0.166312263438276));
#51748=CARTESIAN_POINT('Ctrl Pts',(-0.0415459569642868,0.0509615686075912,
-0.161043267416439));
#51749=CARTESIAN_POINT('Ctrl Pts',(-0.0568307551258429,0.0158977604785168,
-0.157626972111499));
#51750=CARTESIAN_POINT('Ctrl Pts',(-0.0569682917973646,-4.4745706963804E-5,
-0.156063377523455));
#51751=CARTESIAN_POINT('Ctrl Pts',(-0.0569774640760416,-4.14258005045011E-5,
-0.184186622476544));
#51752=CARTESIAN_POINT('Ctrl Pts',(-0.0569988598076398,-0.0026547751392027,
-0.183930205308616));
#51753=CARTESIAN_POINT('Ctrl Pts',(-0.0556479599452488,-0.0241282167988981,
-0.18182108742379));
#51754=CARTESIAN_POINT('Ctrl Pts',(-0.0283502073114013,-0.061023285478019,
-0.177859268822069));
#51755=CARTESIAN_POINT('Ctrl Pts',(0.0359058577506595,-0.0569064546902456,
-0.172301166671379));
#51756=CARTESIAN_POINT('Ctrl Pts',(0.0672838070486334,-0.000681773972618921,
-0.166743064520689));
#51757=CARTESIAN_POINT('Ctrl Pts',(0.0370516110423173,0.0561671930091792,
-0.161184962369999));
#51758=CARTESIAN_POINT('Ctrl Pts',(-0.0271078417631468,0.0615852280566224,
-0.15562686021931));
#51759=CARTESIAN_POINT('Ctrl Pts',(-0.0554139216188823,0.0249057972609597,
-0.151627413588158));
#51760=CARTESIAN_POINT('Ctrl Pts',(-0.0569928958031393,0.00304349410873103,
-0.149480667673903));
#51761=CARTESIAN_POINT('Ctrl Pts',(-0.0569668622207115,4.51962923827061E-5,
-0.149186622476545));
#51762=CARTESIAN_POINT('Origin',(0.,0.,-0.348563377523455));
#51763=CARTESIAN_POINT('',(-0.0569144593207152,5.12769584049947E-5,-0.226063377523455));
#51764=CARTESIAN_POINT('',(-0.0568377956013138,-1.97155662660445E-5,-0.219186622476544));
#51765=CARTESIAN_POINT('',(-0.056925,-2.21215249084286E-15,-0.348563377523455));
#51766=CARTESIAN_POINT('Ctrl Pts',(-0.0569144593207152,5.12769584049893E-5,
-0.226063377523455));
#51767=CARTESIAN_POINT('Ctrl Pts',(-0.056786042516509,-0.0141553962841083,
-0.224673346664028));
#51768=CARTESIAN_POINT('Ctrl Pts',(-0.0442160058077755,-0.0474988985344208,
-0.221430615087703));
#51769=CARTESIAN_POINT('Ctrl Pts',(0.011756104030695,-0.0662531338471764,
-0.216335182794483));
#51770=CARTESIAN_POINT('Ctrl Pts',(0.0620431155853323,-0.0260414998574271,
-0.210777080643793));
#51771=CARTESIAN_POINT('Ctrl Pts',(0.0555201480174088,0.0380144415731405,
-0.205218978493103));
#51772=CARTESIAN_POINT('Ctrl Pts',(-0.00184199994446337,0.0672621487551179,
-0.199660876342414));
#51773=CARTESIAN_POINT('Ctrl Pts',(-0.0491071931595563,0.0398046976257449,
-0.194942342685864));
#51774=CARTESIAN_POINT('Ctrl Pts',(-0.0568112424218084,0.0103772582952248,
-0.192076509746212));
#51775=CARTESIAN_POINT('Ctrl Pts',(-0.056834835552767,-1.44497151729744E-5,
-0.191063377523455));
#51776=CARTESIAN_POINT('Ctrl Pts',(-0.0568377956013138,-1.97155662660506E-5,
-0.219186622476544));
#51777=CARTESIAN_POINT('Ctrl Pts',(-0.0568634717455984,-0.00829475652583425,
-0.218379742943328));
#51778=CARTESIAN_POINT('Ctrl Pts',(-0.0512968444894828,-0.035537488922977,
-0.215720162693216));
#51779=CARTESIAN_POINT('Ctrl Pts',(-0.0092865044532633,-0.0666434551280208,
-0.211207881726207));
#51780=CARTESIAN_POINT('Ctrl Pts',(0.0509637654586514,-0.0439347205576348,
-0.205649779575517));
#51781=CARTESIAN_POINT('Ctrl Pts',(0.0645479274348034,0.0190037516412805,
-0.200091677424827));
#51782=CARTESIAN_POINT('Ctrl Pts',(0.0190270343003033,0.0645410651484606,
-0.194533575274137));
#51783=CARTESIAN_POINT('Ctrl Pts',(-0.0410125742824414,0.0516052793677545,
-0.189231890291377));
#51784=CARTESIAN_POINT('Ctrl Pts',(-0.0568442684142835,0.0162275572428938,
-0.185782906025512));
#51785=CARTESIAN_POINT('Ctrl Pts',(-0.0569774640760416,-4.14258005045011E-5,
-0.184186622476544));
#51786=CARTESIAN_POINT('Origin',(0.,0.,-0.348563377523455));
#51787=CARTESIAN_POINT('',(-0.056925,-2.21215249084286E-15,-0.2608));
#51788=CARTESIAN_POINT('',(-0.0569006472781276,4.53843407899977E-5,-0.254186622476544));
#51789=CARTESIAN_POINT('',(-0.056925,-2.21215249084286E-15,-0.348563377523455));
#51790=CARTESIAN_POINT('',(-0.0568613829974075,-0.00269049226390485,-0.2608));
#51791=CARTESIAN_POINT('Origin',(0.,0.,-0.2608));
#51792=CARTESIAN_POINT('Ctrl Pts',(-0.0568613829974075,-0.00269049226390492,
-0.2608));
#51793=CARTESIAN_POINT('Ctrl Pts',(-0.0559665358845781,-0.0216023639274464,
-0.258947299283104));
#51794=CARTESIAN_POINT('Ctrl Pts',(-0.0338414445280129,-0.0581356593406026,
-0.255241897849311));
#51795=CARTESIAN_POINT('Ctrl Pts',(0.030633014621353,-0.0599605699382118,
-0.249683795698621));
#51796=CARTESIAN_POINT('Ctrl Pts',(0.0669261363759389,-0.00676409500895024,
-0.244125693547931));
#51797=CARTESIAN_POINT('Ctrl Pts',(0.0420024582515309,0.0525667193079089,
-0.238567591397241));
#51798=CARTESIAN_POINT('Ctrl Pts',(-0.0214161385433601,0.0637944995354849,
-0.233009489246552));
#51799=CARTESIAN_POINT('Ctrl Pts',(-0.0542549075170614,0.0283960803383904,
-0.22884141795529));
#51800=CARTESIAN_POINT('Ctrl Pts',(-0.0569572026771635,0.00477994858439163,
-0.226526047380924));
#51801=CARTESIAN_POINT('Ctrl Pts',(-0.0569144593207152,5.12769584049893E-5,
-0.226063377523455));
#51802=CARTESIAN_POINT('Ctrl Pts',(-0.0569006472781276,4.53843407899985E-5,
-0.254186622476544));
#51803=CARTESIAN_POINT('Ctrl Pts',(-0.0567792970591674,-0.0138322573481857,
-0.252829280578041));
#51804=CARTESIAN_POINT('Ctrl Pts',(-0.04469426298412,-0.0468319938291516,
-0.249619237962641));
#51805=CARTESIAN_POINT('Ctrl Pts',(0.0105915237455798,-0.0664545630371273,
-0.244556494630344));
#51806=CARTESIAN_POINT('Ctrl Pts',(0.0615731857537621,-0.0271271707399214,
-0.238998392479655));
#51807=CARTESIAN_POINT('Ctrl Pts',(0.0561817391408256,0.0370298534016153,
-0.233440290328965));
#51808=CARTESIAN_POINT('Ctrl Pts',(-0.000658152491019542,0.067284844560902,
-0.227882188178275));
#51809=CARTESIAN_POINT('Ctrl Pts',(-0.0487294401428577,0.040478373884527,
-0.223130965560802));
#51810=CARTESIAN_POINT('Ctrl Pts',(-0.0568045159672386,0.0107058175214851,
-0.220232443660225));
#51811=CARTESIAN_POINT('Ctrl Pts',(-0.0568377956013138,-1.97155662660506E-5,
-0.219186622476544));
#51812=CARTESIAN_POINT('Ctrl Pts',(0.0565254421840274,-0.00673275656029344,
-0.272347005383792));
#51813=CARTESIAN_POINT('Ctrl Pts',(0.0587647304548727,0.0120673825140235,
-0.270494304666896));
#51814=CARTESIAN_POINT('Ctrl Pts',(0.0429739129313045,0.0517517526536903,
-0.266788903233103));
#51815=CARTESIAN_POINT('Ctrl Pts',(-0.0203148596464441,0.0641947008942669,
-0.261230801082414));
#51816=CARTESIAN_POINT('Ctrl Pts',(-0.0648913925766018,0.0177190613589564,
-0.255672698931723));
#51817=CARTESIAN_POINT('Ctrl Pts',(-0.0501036428777532,-0.0449120440985994,
-0.250114596781034));
#51818=CARTESIAN_POINT('Ctrl Pts',(0.0105915237455798,-0.0664545630371273,
-0.244556494630344));
#51819=CARTESIAN_POINT('Ctrl Pts',(0.0615731857537621,-0.0271271707399214,
-0.238998392479655));
#51820=CARTESIAN_POINT('Ctrl Pts',(0.0561817391408256,0.0370298534016153,
-0.233440290328965));
#51821=CARTESIAN_POINT('Ctrl Pts',(-0.000658152491019542,0.067284844560902,
-0.227882188178275));
#51822=CARTESIAN_POINT('Ctrl Pts',(-0.0568931784612784,0.03592594721713,
-0.222324086027586));
#51823=CARTESIAN_POINT('Ctrl Pts',(-0.0610336724629001,-0.0283279914129754,
-0.216765983876896));
#51824=CARTESIAN_POINT('Ctrl Pts',(-0.0092865044532633,-0.0666434551280208,
-0.211207881726207));
#51825=CARTESIAN_POINT('Ctrl Pts',(0.0509637654586514,-0.0439347205576348,
-0.205649779575517));
#51826=CARTESIAN_POINT('Ctrl Pts',(0.0645479274348034,0.0190037516412805,
-0.200091677424827));
#51827=CARTESIAN_POINT('Ctrl Pts',(0.0190270343003033,0.0645410651484606,
-0.194533575274137));
#51828=CARTESIAN_POINT('Ctrl Pts',(-0.0439164032436867,0.0509796372246231,
-0.188975473123448));
#51829=CARTESIAN_POINT('Ctrl Pts',(-0.0666466849838619,-0.00926257122266713,
-0.183417370972758));
#51830=CARTESIAN_POINT('Ctrl Pts',(-0.0283502073114013,-0.061023285478019,
-0.177859268822069));
#51831=CARTESIAN_POINT('Ctrl Pts',(0.0359058577506595,-0.0569064546902456,
-0.172301166671379));
#51832=CARTESIAN_POINT('Ctrl Pts',(0.0672838070486334,-0.000681773972618921,
-0.166743064520689));
#51833=CARTESIAN_POINT('Ctrl Pts',(0.0370516110423173,0.0561671930091792,
-0.161184962369999));
#51834=CARTESIAN_POINT('Ctrl Pts',(-0.0271078417631468,0.0615852280566224,
-0.15562686021931));
#51835=CARTESIAN_POINT('Ctrl Pts',(-0.0664453046257158,0.0106111703948657,
-0.15006875806862));
#51836=CARTESIAN_POINT('Ctrl Pts',(-0.0449404200929238,-0.0500792779013919,
-0.144510655917931));
#51837=CARTESIAN_POINT('Ctrl Pts',(0.0177153124424513,-0.064913350971688,
-0.138952553767241));
#51838=CARTESIAN_POINT('Ctrl Pts',(0.0641495648705027,-0.0203078496210804,
-0.133394451616552));
#51839=CARTESIAN_POINT('Ctrl Pts',(0.0518436232068167,0.0428930549861271,
-0.127836349465862));
#51840=CARTESIAN_POINT('Ctrl Pts',(-0.00793426170214403,0.0668178339606645,
-0.122278247315172));
#51841=CARTESIAN_POINT('Ctrl Pts',(-0.0604469360797266,0.029559149487349,
-0.116720145164483));
#51842=CARTESIAN_POINT('Ctrl Pts',(-0.0576098239656634,-0.0347661276820822,
-0.111162043013793));
#51843=CARTESIAN_POINT('Ctrl Pts',(-0.00202079792845361,-0.0672569095516575,
-0.105603940863103));
#51844=CARTESIAN_POINT('Ctrl Pts',(0.0554186211910062,-0.038162175403288,
-0.100045838712414));
#51845=CARTESIAN_POINT('Ctrl Pts',(0.0621125631276854,0.0258767294463682,
-0.0944877365617239));
#51846=CARTESIAN_POINT('Ctrl Pts',(0.0119315352940102,0.0662209506917629,
-0.0889296344110343));
#51847=CARTESIAN_POINT('Ctrl Pts',(-0.0491748926707758,0.045928246387533,
-0.0833715322603447));
#51848=CARTESIAN_POINT('Ctrl Pts',(-0.0652530997134914,-0.0164198082371239,
-0.0778134301096549));
#51849=CARTESIAN_POINT('Ctrl Pts',(-0.0215805745713374,-0.0637326942294381,
-0.0722553279589653));
#51850=CARTESIAN_POINT('Ctrl Pts',(0.0418526469681333,-0.0526870098028222,
-0.0666972258082757));
#51851=CARTESIAN_POINT('Ctrl Pts',(0.0669626279198866,0.0066027069012525,
-0.061139123657586));
#51852=CARTESIAN_POINT('Ctrl Pts',(0.0307561651780042,0.0598468259421123,
-0.0555810215068964));
#51853=CARTESIAN_POINT('Ctrl Pts',(-0.0336122173660539,0.0582900187220077,
-0.0500229193562067));
#51854=CARTESIAN_POINT('Ctrl Pts',(-0.0672041366873037,0.0033596851638767,
-0.0444648172055172));
#51855=CARTESIAN_POINT('Ctrl Pts',(-0.039256160803311,-0.054649352190282,
-0.0389067150548275));
#51856=CARTESIAN_POINT('Ctrl Pts',(0.0246325962628555,-0.0626129044013398,
-0.0333486129041379));
#51857=CARTESIAN_POINT('Ctrl Pts',(0.0659756148843137,-0.0132517004322241,
-0.0277905107534482));
#51858=CARTESIAN_POINT('Ctrl Pts',(0.0468879053916966,0.0482596214522584,
-0.0222324086027585));
#51859=CARTESIAN_POINT('Ctrl Pts',(-0.0150988217618111,0.0655506182074447,
-0.0166743064520689));
#51860=CARTESIAN_POINT('Ctrl Pts',(-0.0633271003986383,0.022876439855447,
-0.0111162043013792));
#51861=CARTESIAN_POINT('Ctrl Pts',(-0.0534357766767865,-0.0408609699628471,
-0.00555810215068963));
#51862=CARTESIAN_POINT('Ctrl Pts',(-0.0144175559217569,-0.0582327171563943,
-0.0018527007168965));
#51863=CARTESIAN_POINT('Ctrl Pts',(0.00445734406721196,-0.0567502221041159,
5.55111512312578E-17));
#51864=CARTESIAN_POINT('Ctrl Pts',(0.0631453153720265,-0.00752125096056229,
-0.268498003589195));
#51865=CARTESIAN_POINT('Ctrl Pts',(0.0656468537697459,0.0134806318203061,
-0.266645302872298));
#51866=CARTESIAN_POINT('Ctrl Pts',(0.0480067236976703,0.0578125639731092,
-0.262939901438505));
#51867=CARTESIAN_POINT('Ctrl Pts',(-0.0226939970666099,0.0717127452092156,
-0.257381799287816));
#51868=CARTESIAN_POINT('Ctrl Pts',(-0.0724910286564263,0.0197941966374174,
-0.251823697137126));
#51869=CARTESIAN_POINT('Ctrl Pts',(-0.0559714388523109,-0.0501718355316076,
-0.246265594986436));
#51870=CARTESIAN_POINT('Ctrl Pts',(0.0118319305669034,-0.0742372669501271,
-0.240707492835747));
#51871=CARTESIAN_POINT('Ctrl Pts',(0.0687842161450679,-0.0303041194431771,
-0.235149390685057));
#51872=CARTESIAN_POINT('Ctrl Pts',(0.0627613601791305,0.0413665365697152,
-0.229591288534368));
#51873=CARTESIAN_POINT('Ctrl Pts',(-0.000735230809393581,0.0751647853673317,
-0.224033186383678));
#51874=CARTESIAN_POINT('Ctrl Pts',(-0.0635561184069704,0.0401333484429689,
-0.218475084232988));
#51875=CARTESIAN_POINT('Ctrl Pts',(-0.068181518747532,-0.0316455720205553,
-0.212916982082299));
#51876=CARTESIAN_POINT('Ctrl Pts',(-0.0103740763406316,-0.0744482807907959,
-0.207358879931609));
#51877=CARTESIAN_POINT('Ctrl Pts',(0.0569322931071538,-0.0490800545418405,
-0.201800777780919));
#51878=CARTESIAN_POINT('Ctrl Pts',(0.0721073392263189,0.021229341059085,
-0.19624267563023));
#51879=CARTESIAN_POINT('Ctrl Pts',(0.0212553504238936,0.0720996732759336,
-0.19068457347954));
#51880=CARTESIAN_POINT('Ctrl Pts',(-0.0490595920293621,0.0569500236658029,
-0.18512647132885));
#51881=CARTESIAN_POINT('Ctrl Pts',(-0.0744518889052628,-0.0103473402137565,
-0.179568369178161));
#51882=CARTESIAN_POINT('Ctrl Pts',(-0.0316703896930619,-0.0681699153100223,
-0.174010267027471));
#51883=CARTESIAN_POINT('Ctrl Pts',(0.040110906235585,-0.0635709494570729,
-0.168452164876781));
#51884=CARTESIAN_POINT('Ctrl Pts',(0.0751636263487222,-0.000761618677361565,
-0.162894062726092));
#51885=CARTESIAN_POINT('Ctrl Pts',(0.0413908423164874,0.0627451105040324,
-0.157335960575402));
#51886=CARTESIAN_POINT('Ctrl Pts',(-0.0302825267888408,0.068797668760077,
-0.151777858424713));
#51887=CARTESIAN_POINT('Ctrl Pts',(-0.0742269242568931,0.0118538780973828,
-0.146219756274023));
#51888=CARTESIAN_POINT('Ctrl Pts',(-0.0502035347283126,-0.0559442204165597,
-0.140661654123333));
#51889=CARTESIAN_POINT('Ctrl Pts',(0.0197900086734511,-0.0725155586685627,
-0.135103551972644));
#51890=CARTESIAN_POINT('Ctrl Pts',(0.0716623231630515,-0.0226861660750207,
-0.129545449821954));
#51891=CARTESIAN_POINT('Ctrl Pts',(0.057915193777078,0.0479163962229738,
-0.123987347671264));
#51892=CARTESIAN_POINT('Ctrl Pts',(-0.00886346816704126,0.0746430816796707,
-0.118429245520575));
#51893=CARTESIAN_POINT('Ctrl Pts',(-0.067526067812091,0.033020914908207,
-0.112871143369885));
#51894=CARTESIAN_POINT('Ctrl Pts',(-0.0643566925313977,-0.0388376987764555,
-0.107313041219195));
#51895=CARTESIAN_POINT('Ctrl Pts',(-0.0022574599607718,-0.0751335788008634,
-0.101754939068506));
#51896=CARTESIAN_POINT('Ctrl Pts',(0.0619088710743035,-0.0426314683798115,
-0.0961968369178161));
#51897=CARTESIAN_POINT('Ctrl Pts',(0.0693867617080029,0.0289072350176012,
-0.0906387347671264));
#51898=CARTESIAN_POINT('Ctrl Pts',(0.0133288751030001,0.0739762955246439,
-0.0850806326164367));
#51899=CARTESIAN_POINT('Ctrl Pts',(-0.0549339197731941,0.0513070484823988,
-0.0795225304657472));
#51900=CARTESIAN_POINT('Ctrl Pts',(-0.0728950964593256,-0.0183427838760783,
-0.0739644283150574));
#51901=CARTESIAN_POINT('Ctrl Pts',(-0.0241079438667659,-0.0711966314836541,
-0.0684063261643679));
#51902=CARTESIAN_POINT('Ctrl Pts',(0.0467541427336881,-0.0588573520429421,
-0.0628482240136781));
#51903=CARTESIAN_POINT('Ctrl Pts',(0.0748048329170919,0.00737597077491671,
-0.0572901218629886));
#51904=CARTESIAN_POINT('Ctrl Pts',(0.0343581168896724,0.0668556768795576,
-0.0517320197122989));
#51905=CARTESIAN_POINT('Ctrl Pts',(-0.0375486503762781,0.0651165470454754,
-0.0461739175616092));
#51906=CARTESIAN_POINT('Ctrl Pts',(-0.0750746255395717,0.00375314851201067,
-0.0406158154109196));
#51907=CARTESIAN_POINT('Ctrl Pts',(-0.0438535738676721,-0.0610495105495594,
-0.03505771326023));
#51908=CARTESIAN_POINT('Ctrl Pts',(0.0275173974647707,-0.0699456995295894,
-0.0294996111095403));
#51909=CARTESIAN_POINT('Ctrl Pts',(0.0737022276653781,-0.0148036489530528,
-0.0239415089588508));
#51910=CARTESIAN_POINT('Ctrl Pts',(0.05237909618563,0.0539114582494777,
-0.018383406808161));
#51911=CARTESIAN_POINT('Ctrl Pts',(-0.016867092499543,0.0732274582844401,
-0.0128253046574715));
#51912=CARTESIAN_POINT('Ctrl Pts',(-0.0707435372774131,0.0255555720299983,
-0.00726720250678171));
#51913=CARTESIAN_POINT('Ctrl Pts',(-0.0596938093720625,-0.0456463273000271,
-0.00170910035609216));
#51914=CARTESIAN_POINT('Ctrl Pts',(-0.0161060414637576,-0.0650525347124059,
0.001996301077701));
#51915=CARTESIAN_POINT('Ctrl Pts',(0.00497935771876632,-0.0633964199789941,
0.00384900179459755));
#51916=CARTESIAN_POINT('Ctrl Pts',(0.0697651885600256,-0.00830974536083114,
-0.264649001794597));
#51917=CARTESIAN_POINT('Ctrl Pts',(0.072528977084619,0.0148938811265888,
-0.262796301077701));
#51918=CARTESIAN_POINT('Ctrl Pts',(0.0530395344640362,0.0638733752925282,
-0.259090899643908));
#51919=CARTESIAN_POINT('Ctrl Pts',(-0.0250731344867759,0.0792307895241642,
-0.253532797493218));
#51920=CARTESIAN_POINT('Ctrl Pts',(-0.0800906647362507,0.0218693319158784,
-0.247974695342528));
#51921=CARTESIAN_POINT('Ctrl Pts',(-0.0618392348268687,-0.0554316269646156,
-0.242416593191839));
#51922=CARTESIAN_POINT('Ctrl Pts',(0.0130723373882271,-0.082019970863127,
-0.236858491041149));
#51923=CARTESIAN_POINT('Ctrl Pts',(0.0759952465363734,-0.0334810681464326,
-0.23130038889046));
#51924=CARTESIAN_POINT('Ctrl Pts',(0.0693409812174357,0.045703219737815,
-0.22574228673977));
#51925=CARTESIAN_POINT('Ctrl Pts',(-0.000812309127767784,0.0830447261737616,
-0.22018418458908));
#51926=CARTESIAN_POINT('Ctrl Pts',(-0.0702190583526623,0.0443407496688078,
-0.214626082438391));
#51927=CARTESIAN_POINT('Ctrl Pts',(-0.0753293650321641,-0.0349631526281352,
-0.209067980287701));
#51928=CARTESIAN_POINT('Ctrl Pts',(-0.0114616482279998,-0.0822531064535709,
-0.203509878137011));
#51929=CARTESIAN_POINT('Ctrl Pts',(0.0629008207556561,-0.0542253885260463,
-0.197951775986322));
#51930=CARTESIAN_POINT('Ctrl Pts',(0.0796667510178346,0.0234549304768895,
-0.192393673835632));
#51931=CARTESIAN_POINT('Ctrl Pts',(0.0234836665474837,0.0796582814034065,
-0.186835571684942));
#51932=CARTESIAN_POINT('Ctrl Pts',(-0.0542027808150372,0.0629204101069829,
-0.181277469534253));
#51933=CARTESIAN_POINT('Ctrl Pts',(-0.0822570928266639,-0.011432109204846,
-0.175719367383563));
#51934=CARTESIAN_POINT('Ctrl Pts',(-0.0349905720747223,-0.0753165451420255,
-0.170161265232874));
#51935=CARTESIAN_POINT('Ctrl Pts',(0.0443159547205104,-0.0702354442239004,
-0.164603163082184));
#51936=CARTESIAN_POINT('Ctrl Pts',(0.0830434456488111,-0.000841463382104197,
-0.159045060931494));
#51937=CARTESIAN_POINT('Ctrl Pts',(0.0457300735906574,0.0693230279988856,
-0.153486958780804));
#51938=CARTESIAN_POINT('Ctrl Pts',(-0.0334572118145347,0.0760101094635317,
-0.147928856630115));
#51939=CARTESIAN_POINT('Ctrl Pts',(-0.0820085438880705,0.0130965857998999,
-0.142370754479425));
#51940=CARTESIAN_POINT('Ctrl Pts',(-0.0554666493637013,-0.0618091629317276,
-0.136812652328736));
#51941=CARTESIAN_POINT('Ctrl Pts',(0.0218647049044507,-0.0801177663654375,
-0.131254550178046));
#51942=CARTESIAN_POINT('Ctrl Pts',(0.0791750814556004,-0.0250644825289609,
-0.125696448027356));
#51943=CARTESIAN_POINT('Ctrl Pts',(0.0639867643473392,0.0529397374598205,
-0.120138345876667));
#51944=CARTESIAN_POINT('Ctrl Pts',(-0.0097926746319385,0.0824683293986771,
-0.114580243725977));
#51945=CARTESIAN_POINT('Ctrl Pts',(-0.0746051995444553,0.036482680329065,
-0.109022141575287));
#51946=CARTESIAN_POINT('Ctrl Pts',(-0.0711035610971321,-0.0429092698708288,
-0.103464039424598));
#51947=CARTESIAN_POINT('Ctrl Pts',(-0.00249412199308987,-0.0830102480500694,
-0.0979059372739083));
#51948=CARTESIAN_POINT('Ctrl Pts',(0.0683991209576008,-0.047100761356335,
-0.0923478351232185));
#51949=CARTESIAN_POINT('Ctrl Pts',(0.0766609602883205,0.0319377405888342,
-0.0867897329725289));
#51950=CARTESIAN_POINT('Ctrl Pts',(0.01472621491199,0.0817316403575249,
-0.0812316308218393));
#51951=CARTESIAN_POINT('Ctrl Pts',(-0.0606929468756124,0.0566858505772645,
-0.0756735286711496));
#51952=CARTESIAN_POINT('Ctrl Pts',(-0.0805370932051599,-0.0202657595150326,
-0.07011542652046));
#51953=CARTESIAN_POINT('Ctrl Pts',(-0.0266353131621943,-0.0786605687378701,
-0.0645573243697703));
#51954=CARTESIAN_POINT('Ctrl Pts',(0.0516556384992429,-0.065027694283062,
-0.0589992222190807));
#51955=CARTESIAN_POINT('Ctrl Pts',(0.0826470379142973,0.00814923464858084,
-0.053441120068391));
#51956=CARTESIAN_POINT('Ctrl Pts',(0.0379600686013405,0.073864527817003,
-0.0478830179177014));
#51957=CARTESIAN_POINT('Ctrl Pts',(-0.0414850833865023,0.071943075368943,
-0.0423249157670118));
#51958=CARTESIAN_POINT('Ctrl Pts',(-0.0829451143918398,0.00414661186014473,
-0.0367668136163221));
#51959=CARTESIAN_POINT('Ctrl Pts',(-0.0484509869320331,-0.0674496689088369,
-0.0312087114656326));
#51960=CARTESIAN_POINT('Ctrl Pts',(0.0304021986666858,-0.0772784946578389,
-0.0256506093149427));
#51961=CARTESIAN_POINT('Ctrl Pts',(0.0814288404464425,-0.0163555974738817,
-0.0200925071642533));
#51962=CARTESIAN_POINT('Ctrl Pts',(0.0578702869795633,0.0595632950466971,
-0.0145344050135635));
#51963=CARTESIAN_POINT('Ctrl Pts',(-0.0186353632372748,0.0809042983614356,
-0.00897630286287398));
#51964=CARTESIAN_POINT('Ctrl Pts',(-0.0781599741561879,0.0282347042045496,
-0.00341820071218422));
#51965=CARTESIAN_POINT('Ctrl Pts',(-0.0659518420673384,-0.050431684637207,
0.00213990143850535));
#51966=CARTESIAN_POINT('Ctrl Pts',(-0.0177945270057585,-0.0718723522684174,
0.0058453028722985));
#51967=CARTESIAN_POINT('Ctrl Pts',(0.00550137137032068,-0.0700426178538723,
0.00769800358919505));
#51968=CARTESIAN_POINT('Ctrl Pts',(0.0763850617480246,-0.00909823976109999,
-0.2608));
#51969=CARTESIAN_POINT('Ctrl Pts',(0.0794111003994922,0.0163071304328715,
-0.258947299283103));
#51970=CARTESIAN_POINT('Ctrl Pts',(0.058072345230402,0.0699341866119471,
-0.25524189784931));
#51971=CARTESIAN_POINT('Ctrl Pts',(-0.0274522719069417,0.086748833839113,
-0.249683795698621));
#51972=CARTESIAN_POINT('Ctrl Pts',(-0.0876903008160753,0.0239444671943393,
-0.244125693547931));
#51973=CARTESIAN_POINT('Ctrl Pts',(-0.0677070308014264,-0.0606914183976236,
-0.238567591397241));
#51974=CARTESIAN_POINT('Ctrl Pts',(0.0143127442095507,-0.089802674776127,
-0.233009489246552));
#51975=CARTESIAN_POINT('Ctrl Pts',(0.0832062769276791,-0.0366580168496882,
-0.227451387095862));
#51976=CARTESIAN_POINT('Ctrl Pts',(0.0759206022557407,0.0500399029059149,
-0.221893284945172));
#51977=CARTESIAN_POINT('Ctrl Pts',(-0.000889387446141895,0.0909246669801913,
-0.216335182794483));
#51978=CARTESIAN_POINT('Ctrl Pts',(-0.0768819982983542,0.0485481508946467,
-0.210777080643793));
#51979=CARTESIAN_POINT('Ctrl Pts',(-0.0824772113167961,-0.038280733235715,
-0.205218978493104));
#51980=CARTESIAN_POINT('Ctrl Pts',(-0.0125492201153681,-0.0900579321163461,
-0.199660876342414));
#51981=CARTESIAN_POINT('Ctrl Pts',(0.0688693484041585,-0.0593707225102519,
-0.194102774191724));
#51982=CARTESIAN_POINT('Ctrl Pts',(0.0872261628093503,0.0256805198946939,
-0.188544672041035));
#51983=CARTESIAN_POINT('Ctrl Pts',(0.025711982671074,0.0872168895308795,
-0.182986569890345));
#51984=CARTESIAN_POINT('Ctrl Pts',(-0.0593459696007125,0.0688907965481627,
-0.177428467739655));
#51985=CARTESIAN_POINT('Ctrl Pts',(-0.0900622967480648,-0.0125168781959353,
-0.171870365588966));
#51986=CARTESIAN_POINT('Ctrl Pts',(-0.0383107544563828,-0.0824631749740288,
-0.166312263438276));
#51987=CARTESIAN_POINT('Ctrl Pts',(0.0485210032054359,-0.0768999389907277,
-0.160754161287586));
#51988=CARTESIAN_POINT('Ctrl Pts',(0.0909232649488999,-0.000921308086846913,
-0.155196059136897));
#51989=CARTESIAN_POINT('Ctrl Pts',(0.0500693048648274,0.0759009454937388,
-0.149637956986207));
#51990=CARTESIAN_POINT('Ctrl Pts',(-0.0366318968402287,0.0832225501669864,
-0.144079854835518));
#51991=CARTESIAN_POINT('Ctrl Pts',(-0.0897901635192477,0.0143392935024171,
-0.138521752684828));
#51992=CARTESIAN_POINT('Ctrl Pts',(-0.0607297639990901,-0.0676741054468955,
-0.132963650534138));
#51993=CARTESIAN_POINT('Ctrl Pts',(0.0239394011354505,-0.0877199740623122,
-0.127405548383449));
#51994=CARTESIAN_POINT('Ctrl Pts',(0.0866878397481493,-0.0274427989829012,
-0.121847446232759));
#51995=CARTESIAN_POINT('Ctrl Pts',(0.0700583349176005,0.0579630786966672,
-0.116289344082069));
#51996=CARTESIAN_POINT('Ctrl Pts',(-0.0107218810968358,0.0902935771176834,
-0.11073124193138));
#51997=CARTESIAN_POINT('Ctrl Pts',(-0.0816843312768195,0.039944445749923,
-0.10517313978069));
#51998=CARTESIAN_POINT('Ctrl Pts',(-0.0778504296628665,-0.0469808409652021,
-0.0996150376300002));
#51999=CARTESIAN_POINT('Ctrl Pts',(-0.002730784025408,-0.0908869172992753,
-0.0940569354793109));
#52000=CARTESIAN_POINT('Ctrl Pts',(0.0748893708408981,-0.0515700543328586,
-0.0884988333286209));
#52001=CARTESIAN_POINT('Ctrl Pts',(0.083935158868638,0.0349682461600672,
-0.0829407311779315));
#52002=CARTESIAN_POINT('Ctrl Pts',(0.01612355472098,0.0894869851904058,
-0.0773826290272417));
#52003=CARTESIAN_POINT('Ctrl Pts',(-0.0664519739780307,0.0620646526721303,
-0.0718245268765522));
#52004=CARTESIAN_POINT('Ctrl Pts',(-0.088179089950994,-0.022188735153987,
-0.0662664247258625));
#52005=CARTESIAN_POINT('Ctrl Pts',(-0.0291626824576228,-0.0861245059920862,
-0.0607083225751728));
#52006=CARTESIAN_POINT('Ctrl Pts',(0.0565571342647977,-0.0711980365231819,
-0.0551502204244832));
#52007=CARTESIAN_POINT('Ctrl Pts',(0.0904892429115026,0.00892249852224505,
-0.0495921182737936));
#52008=CARTESIAN_POINT('Ctrl Pts',(0.0415620203130087,0.0808733787544482,
-0.0440340161231039));
#52009=CARTESIAN_POINT('Ctrl Pts',(-0.0454215163967265,0.0787696036924106,
-0.0384759139724143));
#52010=CARTESIAN_POINT('Ctrl Pts',(-0.0908156032441078,0.00454007520827874,
-0.0329178118217246));
#52011=CARTESIAN_POINT('Ctrl Pts',(-0.0530483999963943,-0.0738498272681144,
-0.0273597096710351));
#52012=CARTESIAN_POINT('Ctrl Pts',(0.0332869998686011,-0.0846112897860884,
-0.0218016075203453));
#52013=CARTESIAN_POINT('Ctrl Pts',(0.0891554532275068,-0.0179075459947105,
-0.0162435053696558));
#52014=CARTESIAN_POINT('Ctrl Pts',(0.0633614777734967,0.0652151318439164,
-0.010685403218966));
#52015=CARTESIAN_POINT('Ctrl Pts',(-0.0204036339750069,0.0885811384384311,
-0.00512730106827648));
#52016=CARTESIAN_POINT('Ctrl Pts',(-0.0855764110349624,0.0309138363791009,
0.00043080108241328));
#52017=CARTESIAN_POINT('Ctrl Pts',(-0.0722098747626145,-0.0552170419743869,
0.00598890323310284));
#52018=CARTESIAN_POINT('Ctrl Pts',(-0.0194830125477592,-0.078692169824429,
0.00969430466689599));
#52019=CARTESIAN_POINT('Ctrl Pts',(0.00602338502187503,-0.0766888157287505,
0.0115470053837926));
#52020=CARTESIAN_POINT('',(-0.0702475453412058,0.0316531309938693,3.81639164714898E-17));
#52021=CARTESIAN_POINT('Ctrl Pts',(-0.0702475453412056,0.0316531309938698,
1.04083408558608E-17));
#52022=CARTESIAN_POINT('Ctrl Pts',(-0.0708401438323926,0.029761073498479,
5.79235680573455E-18));
#52023=CARTESIAN_POINT('Ctrl Pts',(-0.0713533641733164,0.0278477587888483,
-2.19516502096945E-17));
#52024=CARTESIAN_POINT('Ctrl Pts',(-0.0717834091387127,0.0259160599661846,
-5.03069808033274E-17));
#52025=CARTESIAN_POINT('Ctrl Pts',(-0.0726956731599413,0.0218183039695723,
-1.10399493300004E-16));
#52026=CARTESIAN_POINT('Ctrl Pts',(-0.0732342513009639,0.0176375932737427,
-1.2801402186765E-16));
#52027=CARTESIAN_POINT('Ctrl Pts',(-0.0734091543575676,0.0134222320461422,
-1.14491749414469E-16));
#52028=CARTESIAN_POINT('Ctrl Pts',(-0.0735212566871715,0.0107204392764101,
-1.05824786852604E-16));
#52029=CARTESIAN_POINT('Ctrl Pts',(-0.0734832703910439,0.00800545788437908,
-8.75273381590973E-17));
#52030=CARTESIAN_POINT('Ctrl Pts',(-0.0732984068112228,0.00530313201976544,
-9.54097911787244E-17));
#52031=CARTESIAN_POINT('Ctrl Pts',(-0.0729691788812362,0.000490495850885873,
-1.09447838550622E-16));
#52032=CARTESIAN_POINT('Ctrl Pts',(-0.0721756952260308,-0.00429375429852149,
-1.18695651748223E-16));
#52033=CARTESIAN_POINT('Ctrl Pts',(-0.0709276079677427,-0.00897089557555983,
-9.54097911787244E-17));
#52034=CARTESIAN_POINT('Ctrl Pts',(-0.0703102811078677,-0.0112842954749435,
-8.38921772543806E-17));
#52035=CARTESIAN_POINT('Ctrl Pts',(-0.0695840020575365,-0.0135618869643576,
-1.04445390710516E-16));
#52036=CARTESIAN_POINT('Ctrl Pts',(-0.0687513992021191,-0.0157936705084804,
-1.04083408558608E-16));
#52037=CARTESIAN_POINT('Ctrl Pts',(-0.0667739557564809,-0.0210941876910649,
-1.03223695876781E-16));
#52038=CARTESIAN_POINT('Ctrl Pts',(-0.0641981025339425,-0.0261408913163681,
-4.81033231372627E-17));
#52039=CARTESIAN_POINT('Ctrl Pts',(-0.0610330648987858,-0.0307922157670597,
-4.85722573273506E-17));
#52040=CARTESIAN_POINT('Ctrl Pts',(-0.0595995290513461,-0.0328989333188744,
-4.87846510013196E-17));
#52041=CARTESIAN_POINT('Ctrl Pts',(-0.0580434790487478,-0.034924535640895,
-9.75325019484706E-17));
#52042=CARTESIAN_POINT('Ctrl Pts',(-0.0563782123517984,-0.036839591092707,
-8.32667268468867E-17));
#52043=CARTESIAN_POINT('Ctrl Pts',(-0.055297679654866,-0.0380822028833062,
-7.40101696404141E-17));
#52044=CARTESIAN_POINT('Ctrl Pts',(-0.0541700936089916,-0.0392799543399077,
-3.01247228678535E-17));
#52045=CARTESIAN_POINT('Ctrl Pts',(-0.0529957554081263,-0.0404291985015901,
-3.81639164714898E-17));
#52046=CARTESIAN_POINT('Ctrl Pts',(-0.0507006751620624,-0.0426752359475643,
-5.38753992627271E-17));
#52047=CARTESIAN_POINT('Ctrl Pts',(-0.0482270615803998,-0.0447363204158576,
-9.98006814252804E-17));
#52048=CARTESIAN_POINT('Ctrl Pts',(-0.0456008459049946,-0.0466020203916923,
-8.41340885848751E-17));
#52049=CARTESIAN_POINT('Ctrl Pts',(-0.0437719639308629,-0.0479012834670357,
-7.32239605591342E-17));
#52050=CARTESIAN_POINT('Ctrl Pts',(-0.0418673313980074,-0.0491066227264505,
-6.15450822730729E-17));
#52051=CARTESIAN_POINT('Ctrl Pts',(-0.0399010703140815,-0.0502099840408421,
-5.20417042793042E-17));
#52052=CARTESIAN_POINT('Ctrl Pts',(-0.0351580807136298,-0.0528714979580334,
-2.91177785798691E-17));
#52053=CARTESIAN_POINT('Ctrl Pts',(-0.0300947711453647,-0.0549234116843586,
-7.62798734692924E-18));
#52054=CARTESIAN_POINT('Ctrl Pts',(-0.0248427491906684,-0.0563131705928901,
3.51281503885303E-17));
#52055=CARTESIAN_POINT('Ctrl Pts',(-0.0227105540742067,-0.0568773794220593,
5.24861182082942E-17));
#52056=CARTESIAN_POINT('Ctrl Pts',(-0.0205472623921807,-0.0573318683473704,
-3.01179988497144E-17));
#52057=CARTESIAN_POINT('Ctrl Pts',(-0.0183622887047919,-0.0576706893152479,
-2.55871712706579E-17));
#52058=CARTESIAN_POINT('Ctrl Pts',(-0.0161895643360923,-0.0580076107975444,
-2.10817442496316E-17));
#52059=CARTESIAN_POINT('Ctrl Pts',(-0.0140040937456036,-0.058228676608621,
-6.10708131189109E-17));
#52060=CARTESIAN_POINT('Ctrl Pts',(-0.0118192148552885,-0.058329734875705,
-5.48606299277665E-17));
#52061=CARTESIAN_POINT('Ctrl Pts',(-0.0068511720320565,-0.0585595241792404,
-4.07397300598246E-17));
#52062=CARTESIAN_POINT('Ctrl Pts',(-0.00187688283265028,-0.058172909763502,
7.5769660385224E-17));
#52063=CARTESIAN_POINT('Ctrl Pts',(0.00298509850992475,-0.0570979057708017,
3.98444298388423E-17));
#52064=CARTESIAN_POINT('Ctrl Pts',(0.00347707029304418,-0.0569891287941157,
3.62092452329056E-17));
#52065=CARTESIAN_POINT('Ctrl Pts',(0.00396786625890273,-0.0568732671910623,
5.43496127043497E-17));
#52066=CARTESIAN_POINT('Ctrl Pts',(0.00445734406721196,-0.0567502221041159,
5.46437894932694E-17));
#52067=CARTESIAN_POINT('Ctrl Pts',(-0.0770428135801558,2.35063928346054E-5,
-0.0326396170927521));
#52068=CARTESIAN_POINT('Ctrl Pts',(-0.0769460377879284,-0.0241773749120882,
-0.0308796479521797));
#52069=CARTESIAN_POINT('Ctrl Pts',(-0.0646022015971733,-0.0484635620670927,
-0.0291196788116074));
#52070=CARTESIAN_POINT('Ctrl Pts',(-0.044953700560181,-0.0625784206083777,
-0.027359709671035));
#52071=CARTESIAN_POINT('Ctrl Pts',(-0.0242699333747295,-0.0774369814407723,
-0.0255070089541385));
#52072=CARTESIAN_POINT('Ctrl Pts',(0.00450853324693592,-0.0810241356134303,
-0.0236543082372419));
#52073=CARTESIAN_POINT('Ctrl Pts',(0.0282091754509194,-0.071700422067863,
-0.0218016075203453));
#52074=CARTESIAN_POINT('Ctrl Pts',(0.0519098176549031,-0.0623767085222956,
-0.0199489068034488));
#52075=CARTESIAN_POINT('Ctrl Pts',(0.070532635441205,-0.040142127258503,
-0.0180962060865523));
#52076=CARTESIAN_POINT('Ctrl Pts',(0.0755450484253542,-0.0151710569868353,
-0.0162435053696557));
#52077=CARTESIAN_POINT('Ctrl Pts',(0.0805574614095034,0.00980001328483202,
-0.0143908046527592));
#52078=CARTESIAN_POINT('Ctrl Pts',(0.0719594695915001,0.0375075725643739,
-0.0125381039358626));
#52079=CARTESIAN_POINT('Ctrl Pts',(0.0536996217244147,0.0552556866365642,
-0.0106854032189661));
#52080=CARTESIAN_POINT('Ctrl Pts',(0.0354397738573291,0.0730038007087545,
-0.0088327025020695));
#52081=CARTESIAN_POINT('Ctrl Pts',(0.00751806994116074,0.0807924695735928,
-0.00698000178517297));
#52082=CARTESIAN_POINT('Ctrl Pts',(-0.0173049115269158,0.0750755869961235,
-0.00512730106827642));
#52083=CARTESIAN_POINT('Ctrl Pts',(-0.0402038968187358,0.0698018123601118,
-0.00341820071218428));
#52084=CARTESIAN_POINT('Ctrl Pts',(-0.0604658994839416,0.0530349449696514,
-0.00170910035609212));
#52085=CARTESIAN_POINT('Ctrl Pts',(-0.0702475453412058,0.0316531309938693,
3.81639164714898E-17));
#52086=CARTESIAN_POINT('',(-0.0213030042343867,0.0527886127454558,-0.2608));
#52087=CARTESIAN_POINT('Ctrl Pts',(-0.0213170383639363,0.0528823612671138,
-0.2608));
#52088=CARTESIAN_POINT('Ctrl Pts',(-0.0200481268693847,0.0536735018248238,
-0.2608));
#52089=CARTESIAN_POINT('Ctrl Pts',(-0.0187486983558779,0.0544095042513574,
-0.2608));
#52090=CARTESIAN_POINT('Ctrl Pts',(-0.0174215591439766,0.0550876795506691,
-0.2608));
#52091=CARTESIAN_POINT('Ctrl Pts',(-0.0145506047994946,0.0565547527140716,
-0.2608));
#52092=CARTESIAN_POINT('Ctrl Pts',(-0.0115504229589048,0.0577517065377783,
-0.2608));
#52093=CARTESIAN_POINT('Ctrl Pts',(-0.00845775334810257,0.0586900169041967,
-0.2608));
#52094=CARTESIAN_POINT('Ctrl Pts',(-0.00612165927441171,0.0593987836210216,
-0.2608));
#52095=CARTESIAN_POINT('Ctrl Pts',(-0.00373424326947691,0.0599588209332557,
-0.2608));
#52096=CARTESIAN_POINT('Ctrl Pts',(-0.0013224230181328,0.0603724403993434,
-0.2608));
#52097=CARTESIAN_POINT('Ctrl Pts',(0.00185366586643284,0.0609171294937934,
-0.2608));
#52098=CARTESIAN_POINT('Ctrl Pts',(0.00507722273770718,0.0612098644046175,
-0.2608));
#52099=CARTESIAN_POINT('Ctrl Pts',(0.00831585952592858,0.0612587666881257,
-0.2608));
#52100=CARTESIAN_POINT('Ctrl Pts',(0.0106237809657182,0.0612936154951835,
-0.2608));
#52101=CARTESIAN_POINT('Ctrl Pts',(0.0129369100215328,0.0612040722239185,
-0.2608));
#52102=CARTESIAN_POINT('Ctrl Pts',(0.0152328715218333,0.0609941762980662,
-0.2608));
#52103=CARTESIAN_POINT('Ctrl Pts',(0.0208062876393118,0.060484656719456,
-0.2608));
#52104=CARTESIAN_POINT('Ctrl Pts',(0.0262953704594572,0.0592700592891648,
-0.2608));
#52105=CARTESIAN_POINT('Ctrl Pts',(0.0315473617407771,0.0573779411784005,
-0.2608));
#52106=CARTESIAN_POINT('Ctrl Pts',(0.0337256011567474,0.0565931938268203,
-0.2608));
#52107=CARTESIAN_POINT('Ctrl Pts',(0.0358639963394174,0.0556903260001544,
-0.2608));
#52108=CARTESIAN_POINT('Ctrl Pts',(0.037936308404479,0.0546778727850125,
-0.2608));
#52109=CARTESIAN_POINT('Ctrl Pts',(0.0396703860429882,0.0538306681047839,
-0.2608));
#52110=CARTESIAN_POINT('Ctrl Pts',(0.0413607927286621,0.0529059149903486,
-0.2608));
#52111=CARTESIAN_POINT('Ctrl Pts',(0.0430016005716766,0.0519049229280611,
-0.2608));
#52112=CARTESIAN_POINT('Ctrl Pts',(0.0469776787705488,0.0494792746517871,
-0.2608));
#52113=CARTESIAN_POINT('Ctrl Pts',(0.0506632023142616,0.0466076377773078,
-0.2608));
#52114=CARTESIAN_POINT('Ctrl Pts',(0.0540354991512064,0.0433644171385233,
-0.2608));
#52115=CARTESIAN_POINT('Ctrl Pts',(0.0556363092948981,0.0418248787325567,
-0.2608));
#52116=CARTESIAN_POINT('Ctrl Pts',(0.0571654283791441,0.0402016121639473,
-0.2608));
#52117=CARTESIAN_POINT('Ctrl Pts',(0.0586117445441614,0.0385124592197734,
-0.2608));
#52118=CARTESIAN_POINT('Ctrl Pts',(0.0616191130766601,0.0350001528971615,
-0.2608));
#52119=CARTESIAN_POINT('Ctrl Pts',(0.0642799176321896,0.03119412357567,
-0.2608));
#52120=CARTESIAN_POINT('Ctrl Pts',(0.0665734050653256,0.0271625612678484,
-0.2608));
#52121=CARTESIAN_POINT('Ctrl Pts',(0.067877037446238,0.0248709964246282,
-0.2608));
#52122=CARTESIAN_POINT('Ctrl Pts',(0.0690618528571677,0.0225062289479046,
-0.2608));
#52123=CARTESIAN_POINT('Ctrl Pts',(0.0701224224214427,0.0200787123815737,
-0.2608));
#52124=CARTESIAN_POINT('Ctrl Pts',(0.0710336990934438,0.0179929093448766,
-0.2608));
#52125=CARTESIAN_POINT('Ctrl Pts',(0.0718509983303909,0.0158652248358311,
-0.2608));
#52126=CARTESIAN_POINT('Ctrl Pts',(0.0725692291932556,0.0137105298517765,
-0.2608));
#52127=CARTESIAN_POINT('Ctrl Pts',(0.0745628323709498,0.00772971366958114,
-0.2608));
#52128=CARTESIAN_POINT('Ctrl Pts',(0.075803672795126,0.00152629816288074,
-0.2608));
#52129=CARTESIAN_POINT('Ctrl Pts',(0.0762256437052851,-0.00475840477433878,
-0.2608));
#52130=CARTESIAN_POINT('Ctrl Pts',(0.0763225129083206,-0.00620114442815519,
-0.2608));
#52131=CARTESIAN_POINT('Ctrl Pts',(0.0763760414501779,-0.00764827653023567,
-0.2608));
#52132=CARTESIAN_POINT('Ctrl Pts',(0.0763850617480247,-0.00909823976109972,
-0.2608));
#52133=CARTESIAN_POINT('Ctrl Pts',(-0.0213170383639359,0.0528823612671139,
-0.2608));
#52134=CARTESIAN_POINT('Ctrl Pts',(-0.0374176429429495,0.0462851352608232,
-0.259090899643908));
#52135=CARTESIAN_POINT('Ctrl Pts',(-0.0541851500158396,0.0276036057596925,
-0.256886440469423));
#52136=CARTESIAN_POINT('Ctrl Pts',(-0.0569449337627208,0.00510999790404281,
-0.254681981294937));
#52137=CARTESIAN_POINT('Ctrl Pts',(-0.0569006472781276,4.53843407899964E-5,
-0.254186622476544));
#52138=CARTESIAN_POINT('Origin',(-8.56069748352724E-18,0.,-0.2608));
#52139=CARTESIAN_POINT('Ctrl Pts',(0.0402078774433248,-0.0657264351496036,
-0.2608));
#52140=CARTESIAN_POINT('Ctrl Pts',(0.03840501184466,-0.0665514984825666,
-0.2608));
#52141=CARTESIAN_POINT('Ctrl Pts',(0.0365711080731641,-0.0673004738245226,
-0.2608));
#52142=CARTESIAN_POINT('Ctrl Pts',(0.0347085406762429,-0.0679692337987251,
-0.2608));
#52143=CARTESIAN_POINT('Ctrl Pts',(0.0307574340573107,-0.0693878895557819,
-0.2608));
#52144=CARTESIAN_POINT('Ctrl Pts',(0.0266771922882156,-0.0704462029385511,
-0.2608));
#52145=CARTESIAN_POINT('Ctrl Pts',(0.0225169930888394,-0.0711480516798359,
-0.2608));
#52146=CARTESIAN_POINT('Ctrl Pts',(0.0198505558885779,-0.0715978944645273,
-0.2608));
#52147=CARTESIAN_POINT('Ctrl Pts',(0.0171522231608511,-0.071900485047978,
-0.2608));
#52148=CARTESIAN_POINT('Ctrl Pts',(0.0144480376767543,-0.0720557703186741,
-0.2608));
#52149=CARTESIAN_POINT('Ctrl Pts',(0.00963208362378582,-0.0723323218840802,
-0.2608));
#52150=CARTESIAN_POINT('Ctrl Pts',(0.00478610537538501,-0.0721447195123662,
-0.2608));
#52151=CARTESIAN_POINT('Ctrl Pts',(-1.05853114393216E-5,-0.0714926725959277,
-0.2608));
#52152=CARTESIAN_POINT('Ctrl Pts',(-0.00238310774834253,-0.0711701594217067,
-0.2608));
#52153=CARTESIAN_POINT('Ctrl Pts',(-0.00473375942598217,-0.0707350657326281,
-0.2608));
#52154=CARTESIAN_POINT('Ctrl Pts',(-0.00705229055096965,-0.0701887458749432,
-0.2608));
#52155=CARTESIAN_POINT('Ctrl Pts',(-0.0125588485324242,-0.0688912252420131,
-0.2608));
#52156=CARTESIAN_POINT('Ctrl Pts',(-0.0178885952542184,-0.0669682018600874,
-0.2608));
#52157=CARTESIAN_POINT('Ctrl Pts',(-0.0228999257528728,-0.0644110854236582,
-0.2608));
#52158=CARTESIAN_POINT('Ctrl Pts',(-0.025169697563011,-0.063252895836241,
-0.2608));
#52159=CARTESIAN_POINT('Ctrl Pts',(-0.0273743491726387,-0.0619629919729461,
-0.2608));
#52160=CARTESIAN_POINT('Ctrl Pts',(-0.0294830145775675,-0.0605508776511837,
-0.2608));
#52161=CARTESIAN_POINT('Ctrl Pts',(-0.0308512530790306,-0.0596346065448305,
-0.2608));
#52162=CARTESIAN_POINT('Ctrl Pts',(-0.0321808825317382,-0.0586660307193501,
-0.2608));
#52163=CARTESIAN_POINT('Ctrl Pts',(-0.0334682470120922,-0.057644991907959,
-0.2608));
#52164=CARTESIAN_POINT('Ctrl Pts',(-0.0359842192458113,-0.0556495156165024,
-0.2608));
#52165=CARTESIAN_POINT('Ctrl Pts',(-0.038339074216195,-0.0534537337051408,
-0.2608));
#52166=CARTESIAN_POINT('Ctrl Pts',(-0.0405192125274857,-0.0510820654044234,
-0.2608));
#52167=CARTESIAN_POINT('Ctrl Pts',(-0.0420374569847095,-0.0494304398019148,
-0.2608));
#52168=CARTESIAN_POINT('Ctrl Pts',(-0.0434720119114289,-0.0476918885002342,
-0.2608));
#52169=CARTESIAN_POINT('Ctrl Pts',(-0.0448131165510465,-0.0458794128670817,
-0.2608));
#52170=CARTESIAN_POINT('Ctrl Pts',(-0.0480480989637234,-0.0415073999581369,
-0.2608));
#52171=CARTESIAN_POINT('Ctrl Pts',(-0.0507184359083405,-0.0367411900030903,
-0.2608));
#52172=CARTESIAN_POINT('Ctrl Pts',(-0.0527554915500067,-0.031704765903902,
-0.2608));
#52173=CARTESIAN_POINT('Ctrl Pts',(-0.053582489134558,-0.0296600939373581,
-0.2608));
#52174=CARTESIAN_POINT('Ctrl Pts',(-0.0543045290184477,-0.027570818899863,
-0.2608));
#52175=CARTESIAN_POINT('Ctrl Pts',(-0.0549145299902943,-0.0254455356779525,
-0.2608));
#52176=CARTESIAN_POINT('Ctrl Pts',(-0.0555211088708353,-0.0233321752456298,
-0.2608));
#52177=CARTESIAN_POINT('Ctrl Pts',(-0.0560143434956106,-0.0211916487578729,
-0.2608));
#52178=CARTESIAN_POINT('Ctrl Pts',(-0.0563884430537062,-0.0190366683982668,
-0.2608));
#52179=CARTESIAN_POINT('Ctrl Pts',(-0.0572390829420659,-0.0141366031272891,
-0.2608));
#52180=CARTESIAN_POINT('Ctrl Pts',(-0.0574789625599653,-0.00915308502654382,
-0.2608));
#52181=CARTESIAN_POINT('Ctrl Pts',(-0.0570218042902053,-0.00419471110367059,
-0.2608));
#52182=CARTESIAN_POINT('Ctrl Pts',(-0.0569755453692129,-0.00369298327171148,
-0.2608));
#52183=CARTESIAN_POINT('Ctrl Pts',(-0.0569221102450288,-0.00319153404867538,
-0.2608));
#52184=CARTESIAN_POINT('Ctrl Pts',(-0.0568613829974075,-0.00269049226390562,
-0.2608));
#52185=CARTESIAN_POINT('Origin',(0.,0.,-0.2608));
#52186=CARTESIAN_POINT('Origin',(0.,0.,-0.348563377523455));
#52187=CARTESIAN_POINT('Ctrl Pts',(-0.0768390318326847,-0.00363576842162216,
-0.272347005383793));
#52188=CARTESIAN_POINT('Ctrl Pts',(-0.0756297895989668,-0.0291921272748137,
-0.270494304666896));
#52189=CARTESIAN_POINT('Ctrl Pts',(-0.0457312801109783,-0.0785610117659347,
-0.266788903233103));
#52190=CARTESIAN_POINT('Ctrl Pts',(0.0413956021036019,-0.0810270855071931,
-0.261230801082413));
#52191=CARTESIAN_POINT('Ctrl Pts',(0.0904399304474149,-0.00914058864406769,
-0.255672698931724));
#52192=CARTESIAN_POINT('Ctrl Pts',(0.0567595801668698,0.0710354832281223,
-0.250114596781034));
#52193=CARTESIAN_POINT('Ctrl Pts',(-0.0289404735607893,0.0862080259423309,
-0.244556494630344));
#52194=CARTESIAN_POINT('Ctrl Pts',(-0.0881160803218006,0.0224199181711109,
-0.238998392479654));
#52195=CARTESIAN_POINT('Ctrl Pts',(-0.0666187715640982,-0.0618859388776004,
-0.233440290328965));
#52196=CARTESIAN_POINT('Ctrl Pts',(0.0158864875285228,-0.0895304755589645,
-0.227882188178275));
#52197=CARTESIAN_POINT('Ctrl Pts',(0.0838413116627435,-0.035190906921961,
-0.222324086027586));
#52198=CARTESIAN_POINT('Ctrl Pts',(0.0750265680498761,0.051370415775385,
-0.216765983876896));
#52199=CARTESIAN_POINT('Ctrl Pts',(-0.00248916725037839,0.0908939972417645,
-0.211207881726206));
#52200=CARTESIAN_POINT('Ctrl Pts',(-0.0777251105279176,0.0471876862083083,
-0.205649779575517));
#52201=CARTESIAN_POINT('Ctrl Pts',(-0.0817903384063056,-0.0397269904622011,
-0.200091677424827));
#52202=CARTESIAN_POINT('Ctrl Pts',(-0.0109620003647857,-0.0902647609758724,
-0.194533575274138));
#52203=CARTESIAN_POINT('Ctrl Pts',(0.0699038979380953,-0.0581492190409055,
-0.188975473123448));
#52204=CARTESIAN_POINT('Ctrl Pts',(0.0867605397727151,0.0272121099867807,
-0.183417370972758));
#52205=CARTESIAN_POINT('Ctrl Pts',(0.0241726471960079,0.0876559919191793,
-0.177859268822068));
#52206=CARTESIAN_POINT('Ctrl Pts',(-0.0605495384751532,0.0678354068241687,
-0.172301166671379));
#52207=CARTESIAN_POINT('Ctrl Pts',(-0.089827992392664,-0.0141004027750951,
-0.166743064520689));
#52208=CARTESIAN_POINT('Ctrl Pts',(-0.0368531383870938,-0.0831248197956735,
-0.16118496237));
#52209=CARTESIAN_POINT('Ctrl Pts',(0.0498672352218698,-0.0760338624070072,
-0.15562686021931));
#52210=CARTESIAN_POINT('Ctrl Pts',(0.0909253969415671,0.000679450155712014,
-0.15006875806862));
#52211=CARTESIAN_POINT('Ctrl Pts',(0.0487253867959945,0.0767706071593588,
-0.144510655917931));
#52212=CARTESIAN_POINT('Ctrl Pts',(-0.0380912730997252,0.0825647887933278,
-0.138952553767241));
#52213=CARTESIAN_POINT('Ctrl Pts',(-0.0900286820059233,0.0127564043178722,
-0.133394451616551));
#52214=CARTESIAN_POINT('Ctrl Pts',(-0.0595290195873821,-0.0687327088728571,
-0.127836349465862));
#52215=CARTESIAN_POINT('Ctrl Pts',(0.0254799164407697,-0.0872849547153862,
-0.122278247315172));
#52216=CARTESIAN_POINT('Ctrl Pts',(0.0871575130564052,-0.0259124931070623,
-0.116720145164483));
#52217=CARTESIAN_POINT('Ctrl Pts',(0.0690270987348237,0.059187406728918,
-0.111162043013793));
#52218=CARTESIAN_POINT('Ctrl Pts',(-0.0123097505872792,0.0900908409118009,
-0.105603940863103));
#52219=CARTESIAN_POINT('Ctrl Pts',(-0.0823748575161993,0.0385002841254505,
-0.100045838712414));
#52220=CARTESIAN_POINT('Ctrl Pts',(-0.0770113205312119,-0.0483440410168286,
-0.0944877365617239));
#52221=CARTESIAN_POINT('Ctrl Pts',(-0.0011303800594704,-0.0909209130646338,
-0.0889296344110343));
#52222=CARTESIAN_POINT('Ctrl Pts',(0.0757855973555288,-0.0502437046352328,
-0.0833715322603447));
#52223=CARTESIAN_POINT('Ctrl Pts',(0.08330659564698,0.0364404122882757,
-0.0778134301096549));
#52224=CARTESIAN_POINT('Ctrl Pts',(0.0145456849523811,0.0897569845586842,
-0.0722553279589654));
#52225=CARTESIAN_POINT('Ctrl Pts',(-0.0675341875961008,0.0608851709532417,
-0.0666972258082757));
#52226=CARTESIAN_POINT('Ctrl Pts',(-0.0877749673282103,-0.0237375187986834,
-0.0611391236575861));
#52227=CARTESIAN_POINT('Ctrl Pts',(-0.0276417441681033,-0.0866247049612507,
-0.0555810215068964));
#52228=CARTESIAN_POINT('Ctrl Pts',(0.0578012067159718,-0.0701910676190134,
-0.0500229193562068));
#52229=CARTESIAN_POINT('Ctrl Pts',(0.0903191709888608,0.0105135099606726,
-0.0444648172055171));
#52230=CARTESIAN_POINT('Ctrl Pts',(0.040129952376398,0.0815936092947214,
-0.0389067150548276));
#52231=CARTESIAN_POINT('Ctrl Pts',(-0.0467974742865224,0.0779557101338933,
-0.0333486129041377));
#52232=CARTESIAN_POINT('Ctrl Pts',(-0.0908884149763414,0.00294461710323904,
-0.0277905107534482));
#52233=CARTESIAN_POINT('Ctrl Pts',(-0.0517269167922935,-0.0747797826777754,
-0.0222324086027586));
#52234=CARTESIAN_POINT('Ctrl Pts',(0.034746178488519,-0.0839978241416842,
-0.0166743064520689));
#52235=CARTESIAN_POINT('Ctrl Pts',(0.0895054655926491,-0.0163632542103587,
-0.0111162043013793));
#52236=CARTESIAN_POINT('Ctrl Pts',(0.0621043605299032,0.0663794467696732,
-0.0055581021506896));
#52237=CARTESIAN_POINT('Ctrl Pts',(0.00622569384473579,0.0808287455412029,
-0.00185270071689654));
#52238=CARTESIAN_POINT('Ctrl Pts',(-0.0186000842079609,0.0746424309120273,
0.));
#52239=CARTESIAN_POINT('Ctrl Pts',(-0.070179815554259,-0.00332067636904975,
-0.268498003589195));
#52240=CARTESIAN_POINT('Ctrl Pts',(-0.0690753716941705,-0.0266622061590246,
-0.266645302872298));
#52241=CARTESIAN_POINT('Ctrl Pts',(-0.0417680015833232,-0.0717525609574906,
-0.262939901438505));
#52242=CARTESIAN_POINT('Ctrl Pts',(0.0378080729428522,-0.0740049136508661,
-0.257381799287816));
#52243=CARTESIAN_POINT('Ctrl Pts',(0.0826019990902562,-0.00834842409902848,
-0.251823697137126));
#52244=CARTESIAN_POINT('Ctrl Pts',(0.0518405395284235,0.0648792285880511,
-0.246265594986436));
#52245=CARTESIAN_POINT('Ctrl Pts',(-0.0264323618883129,0.0787368504733823,
-0.240707492835747));
#52246=CARTESIAN_POINT('Ctrl Pts',(-0.0804795442739791,0.020476907171556,
-0.235149390685057));
#52247=CARTESIAN_POINT('Ctrl Pts',(-0.0608452890322729,-0.0565226249243906,
-0.229591288534368));
#52248=CARTESIAN_POINT('Ctrl Pts',(0.0145096930292469,-0.0817713616550351,
-0.224033186383678));
#52249=CARTESIAN_POINT('Ctrl Pts',(0.0765752463036064,-0.0321411045671164,
-0.218475084232988));
#52250=CARTESIAN_POINT('Ctrl Pts',(0.0685244280390537,0.0469184243746368,
-0.212916982082298));
#52251=CARTESIAN_POINT('Ctrl Pts',(-0.00227344481507348,0.0830167144128823,
-0.207358879931609));
#52252=CARTESIAN_POINT('Ctrl Pts',(-0.0709891026823609,0.0430981889743522,
-0.201800777780919));
#52253=CARTESIAN_POINT('Ctrl Pts',(-0.0747020196190622,-0.0362840706951381,
-0.19624267563023));
#52254=CARTESIAN_POINT('Ctrl Pts',(-0.0100119840835777,-0.0824420105933897,
-0.19068457347954));
#52255=CARTESIAN_POINT('Ctrl Pts',(0.0638457115714528,-0.0531097460441851,
-0.185126471328851));
#52256=CARTESIAN_POINT('Ctrl Pts',(0.0792414809688833,0.0248537860793576,
-0.179568369178161));
#52257=CARTESIAN_POINT('Ctrl Pts',(0.0220777368117798,0.0800593292027518,
-0.174010267027471));
#52258=CARTESIAN_POINT('Ctrl Pts',(-0.0553020429946938,0.0619564852057811,
-0.168452164876781));
#52259=CARTESIAN_POINT('Ctrl Pts',(-0.0820430943410844,-0.0128783984180293,
-0.162894062726092));
#52260=CARTESIAN_POINT('Ctrl Pts',(-0.0336592795733491,-0.0759208488459889,
-0.157335960575402));
#52261=CARTESIAN_POINT('Ctrl Pts',(0.0455455162122831,-0.0694444257343166,
-0.151777858424713));
#52262=CARTESIAN_POINT('Ctrl Pts',(0.0830453928733998,0.00062056594765577,
-0.146219756274023));
#52263=CARTESIAN_POINT('Ctrl Pts',(0.0445026255093734,0.0701173208710384,
-0.140661654123333));
#52264=CARTESIAN_POINT('Ctrl Pts',(-0.0347901119601109,0.0754093526504762,
-0.135103551972643));
#52265=CARTESIAN_POINT('Ctrl Pts',(-0.0822263912893447,0.0116508769151748,
-0.129545449821954));
#52266=CARTESIAN_POINT('Ctrl Pts',(-0.0543699668661269,-0.0627760230210226,
-0.123987347671264));
#52267=CARTESIAN_POINT('Ctrl Pts',(0.0232717122210088,-0.0797204477527267,
-0.118429245520575));
#52268=CARTESIAN_POINT('Ctrl Pts',(0.0796040507614075,-0.0236667998467815,
-0.112871143369885));
#52269=CARTESIAN_POINT('Ctrl Pts',(0.0630448997327806,0.054057959715254,
-0.107313041219195));
#52270=CARTESIAN_POINT('Ctrl Pts',(-0.0112429322068414,0.0822831632247203,
-0.101754939068506));
#52271=CARTESIAN_POINT('Ctrl Pts',(-0.0752358816725248,0.0351636762497748,
-0.0961968369178162));
#52272=CARTESIAN_POINT('Ctrl Pts',(-0.0703371729388632,-0.0441543288715073,
-0.0906387347671264));
#52273=CARTESIAN_POINT('Ctrl Pts',(-0.001032416236745,-0.0830412975894191,
-0.0850806326164368));
#52274=CARTESIAN_POINT('Ctrl Pts',(0.0692176764494058,-0.0458893590921511,
-0.0795225304657471));
#52275=CARTESIAN_POINT('Ctrl Pts',(0.0760868711840199,0.0332823221755449,
-0.0739644283150575));
#52276=CARTESIAN_POINT('Ctrl Pts',(0.0132850904380373,0.0819782403655364,
-0.0684063261643678));
#52277=CARTESIAN_POINT('Ctrl Pts',(-0.0616813709915206,0.0556085880518666,
-0.0628482240136782));
#52278=CARTESIAN_POINT('Ctrl Pts',(-0.0801679936674403,-0.0216803185994695,
-0.0572901218629885));
#52279=CARTESIAN_POINT('Ctrl Pts',(-0.0252461862291492,-0.0791174182134443,
-0.0517320197122989));
#52280=CARTESIAN_POINT('Ctrl Pts',(0.0527918940334048,-0.0641079938355434,
-0.0461739175616093));
#52281=CARTESIAN_POINT('Ctrl Pts',(0.0824917051898045,0.00960236187611665,
-0.0406158154109197));
#52282=CARTESIAN_POINT('Ctrl Pts',(0.0366521101164998,0.0745223399375795,
-0.0350577132602299));
#52283=CARTESIAN_POINT('Ctrl Pts',(-0.0427417945736834,0.0711997174887719,
-0.0294996111095404));
#52284=CARTESIAN_POINT('Ctrl Pts',(-0.0830116159317013,0.00268942333413568,
-0.0239415089588506));
#52285=CARTESIAN_POINT('Ctrl Pts',(-0.0472440294091458,-0.068299030197847,
-0.0183834068081611));
#52286=CARTESIAN_POINT('Ctrl Pts',(0.031734918301019,-0.0767181947068073,
-0.0128253046574713));
#52287=CARTESIAN_POINT('Ctrl Pts',(0.0817485191649469,-0.0149451409649585,
-0.0072672025067818));
#52288=CARTESIAN_POINT('Ctrl Pts',(0.0567221171733953,0.0606267052015075,
-0.00170910035609209));
#52289=CARTESIAN_POINT('Ctrl Pts',(0.00568614720019127,0.0738237627188692,
0.00199630107770095));
#52290=CARTESIAN_POINT('Ctrl Pts',(-0.0169881172091128,0.0681735819542088,
0.0038490017945975));
#52291=CARTESIAN_POINT('Ctrl Pts',(-0.0635205992758333,-0.00300558431647733,
-0.264649001794598));
#52292=CARTESIAN_POINT('Ctrl Pts',(-0.0625209537893743,-0.0241322850432355,
-0.262796301077701));
#52293=CARTESIAN_POINT('Ctrl Pts',(-0.0378047230556681,-0.0649441101490466,
-0.259090899643908));
#52294=CARTESIAN_POINT('Ctrl Pts',(0.0342205437821026,-0.066982741794539,
-0.253532797493218));
#52295=CARTESIAN_POINT('Ctrl Pts',(0.0747640677330976,-0.00755625955398936,
-0.247974695342529));
#52296=CARTESIAN_POINT('Ctrl Pts',(0.0469214988899772,0.05872297394798,
-0.242416593191839));
#52297=CARTESIAN_POINT('Ctrl Pts',(-0.0239242502158365,0.0712656750044335,
-0.23685849104115));
#52298=CARTESIAN_POINT('Ctrl Pts',(-0.0728430082261576,0.0185338961720012,
-0.231300388890459));
#52299=CARTESIAN_POINT('Ctrl Pts',(-0.0550718065004475,-0.051159310971181,
-0.22574228673977));
#52300=CARTESIAN_POINT('Ctrl Pts',(0.013132898529971,-0.0740122477511057,
-0.22018418458908));
#52301=CARTESIAN_POINT('Ctrl Pts',(0.0693091809444694,-0.0290913022122718,
-0.214626082438391));
#52302=CARTESIAN_POINT('Ctrl Pts',(0.0620222880282312,0.0424664329738887,
-0.209067980287701));
#52303=CARTESIAN_POINT('Ctrl Pts',(-0.00205772237976836,0.075139431584,
-0.203509878137012));
#52304=CARTESIAN_POINT('Ctrl Pts',(-0.0642530948368044,0.0390086917403961,
-0.197951775986322));
#52305=CARTESIAN_POINT('Ctrl Pts',(-0.0676137008318185,-0.032841150928075,
-0.192393673835632));
#52306=CARTESIAN_POINT('Ctrl Pts',(-0.00906196780236982,-0.074619260210907,
-0.186835571684942));
#52307=CARTESIAN_POINT('Ctrl Pts',(0.0577875252048107,-0.0480702730474647,
-0.181277469534253));
#52308=CARTESIAN_POINT('Ctrl Pts',(0.0717224221650512,0.0224954621719345,
-0.175719367383563));
#52309=CARTESIAN_POINT('Ctrl Pts',(0.019982826427552,0.0724626664863242,
-0.170161265232874));
#52310=CARTESIAN_POINT('Ctrl Pts',(-0.0500545475142344,0.0560775635873935,
-0.164603163082184));
#52311=CARTESIAN_POINT('Ctrl Pts',(-0.0742581962895047,-0.0116563940609636,
-0.159045060931494));
#52312=CARTESIAN_POINT('Ctrl Pts',(-0.0304654207596044,-0.0687168778963044,
-0.153486958780805));
#52313=CARTESIAN_POINT('Ctrl Pts',(0.0412237972026965,-0.062854989061626,
-0.147928856630115));
#52314=CARTESIAN_POINT('Ctrl Pts',(0.0751653888052323,0.000561681739599467,
-0.142370754479425));
#52315=CARTESIAN_POINT('Ctrl Pts',(0.0402798642227526,0.0634640345827179,
-0.136812652328736));
#52316=CARTESIAN_POINT('Ctrl Pts',(-0.0314889508204967,0.0682539165076246,
-0.131254550178046));
#52317=CARTESIAN_POINT('Ctrl Pts',(-0.074424100572766,0.0105453495124774,
-0.125696448027356));
#52318=CARTESIAN_POINT('Ctrl Pts',(-0.0492109141448716,-0.0568193371691881,
-0.120138345876667));
#52319=CARTESIAN_POINT('Ctrl Pts',(0.0210635080012477,-0.0721559407900673,
-0.114580243725977));
#52320=CARTESIAN_POINT('Ctrl Pts',(0.0720505884664099,-0.0214211065865007,
-0.109022141575287));
#52321=CARTESIAN_POINT('Ctrl Pts',(0.0570627007307374,0.0489285127015899,
-0.103464039424598));
#52322=CARTESIAN_POINT('Ctrl Pts',(-0.0101761138264036,0.0744754855376397,
-0.0979059372739082));
#52323=CARTESIAN_POINT('Ctrl Pts',(-0.0680969058288505,0.0318270683740991,
-0.0923478351232185));
#52324=CARTESIAN_POINT('Ctrl Pts',(-0.0636630253465145,-0.039964616726186,
-0.086789732972529));
#52325=CARTESIAN_POINT('Ctrl Pts',(-0.00093445241401957,-0.0751616821142043,
-0.0812316308218392));
#52326=CARTESIAN_POINT('Ctrl Pts',(0.0626497555432827,-0.0415350135490693,
-0.0756735286711497));
#52327=CARTESIAN_POINT('Ctrl Pts',(0.0688671467210598,0.030124232062814,
-0.0701154265204599));
#52328=CARTESIAN_POINT('Ctrl Pts',(0.0120244959236936,0.0741994961723886,
-0.0645573243697704));
#52329=CARTESIAN_POINT('Ctrl Pts',(-0.0558285543869405,0.0503320051504913,
-0.0589992222190807));
#52330=CARTESIAN_POINT('Ctrl Pts',(-0.0725610200066702,-0.0196231184002554,
-0.0534411200683911));
#52331=CARTESIAN_POINT('Ctrl Pts',(-0.0228506282901951,-0.0716101314656381,
-0.0478830179177014));
#52332=CARTESIAN_POINT('Ctrl Pts',(0.0477825813508377,-0.0580249200520732,
-0.0423249157670118));
#52333=CARTESIAN_POINT('Ctrl Pts',(0.0746642393907483,0.00869121379156067,
-0.0367668136163221));
#52334=CARTESIAN_POINT('Ctrl Pts',(0.0331742678566015,0.0674510705804377,
-0.0312087114656325));
#52335=CARTESIAN_POINT('Ctrl Pts',(-0.0386861148608444,0.0644437248436505,
-0.0256506093149428));
#52336=CARTESIAN_POINT('Ctrl Pts',(-0.0751348168870612,0.00243422956503228,
-0.0200925071642532));
#52337=CARTESIAN_POINT('Ctrl Pts',(-0.0427611420259981,-0.0618182777179186,
-0.0145344050135636));
#52338=CARTESIAN_POINT('Ctrl Pts',(0.0287236581135189,-0.0694385652719304,
-0.00897630286287385));
#52339=CARTESIAN_POINT('Ctrl Pts',(0.0739915727372447,-0.0135270277195584,
-0.00341820071218429));
#52340=CARTESIAN_POINT('Ctrl Pts',(0.0513398738168874,0.0548739636333419,
0.0021399014385054));
#52341=CARTESIAN_POINT('Ctrl Pts',(0.00514660055564675,0.0668187798965355,
0.00584530287229846));
#52342=CARTESIAN_POINT('Ctrl Pts',(-0.0153761502102646,0.0617047329963903,
0.007698003589195));
#52343=CARTESIAN_POINT('Ctrl Pts',(-0.0568613829974075,-0.00269049226390492,
-0.2608));
#52344=CARTESIAN_POINT('Ctrl Pts',(-0.0559665358845781,-0.0216023639274464,
-0.258947299283104));
#52345=CARTESIAN_POINT('Ctrl Pts',(-0.0338414445280129,-0.0581356593406026,
-0.255241897849311));
#52346=CARTESIAN_POINT('Ctrl Pts',(0.030633014621353,-0.0599605699382118,
-0.249683795698621));
#52347=CARTESIAN_POINT('Ctrl Pts',(0.0669261363759389,-0.00676409500895024,
-0.244125693547931));
#52348=CARTESIAN_POINT('Ctrl Pts',(0.0420024582515309,0.0525667193079089,
-0.238567591397241));
#52349=CARTESIAN_POINT('Ctrl Pts',(-0.0214161385433601,0.0637944995354849,
-0.233009489246552));
#52350=CARTESIAN_POINT('Ctrl Pts',(-0.0652064721783362,0.0165908851724463,
-0.227451387095862));
#52351=CARTESIAN_POINT('Ctrl Pts',(-0.0492983239686221,-0.0457959970179712,
-0.221893284945172));
#52352=CARTESIAN_POINT('Ctrl Pts',(0.011756104030695,-0.0662531338471764,
-0.216335182794483));
#52353=CARTESIAN_POINT('Ctrl Pts',(0.0620431155853323,-0.0260414998574271,
-0.210777080643793));
#52354=CARTESIAN_POINT('Ctrl Pts',(0.0555201480174088,0.0380144415731405,
-0.205218978493103));
#52355=CARTESIAN_POINT('Ctrl Pts',(-0.00184199994446337,0.0672621487551179,
-0.199660876342414));
#52356=CARTESIAN_POINT('Ctrl Pts',(-0.0575170869912477,0.0349191945064401,
-0.194102774191724));
#52357=CARTESIAN_POINT('Ctrl Pts',(-0.060525382044575,-0.029398231161012,
-0.188544672041035));
#52358=CARTESIAN_POINT('Ctrl Pts',(-0.00811195152116181,-0.0667965098284243,
-0.182986569890345));
#52359=CARTESIAN_POINT('Ctrl Pts',(0.0517293388381684,-0.0430308000507443,
-0.177428467739655));
#52360=CARTESIAN_POINT('Ctrl Pts',(0.0642033633612193,0.0201371382645114,
-0.171870365588966));
#52361=CARTESIAN_POINT('Ctrl Pts',(0.0178879160433239,0.0648660037698966,
-0.166312263438276));
#52362=CARTESIAN_POINT('Ctrl Pts',(-0.0448070520337749,0.0501986419690058,
-0.160754161287587));
#52363=CARTESIAN_POINT('Ctrl Pts',(-0.0664732982379252,-0.0104343897038979,
-0.155196059136897));
#52364=CARTESIAN_POINT('Ctrl Pts',(-0.0272715619458597,-0.0615129069466198,
-0.149637956986207));
#52365=CARTESIAN_POINT('Ctrl Pts',(0.0369020781931099,-0.0562655523889355,
-0.144079854835517));
#52366=CARTESIAN_POINT('Ctrl Pts',(0.0672853847370649,0.000502797531543261,
-0.138521752684828));
#52367=CARTESIAN_POINT('Ctrl Pts',(0.0360571029361317,0.0568107482943974,
-0.132963650534138));
#52368=CARTESIAN_POINT('Ctrl Pts',(-0.0281877896808826,0.0610984803647731,
-0.127405548383449));
#52369=CARTESIAN_POINT('Ctrl Pts',(-0.0666218098561871,0.00943982210977994,
-0.121847446232759));
#52370=CARTESIAN_POINT('Ctrl Pts',(-0.0440518614236164,-0.0508626513173536,
-0.116289344082069));
#52371=CARTESIAN_POINT('Ctrl Pts',(0.0188553037814868,-0.0645914338274078,
-0.110731241931379));
#52372=CARTESIAN_POINT('Ctrl Pts',(0.0644971261714122,-0.0191754133262199,
-0.10517313978069));
#52373=CARTESIAN_POINT('Ctrl Pts',(0.0510805017286943,0.0437990656879258,
-0.0996150376300002));
#52374=CARTESIAN_POINT('Ctrl Pts',(-0.00910929544596579,0.0666678078505591,
-0.0940569354793109));
#52375=CARTESIAN_POINT('Ctrl Pts',(-0.060957929985176,0.0284904604984234,
-0.0884988333286209));
#52376=CARTESIAN_POINT('Ctrl Pts',(-0.0569888777541658,-0.0357749045808647,
-0.0829407311779316));
#52377=CARTESIAN_POINT('Ctrl Pts',(-0.000836488591294147,-0.0672820666389896,
-0.0773826290272417));
#52378=CARTESIAN_POINT('Ctrl Pts',(0.0560818346371597,-0.0371806680059875,
-0.0718245268765522));
#52379=CARTESIAN_POINT('Ctrl Pts',(0.0616474222580996,0.0269661419500831,
-0.0662664247258625));
#52380=CARTESIAN_POINT('Ctrl Pts',(0.0107639014093499,0.0664207519792408,
-0.0607083225751728));
#52381=CARTESIAN_POINT('Ctrl Pts',(-0.0499757377823604,0.045055422249116,
-0.0551502204244832));
#52382=CARTESIAN_POINT('Ctrl Pts',(-0.0649540463459001,-0.0175659182010413,
-0.0495921182737936));
#52383=CARTESIAN_POINT('Ctrl Pts',(-0.0204550703512412,-0.0641028447178318,
-0.0440340161231039));
#52384=CARTESIAN_POINT('Ctrl Pts',(0.0427732686682708,-0.0519418462686033,
-0.0384759139724143));
#52385=CARTESIAN_POINT('Ctrl Pts',(0.0668367735916919,0.00778006570700472,
-0.0329178118217246));
#52386=CARTESIAN_POINT('Ctrl Pts',(0.0296964255967034,0.0603798012232959,
-0.027359709671035));
#52387=CARTESIAN_POINT('Ctrl Pts',(-0.0346304351480055,0.0576877321985291,
-0.0218016075203453));
#52388=CARTESIAN_POINT('Ctrl Pts',(-0.067258017842421,0.00217903579592891,
-0.0162435053696557));
#52389=CARTESIAN_POINT('Ctrl Pts',(-0.0382782546428504,-0.0553375252379902,
-0.0106854032189661));
#52390=CARTESIAN_POINT('Ctrl Pts',(0.0257123979260188,-0.0621589358370536,
-0.00512730106827636));
#52391=CARTESIAN_POINT('Ctrl Pts',(0.0662346263095425,-0.0121089144741581,
0.000430801082413216));
#52392=CARTESIAN_POINT('Ctrl Pts',(0.0459576304603796,0.0491212220651762,
0.00598890323310289));
#52393=CARTESIAN_POINT('Ctrl Pts',(0.00460705391110222,0.0598137970742019,
0.00969430466689595));
#52394=CARTESIAN_POINT('Ctrl Pts',(-0.0137641832114165,0.0552358840385719,
0.0115470053837925));
#52395=CARTESIAN_POINT('',(-0.0186000842079609,0.0746424309120273,0.));
#52396=CARTESIAN_POINT('Ctrl Pts',(0.0551371004056304,-0.0145210214852671,
-1.38777878078145E-17));
#52397=CARTESIAN_POINT('Ctrl Pts',(0.0557629658139121,-0.0131629595984533,
-1.70794074384518E-17));
#52398=CARTESIAN_POINT('Ctrl Pts',(0.0563303031086066,-0.0117815320725005,
-9.07936409284168E-17));
#52399=CARTESIAN_POINT('Ctrl Pts',(0.0568367962277587,-0.0103798601340677,
-8.84708972748172E-17));
#52400=CARTESIAN_POINT('Ctrl Pts',(0.0579324744939598,-0.00734767386892008,
-8.52714485894961E-17));
#52401=CARTESIAN_POINT('Ctrl Pts',(0.0587439674756155,-0.00422113471852991,
-5.91471153565421E-17));
#52402=CARTESIAN_POINT('Ctrl Pts',(0.0592872651796402,-0.00103525413784158,
-5.72458747072346E-17));
#52403=CARTESIAN_POINT('Ctrl Pts',(0.0596976535666042,0.00137125040448081,
-5.58097429556742E-17));
#52404=CARTESIAN_POINT('Ctrl Pts',(0.0599540529871003,0.00381003129288719,
1.13065255910782E-17));
#52405=CARTESIAN_POINT('Ctrl Pts',(0.0600621304227767,0.00625467285507289,
8.67361737988404E-18));
#52406=CARTESIAN_POINT('Ctrl Pts',(0.0602044555315557,0.00947397459077743,
5.20639089344986E-18));
#52407=CARTESIAN_POINT('Ctrl Pts',(0.0600908652691288,0.0127087915017173,
-8.32645063813673E-17));
#52408=CARTESIAN_POINT('Ctrl Pts',(0.0597334763142803,0.0159280092132275,
-7.97972798949331E-17));
#52409=CARTESIAN_POINT('Ctrl Pts',(0.0594787929043323,0.0182220961820871,
-7.73264562932321E-17));
#52410=CARTESIAN_POINT('Ctrl Pts',(0.0591000457868719,0.0205057594111829,
-8.69735018148149E-17));
#52411=CARTESIAN_POINT('Ctrl Pts',(0.058604046859906,0.022757306393025,
-6.93889390390723E-17));
#52412=CARTESIAN_POINT('Ctrl Pts',(0.0574000150098037,0.0282229115198812,
-2.67026094906683E-17));
#52413=CARTESIAN_POINT('Ctrl Pts',(0.0555070346110573,0.0335164792257551,
6.58435981494048E-17));
#52414=CARTESIAN_POINT('Ctrl Pts',(0.0529715910690817,0.0384899104332707,
7.89299181569447E-17));
#52415=CARTESIAN_POINT('Ctrl Pts',(0.0519200213889706,0.0405526301812588,
8.43574408433455E-17));
#52416=CARTESIAN_POINT('Ctrl Pts',(0.0507562550697398,0.0425610151284201,
-1.69820238630303E-17));
#52417=CARTESIAN_POINT('Ctrl Pts',(0.0494920486484344,0.0444901026849085,
-1.90819582357449E-17));
#52418=CARTESIAN_POINT('Ctrl Pts',(0.0484341874343681,0.0461043223804862,
-2.08391389362553E-17));
#52419=CARTESIAN_POINT('Ctrl Pts',(0.0473048627097976,0.0476654962951114,
-6.98109579163092E-18));
#52420=CARTESIAN_POINT('Ctrl Pts',(0.0461061165839465,0.0491679074422925,
7.80625564189563E-18));
#52421=CARTESIAN_POINT('Ctrl Pts',(0.0432012619200474,0.0528086166248848,
4.35741111720786E-17));
#52422=CARTESIAN_POINT('Ctrl Pts',(0.0398903515469501,0.0561051665186203,
5.00499939764873E-17));
#52423=CARTESIAN_POINT('Ctrl Pts',(0.0362500452078145,0.0590443888276636,
4.33680868994202E-17));
#52424=CARTESIAN_POINT('Ctrl Pts',(0.0345220116191685,0.0604396216463748,
4.01962220095754E-17));
#52425=CARTESIAN_POINT('Ctrl Pts',(0.0327198952772362,0.0617532349568333,
5.64086294081436E-17));
#52426=CARTESIAN_POINT('Ctrl Pts',(0.0308627900046538,0.0629764406192712,
4.85722573273506E-17));
#52427=CARTESIAN_POINT('Ctrl Pts',(0.0270012557184676,0.0655198885725436,
3.22778555419218E-17));
#52428=CARTESIAN_POINT('Ctrl Pts',(0.0228917503466347,0.0676826925597205,
-5.93019284099973E-17));
#52429=CARTESIAN_POINT('Ctrl Pts',(0.0186045273957792,0.0694528091662133,
-6.93889390390723E-17));
#52430=CARTESIAN_POINT('Ctrl Pts',(0.0161676416790297,0.070458955085096,
-7.51224622097737E-17));
#52431=CARTESIAN_POINT('Ctrl Pts',(0.0136730221737058,0.0713380460700889,
1.16527597969391E-16));
#52432=CARTESIAN_POINT('Ctrl Pts',(0.0111317204605169,0.0720860061518305,
1.28803218091278E-16));
#52433=CARTESIAN_POINT('Ctrl Pts',(0.00894815151273096,0.0727286777402524,
1.39350829488168E-16));
#52434=CARTESIAN_POINT('Ctrl Pts',(0.00673480985803829,0.0732728638103404,
3.27324123811703E-17));
#52435=CARTESIAN_POINT('Ctrl Pts',(0.00450708731124494,0.0737153773487098,
3.16587034365767E-17));
#52436=CARTESIAN_POINT('Ctrl Pts',(-0.00167643327094307,0.0749436683566466,
2.8678394525249E-17));
#52437=CARTESIAN_POINT('Ctrl Pts',(-0.00798645148332497,0.0753972328474082,
-6.20569042812721E-17));
#52438=CARTESIAN_POINT('Ctrl Pts',(-0.0142744840883698,0.0750281955405284,
-6.74915852372227E-17));
#52439=CARTESIAN_POINT('Ctrl Pts',(-0.0157179901554196,0.0749434778514024,
-6.87391924659289E-17));
#52440=CARTESIAN_POINT('Ctrl Pts',(-0.0171604219804116,0.0748152105438323,
-2.91779109939374E-18));
#52441=CARTESIAN_POINT('Ctrl Pts',(-0.0186000842079609,0.0746424309120273,
0.));
#52442=CARTESIAN_POINT('Ctrl Pts',(-0.0186000842079609,0.0746424309120273,
0.));
#52443=CARTESIAN_POINT('Ctrl Pts',(0.00622569384473562,0.0808287455412029,
-0.00185270071689653));
#52444=CARTESIAN_POINT('Ctrl Pts',(0.0341650271873191,0.0736040961554381,
-0.00370540143379305));
#52445=CARTESIAN_POINT('Ctrl Pts',(0.0527015447024019,0.0562013212992173,
-0.00555810215068958));
#52446=CARTESIAN_POINT('Ctrl Pts',(0.071238062217485,0.0387985464429963,
-0.00741080286758614));
#52447=CARTESIAN_POINT('Ctrl Pts',(0.0803717639050671,0.0112176461163188,
-0.00926350358448272));
#52448=CARTESIAN_POINT('Ctrl Pts',(0.0758120668981698,-0.0138452323689076,
-0.0111162043013793));
#52449=CARTESIAN_POINT('Ctrl Pts',(0.0712523698912725,-0.0389081108541336,
-0.0129689050182758));
#52450=CARTESIAN_POINT('Ctrl Pts',(0.0529992741898961,-0.0614529674979086,
-0.0148216057351723));
#52451=CARTESIAN_POINT('Ctrl Pts',(0.0294605437924059,-0.0711890555758115,
-0.0166743064520688));
#52452=CARTESIAN_POINT('Ctrl Pts',(0.00592181339491531,-0.0809251436537147,
-0.0185270071689654));
#52453=CARTESIAN_POINT('Ctrl Pts',(-0.0229025516986893,-0.0778524631657451,
-0.020379707885862));
#52454=CARTESIAN_POINT('Ctrl Pts',(-0.0438416506094996,-0.063362056291591,
-0.0222324086027586));
#52455=CARTESIAN_POINT('Ctrl Pts',(-0.0641021519188406,-0.0493412567960065,
-0.0240250667042551));
#52456=CARTESIAN_POINT('Ctrl Pts',(-0.0769801991262393,-0.0246307939408685,
-0.0258177248057515));
#52457=CARTESIAN_POINT('Ctrl Pts',(-0.0770493699172285,1.64405594954022E-5,
-0.027610382907248));
#52458=CARTESIAN_POINT('Origin',(-0.0288,-0.1152,0.0585));
#52459=CARTESIAN_POINT('',(0.0288,-0.1152,0.13));
#52460=CARTESIAN_POINT('',(-0.0288,-0.1152,0.13));
#52461=CARTESIAN_POINT('',(-0.0144,-0.1152,0.13));
#52462=CARTESIAN_POINT('',(0.0288,-0.1152,0.0585));
#52463=CARTESIAN_POINT('',(0.0288,-0.1152,0.0585));
#52464=CARTESIAN_POINT('',(-0.0288,-0.1152,0.0585));
#52465=CARTESIAN_POINT('',(-0.0288,-0.1152,0.0585));
#52466=CARTESIAN_POINT('',(-0.0288,-0.1152,0.0585));
#52467=CARTESIAN_POINT('Origin',(0.0288,-0.1152,0.0585));
#52468=CARTESIAN_POINT('',(0.0288,0.1152,0.13));
#52469=CARTESIAN_POINT('',(0.0288,0.0288,0.13));
#52470=CARTESIAN_POINT('',(0.0288,-0.0576,0.13));
#52471=CARTESIAN_POINT('',(0.0288,0.1152,0.0585));
#52472=CARTESIAN_POINT('',(0.0288,0.1152,0.0585));
#52473=CARTESIAN_POINT('',(0.0288,0.0288,0.0585));
#52474=CARTESIAN_POINT('',(0.0288,-0.1152,0.0585));
#52475=CARTESIAN_POINT('',(0.0288,0.0288,0.0585));
#52476=CARTESIAN_POINT('Origin',(-0.0288,0.1152,0.0585));
#52477=CARTESIAN_POINT('',(-0.0288,0.0288,0.13));
#52478=CARTESIAN_POINT('',(-0.0288,0.1152,0.13));
#52479=CARTESIAN_POINT('',(-0.0288,0.0576,0.13));
#52480=CARTESIAN_POINT('',(-0.0288,0.0288,0.0585));
#52481=CARTESIAN_POINT('',(-0.0288,0.0288,0.0585));
#52482=CARTESIAN_POINT('',(-0.0288,0.1152,0.0585));
#52483=CARTESIAN_POINT('',(-0.0288,0.1152,0.0585));
#52484=CARTESIAN_POINT('',(-0.0288,0.1152,0.0585));
#52485=CARTESIAN_POINT('Origin',(-0.0288,0.1152,0.0585));
#52486=CARTESIAN_POINT('',(-0.0288,-0.0288,0.13));
#52487=CARTESIAN_POINT('',(-0.0288,0.0576,0.13));
#52488=CARTESIAN_POINT('',(-0.0288,-0.0288,0.0585));
#52489=CARTESIAN_POINT('',(-0.0288,0.1152,0.0585));
#52490=CARTESIAN_POINT('',(-0.0288,-0.0288,0.0585));
#52491=CARTESIAN_POINT('Origin',(0.0288,0.1152,0.0585));
#52492=CARTESIAN_POINT('',(0.0144,0.1152,0.13));
#52493=CARTESIAN_POINT('',(0.0288,0.1152,0.0585));
#52494=CARTESIAN_POINT('Origin',(0.0288,-0.1152,0.0585));
#52495=CARTESIAN_POINT('',(0.0288,-0.0288,0.13));
#52496=CARTESIAN_POINT('',(0.0288,-0.0576,0.13));
#52497=CARTESIAN_POINT('',(0.0288,-0.0288,0.0585));
#52498=CARTESIAN_POINT('',(0.0288,-0.0288,0.0585));
#52499=CARTESIAN_POINT('',(0.0288,-0.1152,0.0585));
#52500=CARTESIAN_POINT('Origin',(0.,0.,0.13));
#52501=CARTESIAN_POINT('',(-0.1275,-1.56142466891288E-17,0.13));
#52502=CARTESIAN_POINT('Origin',(0.,0.,0.13));
#52503=CARTESIAN_POINT('',(-0.1152,-0.0288,0.13));
#52504=CARTESIAN_POINT('',(-0.0576,-0.0288,0.13));
#52505=CARTESIAN_POINT('',(-0.1152,0.0288,0.13));
#52506=CARTESIAN_POINT('',(-0.1152,0.0144,0.13));
#52507=CARTESIAN_POINT('',(0.0576,0.0288,0.13));
#52508=CARTESIAN_POINT('',(0.1152,0.0288,0.13));
#52509=CARTESIAN_POINT('',(0.0576,0.0288,0.13));
#52510=CARTESIAN_POINT('',(0.1152,-0.0288,0.13));
#52511=CARTESIAN_POINT('',(0.1152,-0.0144,0.13));
#52512=CARTESIAN_POINT('',(-0.0576,-0.0288,0.13));
#52513=CARTESIAN_POINT('Origin',(-0.1152,-0.0288,0.0585));
#52514=CARTESIAN_POINT('',(-0.1152,-0.0288,0.0585));
#52515=CARTESIAN_POINT('',(-0.1152,-0.0288,0.0585));
#52516=CARTESIAN_POINT('',(-0.1152,-0.0288,0.0585));
#52517=CARTESIAN_POINT('Origin',(0.1152,0.0288,0.0585));
#52518=CARTESIAN_POINT('',(-0.1152,0.0288,0.0585));
#52519=CARTESIAN_POINT('',(-0.1152,0.0288,0.0585));
#52520=CARTESIAN_POINT('',(0.1152,0.0288,0.0585));
#52521=CARTESIAN_POINT('Origin',(0.1152,0.0288,0.0585));
#52522=CARTESIAN_POINT('',(0.1152,0.0288,0.0585));
#52523=CARTESIAN_POINT('',(0.1152,0.0288,0.0585));
#52524=CARTESIAN_POINT('',(0.1152,0.0288,0.0585));
#52525=CARTESIAN_POINT('Origin',(-0.1152,-0.0288,0.0585));
#52526=CARTESIAN_POINT('',(0.1152,-0.0288,0.0585));
#52527=CARTESIAN_POINT('',(0.1152,-0.0288,0.0585));
#52528=CARTESIAN_POINT('',(-0.1152,-0.0288,0.0585));
#52529=CARTESIAN_POINT('Origin',(-0.1152,0.0288,0.0585));
#52530=CARTESIAN_POINT('',(-0.1152,0.0288,0.0585));
#52531=CARTESIAN_POINT('Origin',(0.1152,-0.0288,0.0585));
#52532=CARTESIAN_POINT('',(0.1152,-0.0288,0.0585));
#52533=CARTESIAN_POINT('Origin',(0.,0.,0.0585));
#52534=CARTESIAN_POINT('Origin',(0.0608,0.,-0.3));
#52535=CARTESIAN_POINT('',(-0.0608,-7.44585253881591E-18,-0.3));
#52536=CARTESIAN_POINT('Origin',(0.,0.,-0.3));
#52537=CARTESIAN_POINT('Origin',(0.,0.,-0.2904));
#52538=CARTESIAN_POINT('',(-0.0704,-8.62151346599737E-18,-0.2904));
#52539=CARTESIAN_POINT('Origin',(0.,0.,-0.1404));
#52540=CARTESIAN_POINT('Origin',(0.,0.,0.));
#52541=CARTESIAN_POINT('Origin',(0.16,0.,0.));
#52542=CARTESIAN_POINT('',(-0.16,-1.95943487863577E-17,0.));
#52543=CARTESIAN_POINT('Origin',(0.,0.,0.));
#52544=CARTESIAN_POINT('Origin',(0.,0.,0.039));
#52545=CARTESIAN_POINT('',(-0.16,-1.95943487863577E-17,0.078));
#52546=CARTESIAN_POINT('Origin',(0.,0.,0.078));
#52547=CARTESIAN_POINT('',(-0.16,-1.95943487863577E-17,0.039));
#52548=CARTESIAN_POINT('Origin',(0.,0.,0.104));
#52549=CARTESIAN_POINT('',(-0.14375,-1.76042977377432E-17,0.104));
#52550=CARTESIAN_POINT('',(0.,0.,0.));
#52551=CARTESIAN_POINT('Origin',(0.,0.,-0.2904));
#52552=CARTESIAN_POINT('',(-0.0769096047044028,6.91658437555233E-5,-0.537610382907248));
#52553=CARTESIAN_POINT('',(-0.0768915057166184,6.11931288171008E-5,-0.542639617092752));
#52554=CARTESIAN_POINT('',(-0.076925,-9.42059550244101E-18,-0.2904));
#52555=CARTESIAN_POINT('',(0.040207606550226,-0.0657262044767398,-0.5608));
#52556=CARTESIAN_POINT('Ctrl Pts',(-0.0769096047044028,6.91658437555233E-5,
-0.537610382907248));
#52557=CARTESIAN_POINT('Ctrl Pts',(-0.0769675453873495,0.00649632637372731,
-0.538075722980974));
#52558=CARTESIAN_POINT('Ctrl Pts',(-0.0762292291219459,0.012910442097877,
-0.5385410630547));
#52559=CARTESIAN_POINT('Ctrl Pts',(-0.0746430427302316,0.019107617912474,
-0.539006403128426));
#52560=CARTESIAN_POINT('Ctrl Pts',(-0.0683293317028954,0.0437750702896657,
-0.54085865880928));
#52561=CARTESIAN_POINT('Ctrl Pts',(-0.0485820861472687,0.0650053573804454,
-0.542710914490134));
#52562=CARTESIAN_POINT('Ctrl Pts',(-0.0244321386735508,0.0730771079271841,
-0.544563170170987));
#52563=CARTESIAN_POINT('Ctrl Pts',(-0.000282191199832891,0.0811488584739228,
-0.546415425851841));
#52564=CARTESIAN_POINT('Ctrl Pts',(0.0282704581919762,0.0760620724766204,
-0.548267681532694));
#52565=CARTESIAN_POINT('Ctrl Pts',(0.0481472482356463,0.0601553154154528,
-0.550119937213548));
#52566=CARTESIAN_POINT('Ctrl Pts',(0.0680240382793164,0.0442485583542852,
-0.551972192894402));
#52567=CARTESIAN_POINT('Ctrl Pts',(0.0792249689748476,0.0175218302292525,
-0.553824448575256));
#52568=CARTESIAN_POINT('Ctrl Pts',(0.0766467092357258,-0.0078140970938064,
-0.55567670425611));
#52569=CARTESIAN_POINT('Ctrl Pts',(0.0742695739254072,-0.031173623888351,
-0.557384469504073));
#52570=CARTESIAN_POINT('Ctrl Pts',(0.0601791680603887,-0.0533508732364468,
-0.559092234752036));
#52571=CARTESIAN_POINT('Ctrl Pts',(0.040207606550226,-0.0657262044767398,
-0.5608));
#52572=CARTESIAN_POINT('',(-0.076925,-9.42059550244101E-18,-0.5608));
#52573=CARTESIAN_POINT('Origin',(0.,0.,-0.5608));
#52574=CARTESIAN_POINT('',(-0.076925,-9.42059550244101E-18,-0.583875));
#52575=CARTESIAN_POINT('',(-0.076925,-9.42059550244101E-18,-0.2904));
#52576=CARTESIAN_POINT('Origin',(0.,0.,-0.583875));
#52577=CARTESIAN_POINT('',(0.076385061748025,-0.00909823976109752,-0.5608));
#52578=CARTESIAN_POINT('Origin',(0.,0.,-0.5608));
#52579=CARTESIAN_POINT('Ctrl Pts',(0.0763850617480249,-0.00909823976109754,
-0.5608));
#52580=CARTESIAN_POINT('Ctrl Pts',(0.079410373516701,0.0163010278253042,
-0.558947744319146));
#52581=CARTESIAN_POINT('Ctrl Pts',(0.0687474789230948,0.0431078601247894,
-0.557095488638293));
#52582=CARTESIAN_POINT('Ctrl Pts',(0.0491671677694739,0.0593179775882079,
-0.555243232957439));
#52583=CARTESIAN_POINT('Ctrl Pts',(0.0295868566158525,0.0755280950516269,
-0.553390977276585));
#52584=CARTESIAN_POINT('Ctrl Pts',(0.00108912890221588,0.0811414976789785,
-0.551538721595731));
#52585=CARTESIAN_POINT('Ctrl Pts',(-0.0232026118821274,0.0734899793472007,
-0.549686465914878));
#52586=CARTESIAN_POINT('Ctrl Pts',(-0.0474943526664708,0.065838461015423,
-0.547834210234024));
#52587=CARTESIAN_POINT('Ctrl Pts',(-0.0675801065215208,0.0449220217245157,
-0.54598195455317));
#52588=CARTESIAN_POINT('Ctrl Pts',(-0.0743052974197677,0.0203592775072516,
-0.544129698872317));
#52589=CARTESIAN_POINT('Ctrl Pts',(-0.0761086993520085,0.0137726242727538,
-0.543633004945795));
#52590=CARTESIAN_POINT('Ctrl Pts',(-0.076951372979264,0.006923773377672,
-0.543136311019274));
#52591=CARTESIAN_POINT('Ctrl Pts',(-0.0768915057166184,6.11931288171008E-5,
-0.542639617092752));
#52592=CARTESIAN_POINT('Origin',(0.,0.,-0.2904));
#52593=CARTESIAN_POINT('',(-0.0768038780644556,-2.07208059154612E-5,-0.502610382907248));
#52594=CARTESIAN_POINT('',(-0.0768078911416689,-2.75047320366774E-5,-0.507639617092753));
#52595=CARTESIAN_POINT('',(-0.076925,-9.42059550244101E-18,-0.2904));
#52596=CARTESIAN_POINT('Ctrl Pts',(-0.0768038780644556,-2.07208059154612E-5,
-0.502610382907248));
#52597=CARTESIAN_POINT('Ctrl Pts',(-0.0767698356268339,0.0140956948725698,
-0.503628855562518));
#52598=CARTESIAN_POINT('Ctrl Pts',(-0.0730479576749677,0.0282288086778181,
-0.504647328217789));
#52599=CARTESIAN_POINT('Ctrl Pts',(-0.0657479191161002,0.0401754805758868,
-0.50566580087306));
#52600=CARTESIAN_POINT('Ctrl Pts',(-0.0524716295454961,0.0619024172550219,
-0.507518056553913));
#52601=CARTESIAN_POINT('Ctrl Pts',(-0.0273604846150267,0.0763976428495325,
-0.509370312234767));
#52602=CARTESIAN_POINT('Ctrl Pts',(-0.00190612534401761,0.0770274929451187,
-0.511222567915621));
#52603=CARTESIAN_POINT('Ctrl Pts',(0.0235482339269917,0.0776573430407048,
-0.513074823596474));
#52604=CARTESIAN_POINT('Ctrl Pts',(0.0493458075385404,0.0644218176373664,
-0.514927079277328));
#52605=CARTESIAN_POINT('Ctrl Pts',(0.0636804316029636,0.0433782047807641,
-0.516779334958182));
#52606=CARTESIAN_POINT('Ctrl Pts',(0.0780150556673868,0.0223345919241618,
-0.518631590639035));
#52607=CARTESIAN_POINT('Ctrl Pts',(0.080886730184684,-0.00651710838570469,
-0.520483846319889));
#52608=CARTESIAN_POINT('Ctrl Pts',(0.0709817539352405,-0.0299737413516422,
-0.522336102000743));
#52609=CARTESIAN_POINT('Ctrl Pts',(0.0610767776857971,-0.0534303743175797,
-0.524188357681596));
#52610=CARTESIAN_POINT('Ctrl Pts',(0.0383951506696132,-0.0714919399395886,
-0.52604061336245));
#52611=CARTESIAN_POINT('Ctrl Pts',(0.0133158987600065,-0.0758919834556476,
-0.527892869043304));
#52612=CARTESIAN_POINT('Ctrl Pts',(-0.0117633531496002,-0.0802920269717066,
-0.529745124724158));
#52613=CARTESIAN_POINT('Ctrl Pts',(-0.0392402299526296,-0.0710305483818158,
-0.531597380405011));
#52614=CARTESIAN_POINT('Ctrl Pts',(-0.0565385801046214,-0.0523475002550685,
-0.533449636085865));
#52615=CARTESIAN_POINT('Ctrl Pts',(-0.069491085555866,-0.038358172915681,
-0.534836551692993));
#52616=CARTESIAN_POINT('Ctrl Pts',(-0.0767369162943482,-0.0190865650976122,
-0.53622346730012));
#52617=CARTESIAN_POINT('Ctrl Pts',(-0.0769096047044028,6.91658437555233E-5,
-0.537610382907248));
#52618=CARTESIAN_POINT('Ctrl Pts',(-0.0768915057166184,6.11931288171008E-5,
-0.542639617092752));
#52619=CARTESIAN_POINT('Ctrl Pts',(-0.0767281178287347,-0.0186679493564494,
-0.54128405533842));
#52620=CARTESIAN_POINT('Ctrl Pts',(-0.0698422765132579,-0.037499353071499,
-0.539928493584088));
#52621=CARTESIAN_POINT('Ctrl Pts',(-0.0574168066131572,-0.0513821924115064,
-0.538572931829756));
#52622=CARTESIAN_POINT('Ctrl Pts',(-0.0404384969668562,-0.0703518689693793,
-0.536720676148902));
#52623=CARTESIAN_POINT('Ctrl Pts',(-0.0131172497328104,-0.0800821729415043,
-0.534868420468049));
#52624=CARTESIAN_POINT('Ctrl Pts',(0.0120338256236662,-0.0761076871249378,
-0.533016164787195));
#52625=CARTESIAN_POINT('Ctrl Pts',(0.0371849009801429,-0.0721332013083712,
-0.531163909106341));
#52626=CARTESIAN_POINT('Ctrl Pts',(0.0601658044590504,-0.0544539257031128,
-0.529311653425487));
#52627=CARTESIAN_POINT('Ctrl Pts',(0.0704648543013367,-0.0311671118066004,
-0.527459397744633));
#52628=CARTESIAN_POINT('Ctrl Pts',(0.080763904143623,-0.00788029791008813,
-0.525607142063779));
#52629=CARTESIAN_POINT('Ctrl Pts',(0.0783811003492882,0.0210140542776783,
-0.523754886382926));
#52630=CARTESIAN_POINT('Ctrl Pts',(0.0644041500243277,0.042296301050223,
-0.521902630702073));
#52631=CARTESIAN_POINT('Ctrl Pts',(0.0504271996993672,0.0635785478227678,
-0.520050375021219));
#52632=CARTESIAN_POINT('Ctrl Pts',(0.024856102843781,0.077248689180091,
-0.518198119340365));
#52633=CARTESIAN_POINT('Ctrl Pts',(-0.000605423883035404,0.0770489427047095,
-0.516345863659511));
#52634=CARTESIAN_POINT('Ctrl Pts',(-0.0260669506098518,0.0768491962293279,
-0.514493607978657));
#52635=CARTESIAN_POINT('Ctrl Pts',(-0.0514189072078984,0.0627795619212417,
-0.512641352297804));
#52636=CARTESIAN_POINT('Ctrl Pts',(-0.0650600797594811,0.0412797811922074,
-0.51078909661695));
#52637=CARTESIAN_POINT('Ctrl Pts',(-0.0727916606064359,0.0290940770476583,
-0.509739270108885));
#52638=CARTESIAN_POINT('Ctrl Pts',(-0.0767612381677875,0.0145214929865115,
-0.508689443600819));
#52639=CARTESIAN_POINT('Ctrl Pts',(-0.0768078911416689,-2.75047320366774E-5,
-0.507639617092753));
#52640=CARTESIAN_POINT('Origin',(0.,0.,-0.2904));
#52641=CARTESIAN_POINT('',(-0.0769866657903101,-5.93158920058345E-5,-0.467610382907248));
#52642=CARTESIAN_POINT('',(-0.0769983882791968,-5.48405244063995E-5,-0.472639617092753));
#52643=CARTESIAN_POINT('',(-0.076925,-9.42059550244101E-18,-0.2904));
#52644=CARTESIAN_POINT('Ctrl Pts',(-0.0769866657903101,-5.93158920058345E-5,
-0.467610382907248));
#52645=CARTESIAN_POINT('Ctrl Pts',(-0.0768022090703362,0.0215924718018981,
-0.469181988144063));
#52646=CARTESIAN_POINT('Ctrl Pts',(-0.0672397070232822,0.0433868987541688,
-0.470753593380878));
#52647=CARTESIAN_POINT('Ctrl Pts',(-0.0510603483059523,0.0577035795188773,
-0.472325198617693));
#52648=CARTESIAN_POINT('Ctrl Pts',(-0.0319917499106721,0.0745768710148652,
-0.474177454298547));
#52649=CARTESIAN_POINT('Ctrl Pts',(-0.00373206903032697,0.0810632695438336,
-0.4760297099794));
#52650=CARTESIAN_POINT('Ctrl Pts',(0.0207860373958043,0.0741943601536088,
-0.477881965660254));
#52651=CARTESIAN_POINT('Ctrl Pts',(0.0453041438219356,0.067325450763384,
-0.479734221341108));
#52652=CARTESIAN_POINT('Ctrl Pts',(0.066080675793853,0.0471012334539661,
-0.481586477021962));
#52653=CARTESIAN_POINT('Ctrl Pts',(0.0736075296600365,0.0227770520257243,
-0.483438732702815));
#52654=CARTESIAN_POINT('Ctrl Pts',(0.08113438352622,-0.00154712940251749,
-0.485290988383669));
#52655=CARTESIAN_POINT('Ctrl Pts',(0.0754115592866696,-0.0299712749495833,
-0.487143244064522));
#52656=CARTESIAN_POINT('Ctrl Pts',(0.0590580402410755,-0.0494874691264555,
-0.488995499745376));
#52657=CARTESIAN_POINT('Ctrl Pts',(0.0427045211954813,-0.069003663303328,
-0.49084775542623));
#52658=CARTESIAN_POINT('Ctrl Pts',(0.0157203073438432,-0.0796119061100067,
-0.492700011107084));
#52659=CARTESIAN_POINT('Ctrl Pts',(-0.00954566134870712,-0.0764574612990264,
-0.494552266787938));
#52660=CARTESIAN_POINT('Ctrl Pts',(-0.0348116300412571,-0.0733030164880461,
-0.496404522468791));
#52661=CARTESIAN_POINT('Ctrl Pts',(-0.0583593535747193,-0.0563858840594071,
-0.498256778149645));
#52662=CARTESIAN_POINT('Ctrl Pts',(-0.0694124982360811,-0.0334479939632078,
-0.500109033830498));
#52663=CARTESIAN_POINT('Ctrl Pts',(-0.0743880124122404,-0.0231226249536286,
-0.500942816856081));
#52664=CARTESIAN_POINT('Ctrl Pts',(-0.0768317472531782,-0.0115772684597858,
-0.501776599881665));
#52665=CARTESIAN_POINT('Ctrl Pts',(-0.0768038780644556,-2.07208059154612E-5,
-0.502610382907248));
#52666=CARTESIAN_POINT('Ctrl Pts',(-0.0768078911416689,-2.75047320366774E-5,
-0.507639617092753));
#52667=CARTESIAN_POINT('Ctrl Pts',(-0.0768435500881255,-0.0111479518863914,
-0.506837187919965));
#52668=CARTESIAN_POINT('Ctrl Pts',(-0.0745873478507643,-0.0222546193664585,
-0.506034758747177));
#52669=CARTESIAN_POINT('Ctrl Pts',(-0.0699674254473345,-0.0322711198318006,
-0.505232329574389));
#52670=CARTESIAN_POINT('Ctrl Pts',(-0.0593032100784864,-0.0553923129767922,
-0.503380073893535));
#52671=CARTESIAN_POINT('Ctrl Pts',(-0.0360443908356715,-0.0727047721167927,
-0.501527818212681));
#52672=CARTESIAN_POINT('Ctrl Pts',(-0.0108352639658483,-0.0762854167965552,
-0.499675562531828));
#52673=CARTESIAN_POINT('Ctrl Pts',(0.0143738629039748,-0.0798660614763177,
-0.497823306850974));
#52674=CARTESIAN_POINT('Ctrl Pts',(0.0415332974008062,-0.0697148916958422,
-0.495971051170121));
#52675=CARTESIAN_POINT('Ctrl Pts',(0.0582140048717536,-0.0504775941790726,
-0.494118795489267));
#52676=CARTESIAN_POINT('Ctrl Pts',(0.0748947123427012,-0.0312402966623029,
-0.492266539808413));
#52677=CARTESIAN_POINT('Ctrl Pts',(0.0810966927877647,-0.00291687140923884,
-0.490414284127559));
#52678=CARTESIAN_POINT('Ctrl Pts',(0.0739816346844856,0.0215309246469676,
-0.488562028446706));
#52679=CARTESIAN_POINT('Ctrl Pts',(0.0668665765812064,0.045978720703174,
-0.486709772765852));
#52680=CARTESIAN_POINT('Ctrl Pts',(0.0464344799295845,0.0665508875625229,
-0.484857517084999));
#52681=CARTESIAN_POINT('Ctrl Pts',(0.0220358480118087,0.0738328125955258,
-0.483005261404145));
#52682=CARTESIAN_POINT('Ctrl Pts',(-0.00236278390596698,0.0811147376285286,
-0.481153005723291));
#52683=CARTESIAN_POINT('Ctrl Pts',(-0.0307279510898964,0.0751064208351859,
-0.479300750042437));
#52684=CARTESIAN_POINT('Ctrl Pts',(-0.0500787358259481,0.058557507707521,
-0.477448494361583));
#52685=CARTESIAN_POINT('Ctrl Pts',(-0.0668250827824603,0.0442359261918763,
-0.475845535271973));
#52686=CARTESIAN_POINT('Ctrl Pts',(-0.0768202606431028,0.0220201435331388,
-0.474242576182363));
#52687=CARTESIAN_POINT('Ctrl Pts',(-0.0769983882791968,-5.48405244063995E-5,
-0.472639617092753));
#52688=CARTESIAN_POINT('Origin',(0.,0.,-0.2904));
#52689=CARTESIAN_POINT('',(-0.0769897824783354,5.82191621161781E-5,-0.432610382907248));
#52690=CARTESIAN_POINT('',(-0.0769776111042551,6.21574435400559E-5,-0.437639617092753));
#52691=CARTESIAN_POINT('',(-0.076925,-9.42059550244101E-18,-0.2904));
#52692=CARTESIAN_POINT('Ctrl Pts',(-0.0769897824783354,5.82191621161781E-5,
-0.432610382907248));
#52693=CARTESIAN_POINT('Ctrl Pts',(-0.0770213613227461,0.00381177252221594,
-0.432882865044754));
#52694=CARTESIAN_POINT('Ctrl Pts',(-0.0767705832646258,0.00756108964264168,
-0.433155347182259));
#52695=CARTESIAN_POINT('Ctrl Pts',(-0.0762228831071107,0.0112665186516345,
-0.433427829319765));
#52696=CARTESIAN_POINT('Ctrl Pts',(-0.0724997739982054,0.0364549658457594,
-0.435280085000619));
#52697=CARTESIAN_POINT('Ctrl Pts',(-0.0550562160586267,0.0596153909141568,
-0.437132340681473));
#52698=CARTESIAN_POINT('Ctrl Pts',(-0.0318750171218392,0.070148739350433,
-0.438984596362327));
#52699=CARTESIAN_POINT('Ctrl Pts',(-0.00869381818505173,0.0806820877867091,
-0.44083685204318));
#52700=CARTESIAN_POINT('Ctrl Pts',(0.0202250217489445,0.078588359590864,
-0.442689107724034));
#52701=CARTESIAN_POINT('Ctrl Pts',(0.041647187712571,0.0648257210299977,
-0.444541363404887));
#52702=CARTESIAN_POINT('Ctrl Pts',(0.0630693536761977,0.0510630824691312,
-0.446393619085741));
#52703=CARTESIAN_POINT('Ctrl Pts',(0.0769948456694544,0.0256315335432433,
-0.448245874766595));
#52704=CARTESIAN_POINT('Ctrl Pts',(0.0770508509581164,0.000169477937355909,
-0.450098130447449));
#52705=CARTESIAN_POINT('Ctrl Pts',(0.0771068562467784,-0.0252925776685313,
-0.451950386128303));
#52706=CARTESIAN_POINT('Ctrl Pts',(0.0632933748308458,-0.0507851399544181,
-0.453802641809156));
#52707=CARTESIAN_POINT('Ctrl Pts',(0.0419319594279733,-0.0646418836062034,
-0.45565489749001));
#52708=CARTESIAN_POINT('Ctrl Pts',(0.0205705440251007,-0.0784986272579888,
-0.457507153170863));
#52709=CARTESIAN_POINT('Ctrl Pts',(-0.00833880536471181,-0.0807195522756726,
-0.459359408851717));
#52710=CARTESIAN_POINT('Ctrl Pts',(-0.0315661173541412,-0.0702882820528092,
-0.461211664532571));
#52711=CARTESIAN_POINT('Ctrl Pts',(-0.0547934293435706,-0.0598570118299457,
-0.463063920213425));
#52712=CARTESIAN_POINT('Ctrl Pts',(-0.0723387039326168,-0.0367735463665349,
-0.464916175894278));
#52713=CARTESIAN_POINT('Ctrl Pts',(-0.0761725832720322,-0.011601721403326,
-0.466768431575132));
#52714=CARTESIAN_POINT('Ctrl Pts',(-0.0767534857630434,-0.00778773183038919,
-0.467049082019171));
#52715=CARTESIAN_POINT('Ctrl Pts',(-0.0770196052710104,-0.00392579819187431,
-0.467329732463209));
#52716=CARTESIAN_POINT('Ctrl Pts',(-0.0769866657903101,-5.93158920058345E-5,
-0.467610382907248));
#52717=CARTESIAN_POINT('Ctrl Pts',(-0.0769983882791968,-5.48405244063995E-5,
-0.472639617092753));
#52718=CARTESIAN_POINT('Ctrl Pts',(-0.0770260911774007,-0.00348800255141457,
-0.47239032050151));
#52719=CARTESIAN_POINT('Ctrl Pts',(-0.0768163459113883,-0.00691775903718454,
-0.472141023910266));
#52720=CARTESIAN_POINT('Ctrl Pts',(-0.0763576196212321,-0.0103138848938282,
-0.471891727319023));
#52721=CARTESIAN_POINT('Ctrl Pts',(-0.0729493163922906,-0.0355468549055254,
-0.470039471638169));
#52722=CARTESIAN_POINT('Ctrl Pts',(-0.0557963076462339,-0.0589232854669328,
-0.468187215957315));
#52723=CARTESIAN_POINT('Ctrl Pts',(-0.0327484398723308,-0.0697452642775618,
-0.466334960276461));
#52724=CARTESIAN_POINT('Ctrl Pts',(-0.00970057209842773,-0.0805672430881908,
-0.464482704595607));
#52725=CARTESIAN_POINT('Ctrl Pts',(0.0192421547033216,-0.0788347701480414,
-0.462630448914754));
#52726=CARTESIAN_POINT('Ctrl Pts',(0.0408344964221166,-0.0653406912587224,
-0.460778193233901));
#52727=CARTESIAN_POINT('Ctrl Pts',(0.0624268381409117,-0.0518466123694032,
-0.458925937553047));
#52728=CARTESIAN_POINT('Ctrl Pts',(0.0766687947767522,-0.0265909275309141,
-0.457073681872193));
#52729=CARTESIAN_POINT('Ctrl Pts',(0.077042726683417,-0.00113155689853747,
-0.455221426191339));
#52730=CARTESIAN_POINT('Ctrl Pts',(0.0774166585900817,0.0243278137338391,
-0.453369170510485));
#52731=CARTESIAN_POINT('Ctrl Pts',(0.0639225657675707,0.0499908701601033,
-0.451516914829632));
#52732=CARTESIAN_POINT('Ctrl Pts',(0.0427358375238719,0.0641132616844177,
-0.449664659148778));
#52733=CARTESIAN_POINT('Ctrl Pts',(0.0215491092801732,0.0782356532087321,
-0.447812403467925));
#52734=CARTESIAN_POINT('Ctrl Pts',(-0.00733025438471345,0.0808173798310969,
-0.445960147787071));
#52735=CARTESIAN_POINT('Ctrl Pts',(-0.0306860045756403,0.0706769498119031,
-0.444107892106217));
#52736=CARTESIAN_POINT('Ctrl Pts',(-0.0540417547665674,0.0605365197927092,
-0.442255636425363));
#52737=CARTESIAN_POINT('Ctrl Pts',(-0.0718738914835347,0.0376739331319566,
-0.44040338074451));
#52738=CARTESIAN_POINT('Ctrl Pts',(-0.0760217789291502,0.0125519424202647,
-0.438551125063656));
#52739=CARTESIAN_POINT('Ctrl Pts',(-0.0767021804000287,0.00843103999565815,
-0.438247289073355));
#52740=CARTESIAN_POINT('Ctrl Pts',(-0.0770143702100962,0.00424934220686737,
-0.437943453083054));
#52741=CARTESIAN_POINT('Ctrl Pts',(-0.0769776111042551,6.21574435400559E-5,
-0.437639617092753));
#52742=CARTESIAN_POINT('Origin',(0.,0.,-0.2904));
#52743=CARTESIAN_POINT('',(-0.0768048397279485,2.24810141056936E-5,-0.397610382907248));
#52744=CARTESIAN_POINT('',(-0.0768016249961445,1.56088566556244E-5,-0.402639617092753));
#52745=CARTESIAN_POINT('',(-0.076925,-9.42059550244101E-18,-0.2904));
#52746=CARTESIAN_POINT('Ctrl Pts',(-0.0768048397279485,2.24810141056936E-5,
-0.397610382907248));
#52747=CARTESIAN_POINT('Ctrl Pts',(-0.0768348080986574,0.0114654674856241,
-0.398435997626298));
#52748=CARTESIAN_POINT('Ctrl Pts',(-0.0744407065702995,0.0228965349070991,
-0.399261612345349));
#52749=CARTESIAN_POINT('Ctrl Pts',(-0.0695589566944398,0.0331423278363428,
-0.400087227064399));
#52750=CARTESIAN_POINT('Ctrl Pts',(-0.0586068155426079,0.056128628492264,
-0.401939482745252));
#52751=CARTESIAN_POINT('Ctrl Pts',(-0.0351337611659022,0.0731491667124345,
-0.403791738426106));
#52752=CARTESIAN_POINT('Ctrl Pts',(-0.00988191866549493,0.0764147239363237,
-0.40564399410696));
#52753=CARTESIAN_POINT('Ctrl Pts',(0.0153699238349123,0.0796802811602129,
-0.407496249787814));
#52754=CARTESIAN_POINT('Ctrl Pts',(0.0424005544590212,0.0691908573878207,
-0.409348505468667));
#52755=CARTESIAN_POINT('Ctrl Pts',(0.0588397715697832,0.0497467951974147,
-0.411200761149521));
#52756=CARTESIAN_POINT('Ctrl Pts',(0.0752789886805451,0.0303027330070088,
-0.413053016830375));
#52757=CARTESIAN_POINT('Ctrl Pts',(0.0811267922779602,0.00190403239858913,
-0.414905272511229));
#52758=CARTESIAN_POINT('Ctrl Pts',(0.0737070143245067,-0.0224530263064039,
-0.416757528192082));
#52759=CARTESIAN_POINT('Ctrl Pts',(0.0662872363710531,-0.0468100850113971,
-0.418609783872936));
#52760=CARTESIAN_POINT('Ctrl Pts',(0.0455998768667307,-0.0671255018129637,
-0.420462039553789));
#52761=CARTESIAN_POINT('Ctrl Pts',(0.0211122254254216,-0.0741022016416912,
-0.422314295234643));
#52762=CARTESIAN_POINT('Ctrl Pts',(-0.00337542601588727,-0.0810789014704186,
-0.424166550915497));
#52763=CARTESIAN_POINT('Ctrl Pts',(-0.0316633693941828,-0.0747168843263072,
-0.426018806596351));
#52764=CARTESIAN_POINT('Ctrl Pts',(-0.0508060109442149,-0.0579276410943254,
-0.427871062277204));
#52765=CARTESIAN_POINT('Ctrl Pts',(-0.0671326115227027,-0.0436082344676476,
-0.429450835820552));
#52766=CARTESIAN_POINT('Ctrl Pts',(-0.0768066973653582,-0.0217038102542308,
-0.4310306093639));
#52767=CARTESIAN_POINT('Ctrl Pts',(-0.0769897824783354,5.82191621161781E-5,
-0.432610382907248));
#52768=CARTESIAN_POINT('Ctrl Pts',(-0.0769776111042551,6.21574435400559E-5,
-0.437639617092753));
#52769=CARTESIAN_POINT('Ctrl Pts',(-0.076790278052515,-0.021276721236018,
-0.4360911974022));
#52770=CARTESIAN_POINT('Ctrl Pts',(-0.0675401784708066,-0.0427581054999571,
-0.434542777711647));
#52771=CARTESIAN_POINT('Ctrl Pts',(-0.0517768802514736,-0.0570615176522107,
-0.432994358021095));
#52772=CARTESIAN_POINT('Ctrl Pts',(-0.0329204559539179,-0.074171592250363,
-0.431142102340241));
#52773=CARTESIAN_POINT('Ctrl Pts',(-0.00474396918454293,-0.0810103466840368,
-0.429289846659387));
#52774=CARTESIAN_POINT('Ctrl Pts',(0.0198579929404242,-0.0744481177684896,
-0.427437590978534));
#52775=CARTESIAN_POINT('Ctrl Pts',(0.0444599550653912,-0.0678858888529424,
-0.42558533529768));
#52776=CARTESIAN_POINT('Ctrl Pts',(0.0654873925459503,-0.0479226765881743,
-0.423733079616826));
#52777=CARTESIAN_POINT('Ctrl Pts',(0.0733173836702959,-0.0236943743820276,
-0.421880823935973));
#52778=CARTESIAN_POINT('Ctrl Pts',(0.0811473747946415,0.000533927824119099,
-0.420028568255119));
#52779=CARTESIAN_POINT('Ctrl Pts',(0.0757799195627735,0.0290273199716446,
-0.418176312574265));
#52780=CARTESIAN_POINT('Ctrl Pts',(0.0596713611069964,0.0487461874240278,
-0.416324056893412));
#52781=CARTESIAN_POINT('Ctrl Pts',(0.0435628026512191,0.0684650548764111,
-0.414471801212558));
#52782=CARTESIAN_POINT('Ctrl Pts',(0.0167131409715328,0.0794093976336524,
-0.412619545531704));
#52783=CARTESIAN_POINT('Ctrl Pts',(-0.00859024028526444,0.0765706856200469,
-0.41076728985085));
#52784=CARTESIAN_POINT('Ctrl Pts',(-0.0338936215420614,0.0737319736064415,
-0.408915034169997));
#52785=CARTESIAN_POINT('Ctrl Pts',(-0.0576507223759692,0.0571102068219895,
-0.407062778489143));
#52786=CARTESIAN_POINT('Ctrl Pts',(-0.0689894276722951,0.0343121114815454,
-0.405210522808289));
#52787=CARTESIAN_POINT('Ctrl Pts',(-0.0742354172971678,0.0237642959684653,
-0.404353554236444));
#52788=CARTESIAN_POINT('Ctrl Pts',(-0.0768231717031437,0.0118943987064725,
-0.403496585664598));
#52789=CARTESIAN_POINT('Ctrl Pts',(-0.0768016249961445,1.56088566556244E-5,
-0.402639617092753));
#52790=CARTESIAN_POINT('Origin',(0.,0.,-0.2904));
#52791=CARTESIAN_POINT('',(-0.0769074003423832,-7.00577226088184E-5,-0.362610382907248));
#52792=CARTESIAN_POINT('',(-0.0769203613463617,-7.03313400393759E-5,-0.367639617092753));
#52793=CARTESIAN_POINT('',(-0.076925,-9.42059550244101E-18,-0.2904));
#52794=CARTESIAN_POINT('Ctrl Pts',(-0.0769074003423832,-7.00577226088184E-5,
-0.362610382907248));
#52795=CARTESIAN_POINT('Ctrl Pts',(-0.0767365258441259,0.0189751470910833,
-0.363989130207843));
#52796=CARTESIAN_POINT('Ctrl Pts',(-0.0695830537667149,0.038134992706218,
-0.365367877508438));
#52797=CARTESIAN_POINT('Ctrl Pts',(-0.0567678074694182,0.0520987368937514,
-0.366746624809032));
#52798=CARTESIAN_POINT('Ctrl Pts',(-0.0395513728512194,0.0708581023599177,
-0.368598880489886));
#52799=CARTESIAN_POINT('Ctrl Pts',(-0.012116487223219,0.0802394697255212,
-0.370451136170739));
#52800=CARTESIAN_POINT('Ctrl Pts',(0.0129816459543213,0.0759495834032349,
-0.372303391851593));
#52801=CARTESIAN_POINT('Ctrl Pts',(0.0380797791318617,0.0716596970809485,
-0.374155647532447));
#52802=CARTESIAN_POINT('Ctrl Pts',(0.0608411598589422,0.0536985570707719,
-0.376007903213301));
#52803=CARTESIAN_POINT('Ctrl Pts',(0.0708493508323878,0.0302858355908709,
-0.377860158894154));
#52804=CARTESIAN_POINT('Ctrl Pts',(0.0808575418058333,0.00687311411097037,
-0.379712414575008));
#52805=CARTESIAN_POINT('Ctrl Pts',(0.0781125430256448,-0.0219911888386541,
-0.381564670255862));
#52806=CARTESIAN_POINT('Ctrl Pts',(0.0638705659683053,-0.0430977163397371,
-0.383416925936715));
#52807=CARTESIAN_POINT('Ctrl Pts',(0.0496285889109656,-0.0642042438408205,
-0.385269181617569));
#52808=CARTESIAN_POINT('Ctrl Pts',(0.0238896335764741,-0.0775529958933619,
-0.387121437298423));
#52809=CARTESIAN_POINT('Ctrl Pts',(-0.00156721608113352,-0.0770350970958021,
-0.388973692979277));
#52810=CARTESIAN_POINT('Ctrl Pts',(-0.0270240657387409,-0.0765171982982424,
-0.39082594866013));
#52811=CARTESIAN_POINT('Ctrl Pts',(-0.0521988097194646,-0.0621326486505818,
-0.392678204340984));
#52812=CARTESIAN_POINT('Ctrl Pts',(-0.0655705677463472,-0.0404643422809157,
-0.394530460021838));
#52813=CARTESIAN_POINT('Ctrl Pts',(-0.0729820685794259,-0.0284543529895058,
-0.395557100983641));
#52814=CARTESIAN_POINT('Ctrl Pts',(-0.0767675744561234,-0.0142067210167618,
-0.396583741945445));
#52815=CARTESIAN_POINT('Ctrl Pts',(-0.0768048397279485,2.24810141056936E-5,
-0.397610382907248));
#52816=CARTESIAN_POINT('Ctrl Pts',(-0.0768016249961445,1.56088566556244E-5,
-0.402639617092753));
#52817=CARTESIAN_POINT('Ctrl Pts',(-0.0767766005548495,-0.0137804704822612,
-0.401644329983744));
#52818=CARTESIAN_POINT('Ctrl Pts',(-0.0732319934678846,-0.0275885446797342,
-0.400649042874736));
#52819=CARTESIAN_POINT('Ctrl Pts',(-0.0662444625517081,-0.0393514079285166,
-0.399653755765728));
#52820=CARTESIAN_POINT('Ctrl Pts',(-0.0532404823760513,-0.0612424081016978,
-0.397801500084874));
#52821=CARTESIAN_POINT('Ctrl Pts',(-0.0283122122659939,-0.0760499845516238,
-0.395949244404021));
#52822=CARTESIAN_POINT('Ctrl Pts',(-0.00286773707221562,-0.0769976506705498,
-0.394096988723167));
#52823=CARTESIAN_POINT('Ctrl Pts',(0.0225767381215624,-0.0779453167894759,
-0.392244733042314));
#52824=CARTESIAN_POINT('Ctrl Pts',(0.0485374183990613,-0.0650330725774021,
-0.39039247736146));
#52825=CARTESIAN_POINT('Ctrl Pts',(0.0631337503916168,-0.0441700315399829,
-0.388540221680606));
#52826=CARTESIAN_POINT('Ctrl Pts',(0.0777300823841723,-0.0233069905025635,
-0.386687965999752));
#52827=CARTESIAN_POINT('Ctrl Pts',(0.0809620660917846,0.00550684736020137,
-0.384835710318898));
#52828=CARTESIAN_POINT('Ctrl Pts',(0.0713506279884725,0.0290852197925241,
-0.382983454638045));
#52829=CARTESIAN_POINT('Ctrl Pts',(0.0617391898851602,0.0526635922248472,
-0.381131198957191));
#52830=CARTESIAN_POINT('Ctrl Pts',(0.0392843299709232,0.0710064992267279,
-0.379278943276338));
#52831=CARTESIAN_POINT('Ctrl Pts',(0.0142622104544463,0.0757195580922204,
-0.377426687595484));
#52832=CARTESIAN_POINT('Ctrl Pts',(-0.0107599090620303,0.0804326169577127,
-0.37557443191463));
#52833=CARTESIAN_POINT('Ctrl Pts',(-0.0383492881807465,0.0715158276868172,
-0.373722176233776));
#52834=CARTESIAN_POINT('Ctrl Pts',(-0.055880021589883,0.0530498380002214,
-0.371869920552923));
#52835=CARTESIAN_POINT('Ctrl Pts',(-0.0692259692662876,0.0389918903719781,
-0.370459819399532));
#52836=CARTESIAN_POINT('Ctrl Pts',(-0.0767423247315113,0.0193996048245303,
-0.369049718246142));
#52837=CARTESIAN_POINT('Ctrl Pts',(-0.0769203613463617,-7.03313400393759E-5,
-0.367639617092753));
#52838=CARTESIAN_POINT('Origin',(0.,0.,-0.2904));
#52839=CARTESIAN_POINT('',(-0.0770446167695562,2.01096196933834E-5,-0.327610382907248));
#52840=CARTESIAN_POINT('',(-0.0770389450880675,2.75992272470979E-5,-0.332639617092753));
#52841=CARTESIAN_POINT('',(-0.076925,-9.42059550244101E-18,-0.2904));
#52842=CARTESIAN_POINT('Ctrl Pts',(-0.0770446167695562,2.01096196933833E-5,
-0.327610382907248));
#52843=CARTESIAN_POINT('Ctrl Pts',(-0.0770484429332084,0.00111491216618904,
-0.327690007108533));
#52844=CARTESIAN_POINT('Ctrl Pts',(-0.0770271266597134,0.00220956238892732,
-0.327769631309819));
#52845=CARTESIAN_POINT('Ctrl Pts',(-0.0769802038809804,0.00330311387201044,
-0.327849255511104));
#52846=CARTESIAN_POINT('Ctrl Pts',(-0.0758886640970139,0.0287418236379544,
-0.329701511191958));
#52847=CARTESIAN_POINT('Ctrl Pts',(-0.0609403544790954,0.0535859586125592,
-0.331553766872812));
#52848=CARTESIAN_POINT('Ctrl Pts',(-0.0389761662627314,0.0664659372481025,
-0.333406022553666));
#52849=CARTESIAN_POINT('Ctrl Pts',(-0.0170119780463675,0.0793459158836458,
-0.335258278234519));
#52850=CARTESIAN_POINT('Ctrl Pts',(0.0119680887684414,0.0802617381801278,
-0.337110533915373));
#52851=CARTESIAN_POINT('Ctrl Pts',(0.0347016995000411,0.0687942904797893,
-0.338962789596227));
#52852=CARTESIAN_POINT('Ctrl Pts',(0.0574353102316408,0.0573268427794508,
-0.34081504527708));
#52853=CARTESIAN_POINT('Ctrl Pts',(0.073922464880031,0.0334761250822914,
-0.342667300957934));
#52854=CARTESIAN_POINT('Ctrl Pts',(0.0766180406443424,0.00815709498722714,
-0.344519556638788));
#52855=CARTESIAN_POINT('Ctrl Pts',(0.0793136164086537,-0.0171619351078373,
-0.346371812319641));
#52856=CARTESIAN_POINT('Ctrl Pts',(0.0682176132888862,-0.0439492776008071,
-0.348224068000495));
#52857=CARTESIAN_POINT('Ctrl Pts',(0.0484079666791642,-0.0599460683681405,
-0.350076323681349));
#52858=CARTESIAN_POINT('Ctrl Pts',(0.0285983200694422,-0.0759428591354739,
-0.351928579362203));
#52859=CARTESIAN_POINT('Ctrl Pts',(7.50299697655082E-5,-0.081149098177171,
-0.353780835043056));
#52860=CARTESIAN_POINT('Ctrl Pts',(-0.0241086066091563,-0.0731822207791869,
-0.35563309072391));
#52861=CARTESIAN_POINT('Ctrl Pts',(-0.048292243188078,-0.0652153433812029,
-0.357485346404764));
#52862=CARTESIAN_POINT('Ctrl Pts',(-0.068136226246245,-0.044075349543538,
-0.359337602085617));
#52863=CARTESIAN_POINT('Ctrl Pts',(-0.0745592259711298,-0.0194366708413409,
-0.361189857766471));
#52864=CARTESIAN_POINT('Ctrl Pts',(-0.0762011937769633,-0.0131380691069294,
-0.36166336614673));
#52865=CARTESIAN_POINT('Ctrl Pts',(-0.0769660844151371,-0.00661082416990631,
-0.362136874526989));
#52866=CARTESIAN_POINT('Ctrl Pts',(-0.0769074003423832,-7.00577226088184E-5,
-0.362610382907248));
#52867=CARTESIAN_POINT('Ctrl Pts',(-0.0769203613463617,-7.03313400393759E-5,
-0.367639617092753));
#52868=CARTESIAN_POINT('Ctrl Pts',(-0.0769761869125781,-0.00617536884312658,
-0.367197462565289));
#52869=CARTESIAN_POINT('Ctrl Pts',(-0.0763104994214254,-0.0122683767956985,
-0.366755308037825));
#52870=CARTESIAN_POINT('Ctrl Pts',(-0.0748767850554384,-0.0181749603711571,
-0.366313153510362));
#52871=CARTESIAN_POINT('Ctrl Pts',(-0.068870727412301,-0.0429185789536437,
-0.364460897829508));
#52872=CARTESIAN_POINT('Ctrl Pts',(-0.0493865244264695,-0.0643906260163209,
-0.362608642148654));
#52873=CARTESIAN_POINT('Ctrl Pts',(-0.0253408574380519,-0.0727647103274385,
-0.360756386467801));
#52874=CARTESIAN_POINT('Ctrl Pts',(-0.00129519044963403,-0.0811387946385562,
-0.358904130786947));
#52875=CARTESIAN_POINT('Ctrl Pts',(0.0273119405413703,-0.0764149161981138,
-0.357051875106093));
#52876=CARTESIAN_POINT('Ctrl Pts',(0.0473888698769944,-0.0607548939305632,
-0.35519961942524));
#52877=CARTESIAN_POINT('Ctrl Pts',(0.0674657992126183,-0.0450948716630129,
-0.353347363744386));
#52878=CARTESIAN_POINT('Ctrl Pts',(0.0790125268928624,-0.0184987055683546,
-0.351495108063532));
#52879=CARTESIAN_POINT('Ctrl Pts',(0.0767448495391868,0.00686222951668314,
-0.349642852382678));
#52880=CARTESIAN_POINT('Ctrl Pts',(0.0744771721855112,0.032223164601721,
-0.347790596701825));
#52881=CARTESIAN_POINT('Ctrl Pts',(0.058395089797916,0.0563488686771379,
-0.345938341020971));
#52882=CARTESIAN_POINT('Ctrl Pts',(0.035858349348866,0.068198540356131,
-0.344086085340117));
#52883=CARTESIAN_POINT('Ctrl Pts',(0.0133216088998161,0.080048212035124,
-0.342233829659264));
#52884=CARTESIAN_POINT('Ctrl Pts',(-0.0156697896106886,0.0796218513176928,
-0.34038157397841));
#52885=CARTESIAN_POINT('Ctrl Pts',(-0.0378483257040854,0.0671145764057984,
-0.338529318297556));
#52886=CARTESIAN_POINT('Ctrl Pts',(-0.0600268617974825,0.0546073014939038,
-0.336677062616703));
#52887=CARTESIAN_POINT('Ctrl Pts',(-0.0753925354737718,0.0300191123875455,
-0.334824806935849));
#52888=CARTESIAN_POINT('Ctrl Pts',(-0.0769134544945309,0.00460246047782053,
-0.332972551254995));
#52889=CARTESIAN_POINT('Ctrl Pts',(-0.0770045804849021,0.00307961965225423,
-0.332861573200914));
#52890=CARTESIAN_POINT('Ctrl Pts',(-0.0770460063361865,0.00155380479662527,
-0.332750595146834));
#52891=CARTESIAN_POINT('Ctrl Pts',(-0.0770389450880675,2.75992272470979E-5,
-0.332639617092753));
#52892=CARTESIAN_POINT('Origin',(0.,0.,-0.2904));
#52893=CARTESIAN_POINT('',(-0.0768483116041091,5.73613550720782E-5,-0.292610382907248));
#52894=CARTESIAN_POINT('',(-0.0768387410148688,5.28831155507099E-5,-0.297639617092753));
#52895=CARTESIAN_POINT('',(-0.076925,-9.42059550244101E-18,-0.2904));
#52896=CARTESIAN_POINT('Ctrl Pts',(-0.0768483116041091,5.73613550720782E-5,
-0.292610382907248));
#52897=CARTESIAN_POINT('Ctrl Pts',(-0.0769089693951514,0.00881491466990413,
-0.293243139690078));
#52898=CARTESIAN_POINT('Ctrl Pts',(-0.0755273577316007,0.0175539059982861,
-0.293875896472908));
#52899=CARTESIAN_POINT('Ctrl Pts',(-0.0726202453865263,0.0257519380010413,
-0.294508653255738));
#52900=CARTESIAN_POINT('Ctrl Pts',(-0.0641103162918734,0.0497498654211309,
-0.296360908936592));
#52901=CARTESIAN_POINT('Ctrl Pts',(-0.0425284287601913,0.0691123325583359,
-0.298213164617445));
#52902=CARTESIAN_POINT('Ctrl Pts',(-0.0177512410247428,0.0749783688332192,
-0.300065420298299));
#52903=CARTESIAN_POINT('Ctrl Pts',(0.00702594671070583,0.0808444051081026,
-0.301917675979152));
#52904=CARTESIAN_POINT('Ctrl Pts',(0.0349984346499207,0.0732140105206642,
-0.303769931660006));
#52905=CARTESIAN_POINT('Ctrl Pts',(0.0533649929234512,0.0555791317050634,
-0.30562218734086));
#52906=CARTESIAN_POINT('Ctrl Pts',(0.0717315511969815,0.0379442528894627,
-0.307474443021714));
#52907=CARTESIAN_POINT('Ctrl Pts',(0.0804921798048274,0.0103048898457,-0.309326698702568));
#52908=CARTESIAN_POINT('Ctrl Pts',(0.0756376958364942,-0.0146901776488498,
-0.311178954383421));
#52909=CARTESIAN_POINT('Ctrl Pts',(0.0707832118681609,-0.0396852451433996,
-0.313031210064275));
#52910=CARTESIAN_POINT('Ctrl Pts',(0.0523136153236482,-0.0620360170887368,
-0.314883465745128));
#52911=CARTESIAN_POINT('Ctrl Pts',(0.0286812666607068,-0.0715139657238095,
-0.316735721425982));
#52912=CARTESIAN_POINT('Ctrl Pts',(0.00504891799776517,-0.0809919143588823,
-0.318587977106836));
#52913=CARTESIAN_POINT('Ctrl Pts',(-0.0237461827836053,-0.0775970396836909,
-0.32044023278769));
#52914=CARTESIAN_POINT('Ctrl Pts',(-0.0445263481992833,-0.0628829600674536,
-0.322292488468544));
#52915=CARTESIAN_POINT('Ctrl Pts',(-0.0644132222130738,-0.0488014048101396,
-0.324065119948112));
#52916=CARTESIAN_POINT('Ctrl Pts',(-0.0769594369118439,-0.0243529004262267,
-0.32583775142768));
#52917=CARTESIAN_POINT('Ctrl Pts',(-0.0770446167695562,2.01096196933833E-5,
-0.327610382907248));
#52918=CARTESIAN_POINT('Ctrl Pts',(-0.0770389450880675,2.75992272470979E-5,
-0.332639617092753));
#52919=CARTESIAN_POINT('Ctrl Pts',(-0.0769281520716595,-0.0239190056562616,
-0.33089833946598));
#52920=CARTESIAN_POINT('Ctrl Pts',(-0.064880555867624,-0.0479617984574756,
-0.329157061839207));
#52921=CARTESIAN_POINT('Ctrl Pts',(-0.0455817838885432,-0.0621221627301428,
-0.327415784212434));
#52922=CARTESIAN_POINT('Ctrl Pts',(-0.0250530298965668,-0.0771850193152902,
-0.32556352853158));
#52923=CARTESIAN_POINT('Ctrl Pts',(0.00368064245261536,-0.0810656177724936,
-0.323711272850727));
#52924=CARTESIAN_POINT('Ctrl Pts',(0.0274696575640593,-0.071988054828878,
-0.321859017169873));
#52925=CARTESIAN_POINT('Ctrl Pts',(0.0512586726755034,-0.0629104918852623,
-0.320006761489019));
#52926=CARTESIAN_POINT('Ctrl Pts',(0.0701030305492093,-0.040874767540827,
-0.318154505808165));
#52927=CARTESIAN_POINT('Ctrl Pts',(0.0753788662859333,-0.0159652322933174,
-0.316302250127312));
#52928=CARTESIAN_POINT('Ctrl Pts',(0.0806547020226573,0.00894430295419205,
-0.314449994446458));
#52929=CARTESIAN_POINT('Ctrl Pts',(0.0723620156223999,0.0367276491047761,
-0.312597738765605));
#52930=CARTESIAN_POINT('Ctrl Pts',(0.0542958425884615,0.0546701344642687,
-0.310745483084751));
#52931=CARTESIAN_POINT('Ctrl Pts',(0.036229669554523,0.0726126198237612,
-0.308893227403897));
#52932=CARTESIAN_POINT('Ctrl Pts',(0.00839000988690367,0.0807142443921621,
-0.307040971723043));
#52933=CARTESIAN_POINT('Ctrl Pts',(-0.0164826936026276,0.0752674095232067,
-0.30518871604219));
#52934=CARTESIAN_POINT('Ctrl Pts',(-0.0413553970921589,0.0698205746542512,
-0.303336460361336));
#52935=CARTESIAN_POINT('Ctrl Pts',(-0.0632611444036019,0.0508252803479395,
-0.301484204680482));
#52936=CARTESIAN_POINT('Ctrl Pts',(-0.0721750672662027,0.0269744655155819,
-0.299631948999629));
#52937=CARTESIAN_POINT('Ctrl Pts',(-0.0753710790476155,0.0184229572318016,
-0.298967838364003));
#52938=CARTESIAN_POINT('Ctrl Pts',(-0.0768969651883808,0.00924726184010815,
-0.298303727728378));
#52939=CARTESIAN_POINT('Ctrl Pts',(-0.0768387410148688,5.28831155507099E-5,
-0.297639617092753));
#52940=CARTESIAN_POINT('Origin',(0.,0.,-0.2904));
#52941=CARTESIAN_POINT('',(-0.0768380872454154,-5.25393648240572E-5,-0.257610382907248));
#52942=CARTESIAN_POINT('',(-0.0768475938414276,-5.7058424657009E-5,-0.262639617092752));
#52943=CARTESIAN_POINT('',(-0.076925,-9.42059550244101E-18,-0.2904));
#52944=CARTESIAN_POINT('Ctrl Pts',(-0.0768380872454154,-5.25393648240572E-5,
-0.257610382907248));
#52945=CARTESIAN_POINT('Ctrl Pts',(-0.0767348490166546,0.0163660347791766,
-0.258796272271623));
#52946=CARTESIAN_POINT('Ctrl Pts',(-0.0715814297759752,0.0328437608543134,
-0.259982161635997));
#52947=CARTESIAN_POINT('Ctrl Pts',(-0.061863405086039,0.0459323574614827,
-0.261168051000372));
#52948=CARTESIAN_POINT('Ctrl Pts',(-0.0466846987249234,0.0663756029684686,
-0.263020306681225));
#52949=CARTESIAN_POINT('Ctrl Pts',(-0.0203703117315888,0.078550825357997,
-0.264872562362079));
#52950=CARTESIAN_POINT('Ctrl Pts',(0.0050373334427575,0.0768861991686106,
-0.266724818042932));
#52951=CARTESIAN_POINT('Ctrl Pts',(0.0304449786171051,0.0752215729792241,
-0.268577073723786));
#52952=CARTESIAN_POINT('Ctrl Pts',(0.054945881972464,0.0597170982109209,
-0.27042932940464));
#52953=CARTESIAN_POINT('Ctrl Pts',(0.0673275372583098,0.0374681875400943,
-0.272281585085494));
#52954=CARTESIAN_POINT('Ctrl Pts',(0.0797091925441554,0.0152192768692683,
-0.274133840766348));
#52955=CARTESIAN_POINT('Ctrl Pts',(0.0799715997604887,-0.013774069704081,
-0.275986096447201));
#52956=CARTESIAN_POINT('Ctrl Pts',(0.0679946718023306,-0.0362434401968428,
-0.277838352128055));
#52957=CARTESIAN_POINT('Ctrl Pts',(0.0560177438441725,-0.0587128106896046,
-0.279690607808908));
#52958=CARTESIAN_POINT('Ctrl Pts',(0.031801480711523,-0.074658205101779,
-0.281542863489762));
#52959=CARTESIAN_POINT('Ctrl Pts',(0.00642812691598172,-0.0767824298597068,
-0.283395119170616));
#52960=CARTESIAN_POINT('Ctrl Pts',(-0.0189452268795601,-0.0789066546176347,
-0.28524737485147));
#52961=CARTESIAN_POINT('Ctrl Pts',(-0.0454756713379933,-0.0672097097213156,
-0.287099630532323));
#52962=CARTESIAN_POINT('Ctrl Pts',(-0.0610219082383983,-0.0470445434216687,
-0.288951886213177));
#52963=CARTESIAN_POINT('Ctrl Pts',(-0.0712573303588049,-0.0337680836245259,
-0.2901713851112));
#52964=CARTESIAN_POINT('Ctrl Pts',(-0.076731407113569,-0.0168208877710075,
-0.291390884009224));
#52965=CARTESIAN_POINT('Ctrl Pts',(-0.0768483116041091,5.73613550720782E-5,
-0.292610382907248));
#52966=CARTESIAN_POINT('Ctrl Pts',(-0.0768387410148688,5.28831155507099E-5,
-0.297639617092753));
#52967=CARTESIAN_POINT('Ctrl Pts',(-0.0767345734868098,-0.0163965681347663,
-0.296451472047524));
#52968=CARTESIAN_POINT('Ctrl Pts',(-0.0715599913475533,-0.0329058209298907,
-0.295263327002296));
#52969=CARTESIAN_POINT('Ctrl Pts',(-0.0618075588824273,-0.0460074753678952,
-0.294075181957067));
#52970=CARTESIAN_POINT('Ctrl Pts',(-0.0466040292222927,-0.0664322660606102,
-0.292222926276214));
#52971=CARTESIAN_POINT('Ctrl Pts',(-0.0202748714882653,-0.0785755120876367,
-0.29037067059536));
#52972=CARTESIAN_POINT('Ctrl Pts',(0.00513073223922229,-0.0768800215362977,
-0.288518414914506));
#52973=CARTESIAN_POINT('Ctrl Pts',(0.0305363359667096,-0.0751845309849588,
-0.286666159233653));
#52974=CARTESIAN_POINT('Ctrl Pts',(0.0550183856876571,-0.0596503038552547,
-0.284813903552799));
#52975=CARTESIAN_POINT('Ctrl Pts',(0.0673730032617221,-0.0373863685884066,
-0.282961647871945));
#52976=CARTESIAN_POINT('Ctrl Pts',(0.0797276208357874,-0.0151224333215578,
-0.281109392191092));
#52977=CARTESIAN_POINT('Ctrl Pts',(0.0799548062629695,0.0138712100824353,
-0.279257136510238));
#52978=CARTESIAN_POINT('Ctrl Pts',(0.0679505912125762,0.0363260137999418,
-0.277404880829384));
#52979=CARTESIAN_POINT('Ctrl Pts',(0.0559463761621832,0.0587808175174479,
-0.275552625148531));
#52980=CARTESIAN_POINT('Ctrl Pts',(0.0317107606342153,0.0746967815484678,
-0.273700369467677));
#52981=CARTESIAN_POINT('Ctrl Pts',(0.00633484550162029,0.0767901807342762,
-0.271848113786823));
#52982=CARTESIAN_POINT('Ctrl Pts',(-0.0190410696309747,0.0788835799200847,
-0.269995858105969));
#52983=CARTESIAN_POINT('Ctrl Pts',(-0.0455572843681968,0.0671544142606818,
-0.268143602425116));
#52984=CARTESIAN_POINT('Ctrl Pts',(-0.0610790125281194,0.0469703774023803,
-0.266291346744262));
#52985=CARTESIAN_POINT('Ctrl Pts',(-0.0712793960479106,0.0337060736592007,
-0.265074103527092));
#52986=CARTESIAN_POINT('Ctrl Pts',(-0.076731592629824,0.016790366214193,
-0.263856860309922));
#52987=CARTESIAN_POINT('Ctrl Pts',(-0.0768475938414276,-5.7058424657009E-5,
-0.262639617092752));
#52988=CARTESIAN_POINT('Origin',(0.,0.,-0.2904));
#52989=CARTESIAN_POINT('',(-0.0770384785824837,-2.81238608518045E-5,-0.222610382907248));
#52990=CARTESIAN_POINT('',(-0.0770442613572831,-2.06596519778444E-5,-0.227639617092753));
#52991=CARTESIAN_POINT('',(-0.076925,-9.42059550244101E-18,-0.2904));
#52992=CARTESIAN_POINT('Ctrl Pts',(-0.0770384785824837,-2.81238608518045E-5,
-0.222610382907248));
#52993=CARTESIAN_POINT('Ctrl Pts',(-0.0769260041526005,0.0238878470797757,
-0.224349404853167));
#52994=CARTESIAN_POINT('Ctrl Pts',(-0.0649137963482565,0.0479013199546961,
-0.226088426799086));
#52995=CARTESIAN_POINT('Ctrl Pts',(-0.0456572181419577,0.0620667445766768,
-0.227827448745005));
#52996=CARTESIAN_POINT('Ctrl Pts',(-0.0251467775117378,0.0771545290001813,
-0.229679704425858));
#52997=CARTESIAN_POINT('Ctrl Pts',(0.00358215996774758,0.0810700308031899,
-0.231531960106712));
#52998=CARTESIAN_POINT('Ctrl Pts',(0.0273821855504783,0.0720213736698207,
-0.233384215787566));
#52999=CARTESIAN_POINT('Ctrl Pts',(0.0511822111332089,0.0629727165364516,
-0.23523647146842));
#53000=CARTESIAN_POINT('Ctrl Pts',(0.0700533248191852,0.0409599004667053,
-0.237088727149273));
#53001=CARTESIAN_POINT('Ctrl Pts',(0.0753594172744191,0.0160567922969925,
-0.238940982830127));
#53002=CARTESIAN_POINT('Ctrl Pts',(0.0806655097296531,-0.00884631587272035,
-0.240793238510981));
#53003=CARTESIAN_POINT('Ctrl Pts',(0.0724065809541445,-0.0366397161423994,
-0.242645494191834));
#53004=CARTESIAN_POINT('Ctrl Pts',(0.0543622177318953,-0.0546041356865831,
-0.244497749872688));
#53005=CARTESIAN_POINT('Ctrl Pts',(0.0363178545096461,-0.0725685552307669,
-0.246350005553542));
#53006=CARTESIAN_POINT('Ctrl Pts',(0.00848805684065565,-0.0807039940494551,
-0.248202261234396));
#53007=CARTESIAN_POINT('Ctrl Pts',(-0.0163912456732748,-0.0752873788631742,
-0.250054516915249));
#53008=CARTESIAN_POINT('Ctrl Pts',(-0.0412705481872051,-0.0698707636768933,
-0.251906772596103));
#53009=CARTESIAN_POINT('Ctrl Pts',(-0.0631993555460757,-0.0509020944856437,
-0.253759028276956));
#53010=CARTESIAN_POINT('Ctrl Pts',(-0.0721422463610633,-0.0270621255777965,
-0.25561128395781));
#53011=CARTESIAN_POINT('Ctrl Pts',(-0.0753595350284208,-0.0184854736445279,
-0.256277650274289));
#53012=CARTESIAN_POINT('Ctrl Pts',(-0.0768960981191831,-0.00927834499463494,
-0.256944016590769));
#53013=CARTESIAN_POINT('Ctrl Pts',(-0.0768380872454154,-5.25393648240572E-5,
-0.257610382907248));
#53014=CARTESIAN_POINT('Ctrl Pts',(-0.0768475938414276,-5.7058424657009E-5,
-0.262639617092752));
#53015=CARTESIAN_POINT('Ctrl Pts',(-0.0769081094509062,-0.00884603705747186,
-0.262004604629068));
#53016=CARTESIAN_POINT('Ctrl Pts',(-0.0755163746955851,-0.0176164324632363,
-0.261369592165385));
#53017=CARTESIAN_POINT('Ctrl Pts',(-0.0725889065436049,-0.0258401387677387,
-0.260734579701701));
#53018=CARTESIAN_POINT('Ctrl Pts',(-0.0640498308165448,-0.0498277100223563,
-0.258882324020847));
#53019=CARTESIAN_POINT('Ctrl Pts',(-0.042444437779801,-0.0691639444743909,
-0.257030068339994));
#53020=CARTESIAN_POINT('Ctrl Pts',(-0.0176601426423535,-0.0749998765771247,
-0.25517781265914));
#53021=CARTESIAN_POINT('Ctrl Pts',(0.00712415249509371,-0.0808358086798583,
-0.253325556978286));
#53022=CARTESIAN_POINT('Ctrl Pts',(0.0350873497332448,-0.0731714384332915,
-0.251473301297432));
#53023=CARTESIAN_POINT('Ctrl Pts',(0.0534324709660324,-0.0555142609713604,
-0.249621045616579));
#53024=CARTESIAN_POINT('Ctrl Pts',(0.0717775921988202,-0.0378570835094291,
-0.247768789935725));
#53025=CARTESIAN_POINT('Ctrl Pts',(0.0805046374262445,-0.0102070988321336,
-0.245916534254871));
#53026=CARTESIAN_POINT('Ctrl Pts',(0.0756197927165552,0.0147820524365676,
-0.244064278574018));
#53027=CARTESIAN_POINT('Ctrl Pts',(0.0707349480068659,0.0397712037052691,
-0.242212022893164));
#53028=CARTESIAN_POINT('Ctrl Pts',(0.0522382133600625,0.0620995215653761,
-0.24035976721231));
#53029=CARTESIAN_POINT('Ctrl Pts',(0.0285943686184854,0.0715487540635222,
-0.238507511531456));
#53030=CARTESIAN_POINT('Ctrl Pts',(0.00495052387690865,0.0809979865616681,
-0.236655255850603));
#53031=CARTESIAN_POINT('Ctrl Pts',(-0.0238404309594419,0.0775681336978536,
-0.234803000169749));
#53032=CARTESIAN_POINT('Ctrl Pts',(-0.0446027057419749,0.0628288211351049,
-0.232950744488896));
#53033=CARTESIAN_POINT('Ctrl Pts',(-0.0644471738579057,0.0487410672032344,
-0.231180368690181));
#53034=CARTESIAN_POINT('Ctrl Pts',(-0.0769570964452667,0.0243216340277852,
-0.229409992891467));
#53035=CARTESIAN_POINT('Ctrl Pts',(-0.0770442613572831,-2.06596519778444E-5,
-0.227639617092753));
#53036=CARTESIAN_POINT('Origin',(0.,0.,-0.2904));
#53037=CARTESIAN_POINT('',(-0.0769213030505415,7.03209464845075E-5,-0.187610382907248));
#53038=CARTESIAN_POINT('',(-0.0769083233862821,7.01032878403822E-5,-0.192639617092753));
#53039=CARTESIAN_POINT('',(-0.076925,-9.42059550244101E-18,-0.2904));
#53040=CARTESIAN_POINT('Ctrl Pts',(-0.0769213030505415,7.03209464845076E-5,
-0.187610382907248));
#53041=CARTESIAN_POINT('Ctrl Pts',(-0.0769768969517964,0.00614402362538094,
-0.188050281753858));
#53042=CARTESIAN_POINT('Ctrl Pts',(-0.0763180708120862,0.0122058064274764,
-0.188490180600467));
#53043=CARTESIAN_POINT('Ctrl Pts',(-0.0748988104695978,0.0180839857623078,
-0.188930079447077));
#53044=CARTESIAN_POINT('Ctrl Pts',(-0.0689228160966994,0.042834882814957,
-0.190782335127931));
#53045=CARTESIAN_POINT('Ctrl Pts',(-0.0494647117111675,0.0643305841711047,
-0.192634590808785));
#53046=CARTESIAN_POINT('Ctrl Pts',(-0.0254292349826108,0.0727338735322628,
-0.194486846489638));
#53047=CARTESIAN_POINT('Ctrl Pts',(-0.00139375825405342,0.0811371628934212,
-0.196339102170492));
#53048=CARTESIAN_POINT('Ctrl Pts',(0.027219090817529,0.0764480402595892,
-0.198191357851346));
#53049=CARTESIAN_POINT('Ctrl Pts',(0.0473150297721676,0.0608124190315364,
-0.200043613532199));
#53050=CARTESIAN_POINT('Ctrl Pts',(0.0674109687268059,0.0451767978034838,
-0.201895869213053));
#53051=CARTESIAN_POINT('Ctrl Pts',(0.0789899975645006,0.0185946779812107,
-0.203748124893907));
#53052=CARTESIAN_POINT('Ctrl Pts',(0.0767531307198992,-0.00676899368468636,
-0.20560038057476));
#53053=CARTESIAN_POINT('Ctrl Pts',(0.0745162638752978,-0.0321326653505834,
-0.207452636255614));
#53054=CARTESIAN_POINT('Ctrl Pts',(0.0584635013484002,-0.0562778888601044,
-0.209304891936468));
#53055=CARTESIAN_POINT('Ctrl Pts',(0.0359411722749404,-0.0681549300220585,
-0.211157147617321));
#53056=CARTESIAN_POINT('Ctrl Pts',(0.0134188432014803,-0.0800319711840128,
-0.213009403298175));
#53057=CARTESIAN_POINT('Ctrl Pts',(-0.0155730524185423,-0.0796408299983998,
-0.214861658979029));
#53058=CARTESIAN_POINT('Ctrl Pts',(-0.0377667666111407,-0.0671605069259333,
-0.216713914659883));
#53059=CARTESIAN_POINT('Ctrl Pts',(-0.0599604808037389,-0.054680183853467,
-0.218566170340736));
#53060=CARTESIAN_POINT('Ctrl Pts',(-0.0753560135689132,-0.0301106788941475,
-0.22041842602159));
#53061=CARTESIAN_POINT('Ctrl Pts',(-0.0769078080610228,-0.00469589289248762,
-0.222270681702444));
#53062=CARTESIAN_POINT('Ctrl Pts',(-0.077002673736431,-0.00314221368325,
-0.222383915437378));
#53063=CARTESIAN_POINT('Ctrl Pts',(-0.0770458021817116,-0.00158537546457811,
-0.222497149172313));
#53064=CARTESIAN_POINT('Ctrl Pts',(-0.0770384785824837,-2.81238608518045E-5,
-0.222610382907248));
#53065=CARTESIAN_POINT('Ctrl Pts',(-0.0770442613572831,-2.06596519778444E-5,
-0.227639617092753));
#53066=CARTESIAN_POINT('Ctrl Pts',(-0.0770482927345352,-0.0011464907545882,
-0.227557737210613));
#53067=CARTESIAN_POINT('Ctrl Pts',(-0.077025751055757,-0.00227215685099022,
-0.227475857328474));
#53068=CARTESIAN_POINT('Ctrl Pts',(-0.0769761329357462,-0.00339662817961441,
-0.227393977446334));
#53069=CARTESIAN_POINT('Ctrl Pts',(-0.0758536906182689,-0.0288339926699021,
-0.225541721765481));
#53070=CARTESIAN_POINT('Ctrl Pts',(-0.0608752112545988,-0.0536599493887943,
-0.223689466084627));
#53071=CARTESIAN_POINT('Ctrl Pts',(-0.0388953928553611,-0.0665132358208449,
-0.221837210403773));
#53072=CARTESIAN_POINT('Ctrl Pts',(-0.0169155744561231,-0.0793665222528957,
-0.21998495472292));
#53073=CARTESIAN_POINT('Ctrl Pts',(0.0120655829786826,-0.0802471383981044,
-0.218132699042066));
#53074=CARTESIAN_POINT('Ctrl Pts',(0.0347852456599467,-0.0687520822165361,
-0.216280443361212));
#53075=CARTESIAN_POINT('Ctrl Pts',(0.0575049083412103,-0.057257026034968,
-0.214428187680358));
#53076=CARTESIAN_POINT('Ctrl Pts',(0.0739630762689327,-0.033386297526623,
-0.212575931999505));
#53077=CARTESIAN_POINT('Ctrl Pts',(0.0766278920219695,-0.00806401196686029,
-0.210723676318651));
#53078=CARTESIAN_POINT('Ctrl Pts',(0.0792927077750063,0.0172582735929026,
-0.208871420637797));
#53079=CARTESIAN_POINT('Ctrl Pts',(0.0681641713533576,0.0440321162040837,
-0.207019164956944));
#53080=CARTESIAN_POINT('Ctrl Pts',(0.0483351065756888,0.0600048297810181,
-0.20516690927609));
#53081=CARTESIAN_POINT('Ctrl Pts',(0.0285060417980199,0.0759775433579526,
-0.203314653595236));
#53082=CARTESIAN_POINT('Ctrl Pts',(-2.35513356690899E-5,0.0811491279006402,
-0.201462397914382));
#53083=CARTESIAN_POINT('Ctrl Pts',(-0.0241974913166144,0.0731528778566806,
-0.199610142233529));
#53084=CARTESIAN_POINT('Ctrl Pts',(-0.0483714312975601,0.0651566278127208,
-0.197757886552675));
#53085=CARTESIAN_POINT('Ctrl Pts',(-0.0681897181257618,0.0439925431821134,
-0.195905630871822));
#53086=CARTESIAN_POINT('Ctrl Pts',(-0.074582781519945,0.0193460803647884,
-0.194053375190968));
#53087=CARTESIAN_POINT('Ctrl Pts',(-0.0762093109527435,0.0130755032228149,
-0.193582122491563));
#53088=CARTESIAN_POINT('Ctrl Pts',(-0.0769668252245155,0.00657951162457119,
-0.193110869792158));
#53089=CARTESIAN_POINT('Ctrl Pts',(-0.0769083233862821,7.01032878403821E-5,
-0.192639617092753));
#53090=CARTESIAN_POINT('Origin',(0.,0.,-0.2904));
#53091=CARTESIAN_POINT('',(-0.0768014403980194,-1.51076210625975E-5,-0.152610382907248));
#53092=CARTESIAN_POINT('',(-0.0768045683068413,-2.19932982921254E-5,-0.157639617092752));
#53093=CARTESIAN_POINT('',(-0.076925,-9.42059550244101E-18,-0.2904));
#53094=CARTESIAN_POINT('Ctrl Pts',(-0.0768014403980194,-1.51076210625975E-5,
-0.152610382907248));
#53095=CARTESIAN_POINT('Ctrl Pts',(-0.0767772777264159,0.0137497882837818,
-0.153603414335402));
#53096=CARTESIAN_POINT('Ctrl Pts',(-0.0732496519640692,0.0275262395484409,
-0.154596445763557));
#53097=CARTESIAN_POINT('Ctrl Pts',(-0.0662922196675392,0.0392709047833103,
-0.155589477191711));
#53098=CARTESIAN_POINT('Ctrl Pts',(-0.0533148423861816,0.0611776866677943,
-0.157441732872564));
#53099=CARTESIAN_POINT('Ctrl Pts',(-0.0284045786794063,0.0760155357443801,
-0.159293988553418));
#53100=CARTESIAN_POINT('Ctrl Pts',(-0.00296127301607803,0.076994111547066,
-0.161146244234272));
#53101=CARTESIAN_POINT('Ctrl Pts',(0.0224820326472499,0.0779726873497518,
-0.162998499915125));
#53102=CARTESIAN_POINT('Ctrl Pts',(0.0484583802671308,0.0650919898785382,
-0.164850755595979));
#53103=CARTESIAN_POINT('Ctrl Pts',(0.0630800465304561,0.0442466957013912,
-0.166703011276833));
#53104=CARTESIAN_POINT('Ctrl Pts',(0.0777017127937813,0.0234014015242443,
-0.168555266957687));
#53105=CARTESIAN_POINT('Ctrl Pts',(0.0809686977005509,-0.00540848935883606,
-0.17040752263854));
#53106=CARTESIAN_POINT('Ctrl Pts',(0.0713859098992575,-0.0289985209741058,
-0.172259778319394));
#53107=CARTESIAN_POINT('Ctrl Pts',(0.0618031220979642,-0.0525885525893755,
-0.174112034000248));
#53108=CARTESIAN_POINT('Ctrl Pts',(0.0393705615886079,-0.0709587249368346,
-0.175964289681101));
#53109=CARTESIAN_POINT('Ctrl Pts',(0.0143541855602173,-0.0757021776946229,
-0.177816545361955));
#53110=CARTESIAN_POINT('Ctrl Pts',(-0.0106621904681737,-0.0804456304524112,
-0.179668801042809));
#53111=CARTESIAN_POINT('Ctrl Pts',(-0.0382623820155991,-0.0715623636205283,
-0.181521056723662));
#53112=CARTESIAN_POINT('Ctrl Pts',(-0.0558155356091798,-0.053117683830011,
-0.183373312404516));
#53113=CARTESIAN_POINT('Ctrl Pts',(-0.0691999277839148,-0.0390534972131984,
-0.18478566923876));
#53114=CARTESIAN_POINT('Ctrl Pts',(-0.0767428110472438,-0.0194301518413298,
-0.186198026073004));
#53115=CARTESIAN_POINT('Ctrl Pts',(-0.0769213030505415,7.03209464845076E-5,
-0.187610382907248));
#53116=CARTESIAN_POINT('Ctrl Pts',(-0.0769083233862821,7.01032878403821E-5,
-0.192639617092753));
#53117=CARTESIAN_POINT('Ctrl Pts',(-0.0767368841284859,-0.0190056756558977,
-0.191258614111304));
#53118=CARTESIAN_POINT('Ctrl Pts',(-0.0695576680328398,-0.0381966747626404,
-0.189877611129855));
#53119=CARTESIAN_POINT('Ctrl Pts',(-0.0567044741044506,-0.0521676599175141,
-0.188496608148407));
#53120=CARTESIAN_POINT('Ctrl Pts',(-0.039465263334608,-0.0709060963784499,
-0.186644352467553));
#53121=CARTESIAN_POINT('Ctrl Pts',(-0.0120190018347582,-0.0802541282962796,
-0.184792096786699));
#53122=CARTESIAN_POINT('Ctrl Pts',(0.0130739009213669,-0.0759337555994022,
-0.182939841105846));
#53123=CARTESIAN_POINT('Ctrl Pts',(0.0381668036774915,-0.0716133829025249,
-0.181087585424992));
#53124=CARTESIAN_POINT('Ctrl Pts',(0.0609063476898911,-0.0536246055909411,
-0.179235329744138));
#53125=CARTESIAN_POINT('Ctrl Pts',(0.0708860889317149,-0.0301997437191199,
-0.177383074063285));
#53126=CARTESIAN_POINT('Ctrl Pts',(0.080865830173539,-0.00677488184729807,
-0.175530818382431));
#53127=CARTESIAN_POINT('Ctrl Pts',(0.0780857686447859,0.0220860645847622,
-0.173678562701577));
#53128=CARTESIAN_POINT('Ctrl Pts',(0.0638181618136476,0.0431752747235632,
-0.171826307020723));
#53129=CARTESIAN_POINT('Ctrl Pts',(0.0495505549825093,0.0642644848623639,
-0.16997405133987));
#53130=CARTESIAN_POINT('Ctrl Pts',(0.0237954028489864,0.0775819587079064,
-0.168121795659016));
#53131=CARTESIAN_POINT('Ctrl Pts',(-0.00166079838775686,0.0770331349059874,
-0.166269539978162));
#53132=CARTESIAN_POINT('Ctrl Pts',(-0.0271169996245001,0.0764843111040684,
-0.164417284297309));
#53133=CARTESIAN_POINT('Ctrl Pts',(-0.0522742499644634,0.0620691896546879,
-0.162565028616455));
#53134=CARTESIAN_POINT('Ctrl Pts',(-0.0656196748575325,0.0403846554565688,
-0.160712772935601));
#53135=CARTESIAN_POINT('Ctrl Pts',(-0.07300032806313,0.0283920791149677,
-0.159688387654652));
#53136=CARTESIAN_POINT('Ctrl Pts',(-0.0767681988336545,0.0141760694175307,
-0.158664002373702));
#53137=CARTESIAN_POINT('Ctrl Pts',(-0.0768045683068413,-2.19932982921254E-5,
-0.157639617092752));
#53138=CARTESIAN_POINT('Origin',(0.,0.,-0.2904));
#53139=CARTESIAN_POINT('',(-0.0769767170183498,-6.24120630863603E-5,-0.117610382907248));
#53140=CARTESIAN_POINT('',(-0.0769889244048768,-5.85269688276939E-5,-0.122639617092752));
#53141=CARTESIAN_POINT('',(-0.076925,-9.42059550244101E-18,-0.2904));
#53142=CARTESIAN_POINT('Ctrl Pts',(-0.0769767170183498,-6.24120630863603E-5,
-0.117610382907248));
#53143=CARTESIAN_POINT('Ctrl Pts',(-0.0767891818127649,0.0212460239503849,
-0.119156546916947));
#53144=CARTESIAN_POINT('Ctrl Pts',(-0.0675691351190549,0.0426968904112383,
-0.120702710926645));
#53145=CARTESIAN_POINT('Ctrl Pts',(-0.0518461623588979,0.0569985772172947,
-0.122248874936344));
#53146=CARTESIAN_POINT('Ctrl Pts',(-0.0330105372685272,0.0741315465957961,
-0.124101130617198));
#53147=CARTESIAN_POINT('Ctrl Pts',(-0.00484237846485304,0.0810045253994228,
-0.125953386298051));
#53148=CARTESIAN_POINT('Ctrl Pts',(0.0197675379063687,0.0744721880741092,
-0.127805641978905));
#53149=CARTESIAN_POINT('Ctrl Pts',(0.0443774542775902,0.0679398507487956,
-0.129657897659759));
#53150=CARTESIAN_POINT('Ctrl Pts',(0.0654291282163597,0.0480021972945419,
-0.131510153340613));
#53151=CARTESIAN_POINT('Ctrl Pts',(0.0732885466351915,0.0237834245026632,
-0.133362409021466));
#53152=CARTESIAN_POINT('Ctrl Pts',(0.0811479650540234,-0.000435348289215827,
-0.13521466470232));
#53153=CARTESIAN_POINT('Ctrl Pts',(0.0758151279529177,-0.0289352404187193,
-0.137066920383174));
#53154=CARTESIAN_POINT('Ctrl Pts',(0.0597305358875067,-0.0486736626347264,
-0.138919176064027));
#53155=CARTESIAN_POINT('Ctrl Pts',(0.0436459438220958,-0.0684120848507334,
-0.140771431744881));
#53156=CARTESIAN_POINT('Ctrl Pts',(0.0168095967923794,-0.0793890371532433,
-0.142623687425735));
#53157=CARTESIAN_POINT('Ctrl Pts',(-0.00849721479305223,-0.0765810661428619,
-0.144475943106588));
#53158=CARTESIAN_POINT('Ctrl Pts',(-0.0338040263784831,-0.0737730951324806,
-0.146328198787442));
#53159=CARTESIAN_POINT('Ctrl Pts',(-0.0575813025196296,-0.0571802008092089,
-0.148180454468296));
#53160=CARTESIAN_POINT('Ctrl Pts',(-0.068947695162233,-0.0343958963013827,
-0.150032710149149));
#53161=CARTESIAN_POINT('Ctrl Pts',(-0.074220336690712,-0.0238267145105662,
-0.150891934401849));
#53162=CARTESIAN_POINT('Ctrl Pts',(-0.0768223472423177,-0.0119252366079264,
-0.151751158654548));
#53163=CARTESIAN_POINT('Ctrl Pts',(-0.0768014403980194,-1.51076210625975E-5,
-0.152610382907248));
#53164=CARTESIAN_POINT('Ctrl Pts',(-0.0768045683068413,-2.19932982921254E-5,
-0.157639617092752));
#53165=CARTESIAN_POINT('Ctrl Pts',(-0.0768339607735931,-0.0114963438937193,
-0.156811746692848));
#53166=CARTESIAN_POINT('Ctrl Pts',(-0.0744262066756044,-0.0229589728197424,
-0.155983876292944));
#53167=CARTESIAN_POINT('Ctrl Pts',(-0.0695186422021508,-0.0332268041055519,
-0.15515600589304));
#53168=CARTESIAN_POINT('Ctrl Pts',(-0.0585385852075251,-0.0561997825226952,
-0.153303750212186));
#53169=CARTESIAN_POINT('Ctrl Pts',(-0.0350448717720988,-0.0731917924101241,
-0.151451494531333));
#53170=CARTESIAN_POINT('Ctrl Pts',(-0.0097890813327328,-0.0764266708118463,
-0.149599238850479));
#53171=CARTESIAN_POINT('Ctrl Pts',(0.0154667091066325,-0.0796615492135685,
-0.147746983169625));
#53172=CARTESIAN_POINT('Ctrl Pts',(0.0424845765499378,-0.0691392961295849,
-0.145894727488772));
#53173=CARTESIAN_POINT('Ctrl Pts',(0.058900160252147,-0.0496752780278504,
-0.144042471807918));
#53174=CARTESIAN_POINT('Ctrl Pts',(0.0753157439543566,-0.0302112599261153,
-0.142190216127064));
#53175=CARTESIAN_POINT('Ctrl Pts',(0.0811290439154697,-0.00180547680662942,
-0.140337960446211));
#53176=CARTESIAN_POINT('Ctrl Pts',(0.0736796822281447,0.0225425497946054,
-0.138485704765357));
#53177=CARTESIAN_POINT('Ctrl Pts',(0.0662303205408196,0.0468905763958403,
-0.136633449084503));
#53178=CARTESIAN_POINT('Ctrl Pts',(0.0455182972050559,0.0671808464788235,
-0.13478119340365));
#53179=CARTESIAN_POINT('Ctrl Pts',(0.0210221888861179,0.0741277930278272,
-0.132928937722796));
#53180=CARTESIAN_POINT('Ctrl Pts',(-0.00347391943281973,0.0810747395768307,
-0.131076682041942));
#53181=CARTESIAN_POINT('Ctrl Pts',(-0.031754112734932,0.0746783625918553,
-0.129224426361088));
#53182=CARTESIAN_POINT('Ctrl Pts',(-0.050876343940606,0.0578658772753876,
-0.127372170680235));
#53183=CARTESIAN_POINT('Ctrl Pts',(-0.0671622496120032,0.0435471219470607,
-0.12579465281774));
#53184=CARTESIAN_POINT('Ctrl Pts',(-0.0768054414749702,0.0216730583618212,
-0.124217134955246));
#53185=CARTESIAN_POINT('Ctrl Pts',(-0.0769889244048768,-5.85269688276939E-5,
-0.122639617092752));
#53186=CARTESIAN_POINT('Origin',(0.,0.,-0.2904));
#53187=CARTESIAN_POINT('',(-0.076999203572401,5.4492118465423E-5,-0.0826103829072478));
#53188=CARTESIAN_POINT('',(-0.0769875287350775,5.90179537171767E-5,-0.0876396170927523));
#53189=CARTESIAN_POINT('',(-0.076925,-9.42059550244101E-18,-0.2904));
#53190=CARTESIAN_POINT('Ctrl Pts',(-0.076999203572401,5.4492118465423E-5,
-0.0826103829072478));
#53191=CARTESIAN_POINT('Ctrl Pts',(-0.0770265285682266,0.00345649638462249,
-0.0828574238176373));
#53192=CARTESIAN_POINT('Ctrl Pts',(-0.0768205763822429,0.00685517124978457,
-0.0831044647280268));
#53193=CARTESIAN_POINT('Ctrl Pts',(-0.0763700887674245,0.0102211183005622,
-0.0833515056384164));
#53194=CARTESIAN_POINT('Ctrl Pts',(-0.0729924366919608,0.0354582117699201,
-0.08520376131927));
#53195=CARTESIAN_POINT('Ctrl Pts',(-0.0558678488876682,0.0588554607511704,
-0.0870560170001238));
#53196=CARTESIAN_POINT('Ctrl Pts',(-0.032833146889111,0.0697054301112457,
-0.0889082726809775));
#53197=CARTESIAN_POINT('Ctrl Pts',(-0.00979844489055356,0.0805553994713211,
-0.0907605283618312));
#53198=CARTESIAN_POINT('Ctrl Pts',(0.0191463713022683,0.0788580892102209,
-0.0926127840426848));
#53199=CARTESIAN_POINT('Ctrl Pts',(0.0407550916409124,0.0653902510666844,
-0.0944650397235385));
#53200=CARTESIAN_POINT('Ctrl Pts',(0.0623638119795563,0.051922412923148,
-0.0963172954043922));
#53201=CARTESIAN_POINT('Ctrl Pts',(0.0766364364640223,0.0266840468971758,
-0.0981695510852459));
#53202=CARTESIAN_POINT('Ctrl Pts',(0.0770412958690424,0.00122514865842206,
-0.1000218067661));
#53203=CARTESIAN_POINT('Ctrl Pts',(0.0774461552740624,-0.0242337495803313,
-0.101874062446953));
#53204=CARTESIAN_POINT('Ctrl Pts',(0.0639832495996361,-0.0499131800318667,
-0.103726318127807));
#53205=CARTESIAN_POINT('Ctrl Pts',(0.0428136930638241,-0.0640612993006833,
-0.105578573808661));
#53206=CARTESIAN_POINT('Ctrl Pts',(0.0216441365280112,-0.0782094185695004,
-0.107430829489514));
#53207=CARTESIAN_POINT('Ctrl Pts',(-0.00723207086918824,-0.0808262266555986,
-0.109283085170368));
#53208=CARTESIAN_POINT('Ctrl Pts',(-0.0306001232239576,-0.0707141769196905,
-0.111135340851222));
#53209=CARTESIAN_POINT('Ctrl Pts',(-0.0539681755787259,-0.0606021271837827,
-0.112987596532076));
#53210=CARTESIAN_POINT('Ctrl Pts',(-0.0718280728910644,-0.0377612196258701,
-0.114839852212929));
#53211=CARTESIAN_POINT('Ctrl Pts',(-0.0760064758587001,-0.0126442858702262,
-0.116692107893783));
#53212=CARTESIAN_POINT('Ctrl Pts',(-0.0766969714313918,-0.00849362551214272,
-0.116998199564938));
#53213=CARTESIAN_POINT('Ctrl Pts',(-0.0770138430697374,-0.00428080981917798,
-0.117304291236093));
#53214=CARTESIAN_POINT('Ctrl Pts',(-0.0769767170183498,-6.24120630863603E-5,
-0.117610382907248));
#53215=CARTESIAN_POINT('Ctrl Pts',(-0.0769889244048768,-5.85269688276939E-5,
-0.122639617092752));
#53216=CARTESIAN_POINT('Ctrl Pts',(-0.0770208794787732,-0.00384326277764943,
-0.122364879274393));
#53217=CARTESIAN_POINT('Ctrl Pts',(-0.0767659110702742,-0.00762367706270524,
-0.122090141456033));
#53218=CARTESIAN_POINT('Ctrl Pts',(-0.0762091386433896,-0.0113591069246425,
-0.121815403637674));
#53219=CARTESIAN_POINT('Ctrl Pts',(-0.072455433031263,-0.0365430121602462,
-0.11996314795682));
#53220=CARTESIAN_POINT('Ctrl Pts',(-0.0549837526977732,-0.059682228983493,
-0.118110892275966));
#53221=CARTESIAN_POINT('Ctrl Pts',(-0.0317897751949185,-0.0701874085460173,
-0.116258636595113));
#53222=CARTESIAN_POINT('Ctrl Pts',(-0.00859579769206384,-0.0806925881085414,
-0.114406380914259));
#53223=CARTESIAN_POINT('Ctrl Pts',(0.0203204769801554,-0.078563730410343,
-0.112554125233405));
#53224=CARTESIAN_POINT('Ctrl Pts',(0.0417259075957495,-0.0647750782738639,
-0.110701869552551));
#53225=CARTESIAN_POINT('Ctrl Pts',(0.0631313382113431,-0.0509864261373853,
-0.108849613871698));
#53226=CARTESIAN_POINT('Ctrl Pts',(0.0770259247703119,-0.0255379795626259,
-0.106997358190844));
#53227=CARTESIAN_POINT('Ctrl Pts',(0.077050998400323,-7.58751863531738E-5,
-0.10514510250999));
#53228=CARTESIAN_POINT('Ctrl Pts',(0.0770760720303342,0.0253862291899199,
-0.103292846829137));
#53229=CARTESIAN_POINT('Ctrl Pts',(0.0632316327313878,0.0508619913677072,
-0.101440591148283));
#53230=CARTESIAN_POINT('Ctrl Pts',(0.0418533999014276,0.0646927743211912,
-0.0995883354674292));
#53231=CARTESIAN_POINT('Ctrl Pts',(0.0204751670714671,0.0785235572746754,
-0.0977360797865755));
#53232=CARTESIAN_POINT('Ctrl Pts',(-0.00843685928950717,0.0807093610038558,
-0.0958838241057219));
#53233=CARTESIAN_POINT('Ctrl Pts',(-0.0316514812450822,0.0702498817851143,
-0.0940315684248682));
#53234=CARTESIAN_POINT('Ctrl Pts',(-0.054866103200657,0.0597904025663729,
-0.0921793127440145));
#53235=CARTESIAN_POINT('Ctrl Pts',(-0.0723833207508324,0.03668564039971,
-0.0903270570631607));
#53236=CARTESIAN_POINT('Ctrl Pts',(-0.0761866187557145,0.0115091769813019,
-0.088474801382307));
#53237=CARTESIAN_POINT('Ctrl Pts',(-0.0767582559537188,0.00772514454795501,
-0.0881964066191221));
#53238=CARTESIAN_POINT('Ctrl Pts',(-0.0770200928405554,0.00389431194997852,
-0.0879180118559372));
#53239=CARTESIAN_POINT('Ctrl Pts',(-0.0769875287350775,5.90179537171767E-5,
-0.0876396170927523));
#53240=CARTESIAN_POINT('Origin',(0.,0.,-0.2904));
#53241=CARTESIAN_POINT('',(-0.0768084924694757,2.79143412051236E-5,-0.0476103829072477));
#53242=CARTESIAN_POINT('',(-0.0768041739443497,2.12084165925656E-5,-0.0526396170927524));
#53243=CARTESIAN_POINT('',(-0.076925,-9.42059550244101E-18,-0.2904));
#53244=CARTESIAN_POINT('Ctrl Pts',(-0.0768084924694757,2.79143412051236E-5,
-0.0476103829072477));
#53245=CARTESIAN_POINT('Ctrl Pts',(-0.0768444791363969,0.0111170264114585,
-0.0484105563991817));
#53246=CARTESIAN_POINT('Ctrl Pts',(-0.0746012189287571,0.0221922041442296,
-0.0492107298911157));
#53247=CARTESIAN_POINT('Ctrl Pts',(-0.0700063260412132,0.0321861597049033,
-0.0500109033830497));
#53248=CARTESIAN_POINT('Ctrl Pts',(-0.0593699871226408,0.0553203439137752,
-0.0518631590639034));
#53249=CARTESIAN_POINT('Ctrl Pts',(-0.0361327054769651,0.0726609283048269,
-0.0537154147447572));
#53250=CARTESIAN_POINT('Ctrl Pts',(-0.0109280621864315,0.0762721671121984,
-0.0555676704256109));
#53251=CARTESIAN_POINT('Ctrl Pts',(0.0142765811041018,0.0798834059195699,
-0.0574199261064646));
#53252=CARTESIAN_POINT('Ctrl Pts',(0.0414485860394929,0.0697652991432615,
-0.0592721817873183));
#53253=CARTESIAN_POINT('Ctrl Pts',(0.0581527122960003,0.0505482940944206,
-0.061124437468172));
#53254=CARTESIAN_POINT('Ctrl Pts',(0.0748568385525076,0.0313312890455796,
-0.0629766931490256));
#53255=CARTESIAN_POINT('Ctrl Pts',(0.0810930861301312,0.00301538572420598,
-0.0648289488298794));
#53256=CARTESIAN_POINT('Ctrl Pts',(0.0740077005522793,-0.0214410439709651,
-0.0666812045107331));
#53257=CARTESIAN_POINT('Ctrl Pts',(0.0669223149744274,-0.0458974736661366,
-0.0685334601915868));
#53258=CARTESIAN_POINT('Ctrl Pts',(0.0465152962410998,-0.0664944297351054,
-0.0703857158724405));
#53259=CARTESIAN_POINT('Ctrl Pts',(0.0221255450337808,-0.0738059853161984,
-0.0722379715532942));
#53260=CARTESIAN_POINT('Ctrl Pts',(-0.00226420617353785,-0.0811175408972913,
-0.0740902272341478));
#53261=CARTESIAN_POINT('Ctrl Pts',(-0.0306366898548477,-0.0751436959905087,
-0.0759424829150016));
#53262=CARTESIAN_POINT('Ctrl Pts',(-0.0500075735221853,-0.0586183045583848,
-0.0777947385958553));
#53263=CARTESIAN_POINT('Ctrl Pts',(-0.066794904181321,-0.0442969542778871,
-0.0793999533663195));
#53264=CARTESIAN_POINT('Ctrl Pts',(-0.076821652061467,-0.0220509457566094,
-0.0810051681367836));
#53265=CARTESIAN_POINT('Ctrl Pts',(-0.076999203572401,5.4492118465423E-5,
-0.0826103829072478));
#53266=CARTESIAN_POINT('Ctrl Pts',(-0.0769875287350775,5.90179537171767E-5,
-0.0876396170927523));
#53267=CARTESIAN_POINT('Ctrl Pts',(-0.076803432696976,-0.0216232121982777,
-0.0860657561750835));
#53268=CARTESIAN_POINT('Ctrl Pts',(-0.0672101984381137,-0.0434480298897704,
-0.0844918952574148));
#53269=CARTESIAN_POINT('Ctrl Pts',(-0.0509902119604506,-0.0577655648933422,
-0.082918034339746));
#53270=CARTESIAN_POINT('Ctrl Pts',(-0.031901128700716,-0.0746156786794249,
-0.0810657786588923));
#53271=CARTESIAN_POINT('Ctrl Pts',(-0.00363358372165781,-0.0810677415814372,
-0.0792135229780386));
#53272=CARTESIAN_POINT('Ctrl Pts',(0.0208761571269007,-0.074169052572059,
-0.0773612672971849));
#53273=CARTESIAN_POINT('Ctrl Pts',(0.04538589797546,-0.0672703635626806,
-0.0755090116163311));
#53274=CARTESIAN_POINT('Ctrl Pts',(0.0661378346935198,-0.0470209226419106,
-0.0736567559354774));
#53275=CARTESIAN_POINT('Ctrl Pts',(0.0736351382952468,-0.0226876155441985,
-0.0718045002546237));
#53276=CARTESIAN_POINT('Ctrl Pts',(0.0811324418969736,0.00164569155351299,
-0.06995224457377));
#53277=CARTESIAN_POINT('Ctrl Pts',(0.075375112382369,0.0300628648281658,
-0.0680999888929164));
#53278=CARTESIAN_POINT('Ctrl Pts',(0.0589978879383866,0.0495591770732237,
-0.0662477332120627));
#53279=CARTESIAN_POINT('Ctrl Pts',(0.0426206634944041,0.0690554893182815,
-0.064395477531209));
#53280=CARTESIAN_POINT('Ctrl Pts',(0.0156235441210435,0.0796309405337437,
-0.0625432218503553));
#53281=CARTESIAN_POINT('Ctrl Pts',(-0.00963855596190587,0.0764458058085026,
-0.0606909661695016));
#53282=CARTESIAN_POINT('Ctrl Pts',(-0.0349006560448556,0.0732606710832615,
-0.0588387104886479));
#53283=CARTESIAN_POINT('Ctrl Pts',(-0.0584277368373945,0.0563149504173167,
-0.0569864548077942));
#53284=CARTESIAN_POINT('Ctrl Pts',(-0.0694530408221216,0.0333636478502638,
-0.0551341991269405));
#53285=CARTESIAN_POINT('Ctrl Pts',(-0.0744025960277123,0.0230601914328076,
-0.0543026717822111));
#53286=CARTESIAN_POINT('Ctrl Pts',(-0.0768326014642731,0.011546398058898,
-0.0534711444374817));
#53287=CARTESIAN_POINT('Ctrl Pts',(-0.0768041739443497,2.12084165925656E-5,
-0.0526396170927524));
#53288=CARTESIAN_POINT('Origin',(0.,0.,-0.2904));
#53289=CARTESIAN_POINT('',(-0.0769167618896329,-6.73610264414135E-5,-0.0126103829072477));
#53290=CARTESIAN_POINT('',(-0.0769126606442387,-6.94072219677582E-5,-0.0176396170927523));
#53291=CARTESIAN_POINT('',(-0.076925,-9.42059550244101E-18,-0.2904));
#53292=CARTESIAN_POINT('Ctrl Pts',(-0.0769167618896329,-6.73610264414135E-5,
-0.0126103829072477));
#53293=CARTESIAN_POINT('Ctrl Pts',(-0.0767492626789875,0.0186325472370117,
-0.0139636889807262));
#53294=CARTESIAN_POINT('Ctrl Pts',(-0.0698631593360463,0.0374386870015039,
-0.0153169950542047));
#53295=CARTESIAN_POINT('Ctrl Pts',(-0.0574675930756223,0.0513152403887189,
-0.0166703011276831));
#53296=CARTESIAN_POINT('Ctrl Pts',(-0.0405019128993307,0.0703079319504091,
-0.0185225568085369));
#53297=CARTESIAN_POINT('Ctrl Pts',(-0.0132152969986564,0.080065976703565,
-0.0203748124893906));
#53298=CARTESIAN_POINT('Ctrl Pts',(0.0119351900732871,0.0761207640746733,
-0.0222270681702443));
#53299=CARTESIAN_POINT('Ctrl Pts',(0.0370856771452302,0.0721755514457817,
-0.024079323851098));
#53300=CARTESIAN_POINT('Ctrl Pts',(0.0601000353884424,0.0545270814348429,
-0.0259315795319517));
#53301=CARTESIAN_POINT('Ctrl Pts',(0.0704302024641108,0.0312534747512865,
-0.0277838352128054));
#53302=CARTESIAN_POINT('Ctrl Pts',(0.0807603695397792,0.00797986806773009,
-0.0296360908936591));
#53303=CARTESIAN_POINT('Ctrl Pts',(0.0784063454479036,-0.0209188752884439,
-0.0314883465745128));
#53304=CARTESIAN_POINT('Ctrl Pts',(0.0644537650205357,-0.0422184446065205,
-0.0333406022553665));
#53305=CARTESIAN_POINT('Ctrl Pts',(0.0505011845931677,-0.063518013924597,
-0.0351928579362202));
#53306=CARTESIAN_POINT('Ctrl Pts',(0.0249500478303073,-0.0772184092045762,
-0.0370451136170738));
#53307=CARTESIAN_POINT('Ctrl Pts',(-0.000510915286151261,-0.0770494048566988,
-0.0388973692979275));
#53308=CARTESIAN_POINT('Ctrl Pts',(-0.0259718784026102,-0.0768804005088213,
-0.0407496249787812));
#53309=CARTESIAN_POINT('Ctrl Pts',(-0.0513426678726673,-0.0628419965330865,
-0.042601880659635));
#53310=CARTESIAN_POINT('Ctrl Pts',(-0.0650103645119611,-0.0413589025318731,
-0.0444541363404887));
#53311=CARTESIAN_POINT('Ctrl Pts',(-0.0727736233030644,-0.0291564939793202,
-0.0455062185294084));
#53312=CARTESIAN_POINT('Ctrl Pts',(-0.0767611765665022,-0.0145522453587242,
-0.0465583007183281));
#53313=CARTESIAN_POINT('Ctrl Pts',(-0.0768084924694757,2.79143412051236E-5,
-0.0476103829072477));
#53314=CARTESIAN_POINT('Ctrl Pts',(-0.0768041739443497,2.12084165925656E-5,
-0.0526396170927524));
#53315=CARTESIAN_POINT('Ctrl Pts',(-0.0767692781886113,-0.0141263571706058,
-0.051618888756628));
#53316=CARTESIAN_POINT('Ctrl Pts',(-0.073029916198227,-0.0282910951160585,
-0.0505981604205037));
#53317=CARTESIAN_POINT('Ctrl Pts',(-0.0656991356399959,-0.0402553268175926,
-0.0495774320843794));
#53318=CARTESIAN_POINT('Ctrl Pts',(-0.0523963992962273,-0.0619661144502356,
-0.0477251764035257));
#53319=CARTESIAN_POINT('Ctrl Pts',(-0.0272673994317745,-0.076430805247361,
-0.045872920722672));
#53320=CARTESIAN_POINT('Ctrl Pts',(-0.00181241292307686,-0.0770297407390354,
-0.0440206650418183));
#53321=CARTESIAN_POINT('Ctrl Pts',(0.0236425735856208,-0.0776286762307097,
-0.0421684093609646));
#53322=CARTESIAN_POINT('Ctrl Pts',(0.0494235467385634,-0.0643618564169329,
-0.0403161536801109));
#53323=CARTESIAN_POINT('Ctrl Pts',(0.0637328207573074,-0.0433008299216478,
-0.0384638979992572));
#53324=CARTESIAN_POINT('Ctrl Pts',(0.0780420947760517,-0.0222398034263625,
-0.0366116423184035));
#53325=CARTESIAN_POINT('Ctrl Pts',(0.0808796696605973,0.00661542975043124,
-0.0347593866375498));
#53326=CARTESIAN_POINT('Ctrl Pts',(0.0709457789894668,0.0300599825942979,
-0.0329071309566961));
#53327=CARTESIAN_POINT('Ctrl Pts',(0.0610118883183366,0.0535045354381642,
-0.0310548752758424));
#53328=CARTESIAN_POINT('Ctrl Pts',(0.0383065320915307,0.0715384079491035,
-0.0292026195949887));
#53329=CARTESIAN_POINT('Ctrl Pts',(0.0132227623505595,0.0759080376423198,
-0.027350363914135));
#53330=CARTESIAN_POINT('Ctrl Pts',(-0.0118610073904114,0.080277667335536,
-0.0254981082332814));
#53331=CARTESIAN_POINT('Ctrl Pts',(-0.0393231906455477,0.0709830542110295,
-0.0236458525524277));
#53332=CARTESIAN_POINT('Ctrl Pts',(-0.0566003641452171,0.052278899459558,
-0.021793596871574));
#53333=CARTESIAN_POINT('Ctrl Pts',(-0.0695159729521222,0.0382965460474998,
-0.0204089369453001));
#53334=CARTESIAN_POINT('Ctrl Pts',(-0.0767398316412204,0.0190558020251586,
-0.0190242770190262));
#53335=CARTESIAN_POINT('Ctrl Pts',(-0.0769126606442387,-6.94072219677582E-5,
-0.0176396170927523));
#53336=CARTESIAN_POINT('Origin',(0.,0.,-0.648563377523455));
#53337=CARTESIAN_POINT('',(-0.0569189037447819,-4.98475974056255E-5,-0.00106337752345494));
#53338=CARTESIAN_POINT('',(-0.056925,-6.31153998696879E-15,0.));
#53339=CARTESIAN_POINT('',(-0.056925,-6.31153998696879E-15,-0.648563377523455));
#53340=CARTESIAN_POINT('',(-0.0558909241998548,-0.0108009359356534,0.));
#53341=CARTESIAN_POINT('Ctrl Pts',(-0.0569189037447819,-4.98475974056176E-5,
-0.00106337752345494));
#53342=CARTESIAN_POINT('Ctrl Pts',(-0.056951368975225,-0.00367432337077014,
-0.000708918348970012));
#53343=CARTESIAN_POINT('Ctrl Pts',(-0.0566427552153233,-0.00729340615886513,
-0.000354459174485079));
#53344=CARTESIAN_POINT('Ctrl Pts',(-0.0559769847942903,-0.010840135857283,
-1.4644860844848E-16));
#53345=CARTESIAN_POINT('Origin',(0.,0.,0.));
#53346=CARTESIAN_POINT('Origin',(0.,0.,-0.648563377523455));
#53347=CARTESIAN_POINT('',(-0.056838783670132,2.06567939264175E-5,-0.0360633775234549));
#53348=CARTESIAN_POINT('',(-0.0569158687965329,-5.13617954007034E-5,-0.0291866224765442));
#53349=CARTESIAN_POINT('',(-0.056925,-6.31153998696879E-15,-0.648563377523455));
#53350=CARTESIAN_POINT('Ctrl Pts',(-0.056838783670132,2.06567939264176E-5,
-0.0360633775234549));
#53351=CARTESIAN_POINT('Ctrl Pts',(-0.0568037695943851,-0.0107687561526893,
-0.0350112953345353));
#53352=CARTESIAN_POINT('Ctrl Pts',(-0.0486578615942883,-0.0406028067131398,
-0.032106957464762));
#53353=CARTESIAN_POINT('Ctrl Pts',(-0.000444809717068389,-0.0672805062760264,
-0.0273503639141349));
#53354=CARTESIAN_POINT('Ctrl Pts',(0.0562792121311924,-0.036865361603442,
-0.021793596871574));
#53355=CARTESIAN_POINT('Ctrl Pts',(0.0615051915174765,0.0272904121586725,
-0.0162368298290127));
#53356=CARTESIAN_POINT('Ctrl Pts',(0.0104128674487777,0.0664703597195168,
-0.0106800627864517));
#53357=CARTESIAN_POINT('Ctrl Pts',(-0.0447246776124606,0.046752464534374,
-0.00562224535126571));
#53358=CARTESIAN_POINT('Ctrl Pts',(-0.0567949532401875,0.0137882060639156,
-0.0024166835969335));
#53359=CARTESIAN_POINT('Ctrl Pts',(-0.0569189037447819,-4.98475974056176E-5,
-0.00106337752345494));
#53360=CARTESIAN_POINT('',(-0.0286389268003753,0.0491962142519396,0.));
#53361=CARTESIAN_POINT('Origin',(0.,0.,0.));
#53362=CARTESIAN_POINT('Ctrl Pts',(-0.0569158687965329,-5.13617954006995E-5,
-0.0291866224765442));
#53363=CARTESIAN_POINT('Ctrl Pts',(-0.0569590584376293,-0.00483071542741229,
-0.0287190267219646));
#53364=CARTESIAN_POINT('Ctrl Pts',(-0.0542212221178314,-0.0284938299898704,
-0.0263991752865313));
#53365=CARTESIAN_POINT('Ctrl Pts',(-0.0212425420460525,-0.0638395728638739,
-0.0222270681702444));
#53366=CARTESIAN_POINT('Ctrl Pts',(0.0420792312090032,-0.0524733655289061,
-0.0166703011276832));
#53367=CARTESIAN_POINT('Ctrl Pts',(0.0669727390520183,0.00689708027414815,
-0.0111135340851222));
#53368=CARTESIAN_POINT('Ctrl Pts',(0.0303982238704425,0.0600019556186538,
-0.00555676704256101));
#53369=CARTESIAN_POINT('Ctrl Pts',(-0.012280390439628,0.0587191202828289,
-0.00185225568085369));
#53370=CARTESIAN_POINT('Ctrl Pts',(-0.0286389268003753,0.0491962142519396,
0.));
#53371=CARTESIAN_POINT('Origin',(0.,0.,-0.648563377523455));
#53372=CARTESIAN_POINT('',(-0.0569799111258879,4.03245218502727E-5,-0.0710633775234549));
#53373=CARTESIAN_POINT('',(-0.056835587933469,1.56943661208178E-5,-0.0641866224765442));
#53374=CARTESIAN_POINT('',(-0.056925,-6.31153998696879E-15,-0.648563377523455));
#53375=CARTESIAN_POINT('Ctrl Pts',(-0.0569799111258879,4.03245218502722E-5,
-0.0710633775234549));
#53376=CARTESIAN_POINT('Ctrl Pts',(-0.0568485218537396,-0.0163178431874584,
-0.0694581627529908));
#53377=CARTESIAN_POINT('Ctrl Pts',(-0.0408668960010946,-0.0517757393220317,
-0.0660006923016731));
#53378=CARTESIAN_POINT('Ctrl Pts',(0.0193202950553148,-0.0644481915748698,
-0.0606909661695014));
#53379=CARTESIAN_POINT('Ctrl Pts',(0.0646242745702175,-0.0187225474711557,
-0.0551341991269405));
#53380=CARTESIAN_POINT('Ctrl Pts',(0.0507796833441037,0.0441393100486048,
-0.0495774320843793));
#53381=CARTESIAN_POINT('Ctrl Pts',(-0.00954269745331579,0.0666017043901573,
-0.0440206650418183));
#53382=CARTESIAN_POINT('Ctrl Pts',(-0.0513627268784663,0.0353939340261016,
-0.0395159801881768));
#53383=CARTESIAN_POINT('Ctrl Pts',(-0.0568654140375617,0.00822667180334124,
-0.036863551015389));
#53384=CARTESIAN_POINT('Ctrl Pts',(-0.056838783670132,2.06567939264176E-5,
-0.0360633775234549));
#53385=CARTESIAN_POINT('Ctrl Pts',(-0.056835587933469,1.56943661208178E-5,
-0.0641866224765442));
#53386=CARTESIAN_POINT('Ctrl Pts',(-0.0568097648474042,-0.0104535961252809,
-0.0631658941404201));
#53387=CARTESIAN_POINT('Ctrl Pts',(-0.0490212243523883,-0.0399566598492793,
-0.0602929101234423));
#53388=CARTESIAN_POINT('Ctrl Pts',(-0.00158242957906591,-0.0672632578788742,
-0.055567670425611));
#53389=CARTESIAN_POINT('Ctrl Pts',(0.0556518335368746,-0.0378106591957688,
-0.0500109033830497));
#53390=CARTESIAN_POINT('Ctrl Pts',(0.0619513051118907,0.0262485211196931,
-0.0444541363404888));
#53391=CARTESIAN_POINT('Ctrl Pts',(0.0115449715450025,0.0662840697456999,
-0.0388973692979276));
#53392=CARTESIAN_POINT('Ctrl Pts',(-0.0442913408145573,0.0473861941886207,
-0.0338081980099462));
#53393=CARTESIAN_POINT('Ctrl Pts',(-0.0567879742109411,0.0141014173582273,
-0.0305712824028183));
#53394=CARTESIAN_POINT('Ctrl Pts',(-0.0569158687965329,-5.13617954006995E-5,
-0.0291866224765442));
#53395=CARTESIAN_POINT('Origin',(0.,0.,-0.648563377523455));
#53396=CARTESIAN_POINT('',(-0.056963270929731,-4.61853323570465E-5,-0.106063377523455));
#53397=CARTESIAN_POINT('',(-0.0569712716703839,4.36736693513254E-5,-0.0991866224765444));
#53398=CARTESIAN_POINT('',(-0.056925,-6.31153998696879E-15,-0.648563377523455));
#53399=CARTESIAN_POINT('Ctrl Pts',(-0.056963270929731,-4.61853323570488E-5,
-0.106063377523455));
#53400=CARTESIAN_POINT('Ctrl Pts',(-0.0569907444490709,-0.00316782709076371,
-0.1057572858523));
#53401=CARTESIAN_POINT('Ctrl Pts',(-0.0553373033443182,-0.0251503644672759,
-0.103598938500292));
#53402=CARTESIAN_POINT('Ctrl Pts',(-0.0267203606150653,-0.061748388075023,
-0.0995883354674292));
#53403=CARTESIAN_POINT('Ctrl Pts',(0.0373853828786833,-0.055939023097401,
-0.0940315684248681));
#53404=CARTESIAN_POINT('Ctrl Pts',(0.0672732959960052,0.00106981324138322,
-0.088474801382307));
#53405=CARTESIAN_POINT('Ctrl Pts',(0.035587791331269,0.0570994779548752,
-0.0829180343397459));
#53406=CARTESIAN_POINT('Ctrl Pts',(-0.0286702650266008,0.0608675398312384,
-0.0773612672971849));
#53407=CARTESIAN_POINT('Ctrl Pts',(-0.0557050211889429,0.0239300714199293,
-0.0734097150250878));
#53408=CARTESIAN_POINT('Ctrl Pts',(-0.0570001318004071,0.00255782979128222,
-0.0713104184338445));
#53409=CARTESIAN_POINT('Ctrl Pts',(-0.0569799111258879,4.03245218502722E-5,
-0.0710633775234549));
#53410=CARTESIAN_POINT('Ctrl Pts',(-0.0569712716703839,4.36736693513245E-5,
-0.0991866224765444));
#53411=CARTESIAN_POINT('Ctrl Pts',(-0.0568350394055926,-0.016001317574096,
-0.0976127615588758));
#53412=CARTESIAN_POINT('Ctrl Pts',(-0.0413812008133835,-0.0511591382639303,
-0.0941866449603535));
#53413=CARTESIAN_POINT('Ctrl Pts',(0.0182292914472235,-0.0647652241822597,
-0.0889082726809775));
#53414=CARTESIAN_POINT('Ctrl Pts',(0.0642989956139634,-0.0198110704839244,
-0.0833515056384163));
#53415=CARTESIAN_POINT('Ctrl Pts',(0.0515176118264206,0.0432756083068328,
-0.0777947385958553));
#53416=CARTESIAN_POINT('Ctrl Pts',(-0.00841651961310768,0.0667533162213003,
-0.0722379715532942));
#53417=CARTESIAN_POINT('Ctrl Pts',(-0.0510528083444251,0.0360439117930788,
-0.0677019328468572));
#53418=CARTESIAN_POINT('Ctrl Pts',(-0.0568566244829879,0.00854440961328914,
-0.0650181498212739));
#53419=CARTESIAN_POINT('Ctrl Pts',(-0.056835587933469,1.56943661208178E-5,
-0.0641866224765442));
#53420=CARTESIAN_POINT('Origin',(0.,0.,-0.648563377523455));
#53421=CARTESIAN_POINT('',(-0.056833565091417,-1.11797377874599E-5,-0.141063377523455));
#53422=CARTESIAN_POINT('',(-0.0569723044751072,-4.33103373571816E-5,-0.134186622476544));
#53423=CARTESIAN_POINT('',(-0.056925,-6.31153998696879E-15,-0.648563377523455));
#53424=CARTESIAN_POINT('Ctrl Pts',(-0.056833565091417,-1.11797377874701E-5,
-0.141063377523455));
#53425=CARTESIAN_POINT('Ctrl Pts',(-0.0568490362920882,-0.00882475260196868,
-0.140204153270756));
#53426=CARTESIAN_POINT('Ctrl Pts',(-0.0507726628702476,-0.0366178082310402,
-0.137492673337203));
#53427=CARTESIAN_POINT('Ctrl Pts',(-0.00741986034787437,-0.0668714195615047,
-0.132928937722796));
#53428=CARTESIAN_POINT('Ctrl Pts',(0.0521573533537793,-0.0425023714047127,
-0.127372170680235));
#53429=CARTESIAN_POINT('Ctrl Pts',(0.0639963557059561,0.0207679448567898,
-0.121815403637674));
#53430=CARTESIAN_POINT('Ctrl Pts',(0.0172612290645072,0.0650299242997547,
-0.116258636595113));
#53431=CARTESIAN_POINT('Ctrl Pts',(-0.0418279869431582,0.0506122645593998,
-0.111007961223706));
#53432=CARTESIAN_POINT('Ctrl Pts',(-0.0568244936586512,0.0157221958189843,
-0.107609541533154));
#53433=CARTESIAN_POINT('Ctrl Pts',(-0.056963270929731,-4.61853323570488E-5,
-0.106063377523455));
#53434=CARTESIAN_POINT('Ctrl Pts',(-0.0569723044751072,-4.33103373571769E-5,
-0.134186622476544));
#53435=CARTESIAN_POINT('Ctrl Pts',(-0.0569959514374928,-0.00284403943605085,
-0.133911884658185));
#53436=CARTESIAN_POINT('Ctrl Pts',(-0.0555352225271942,-0.024502253767729,
-0.131784891158972));
#53437=CARTESIAN_POINT('Ctrl Pts',(-0.0277591773719423,-0.0612884082229279,
-0.127805641978905));
#53438=CARTESIAN_POINT('Ctrl Pts',(0.0364355162536436,-0.0565623026212381,
-0.122248874936344));
#53439=CARTESIAN_POINT('Ctrl Pts',(0.0672817693522171,-6.62549929698068E-5,
-0.116692107893783));
#53440=CARTESIAN_POINT('Ctrl Pts',(0.0365468441487368,0.0564904338066607,
-0.111135340851222));
#53441=CARTESIAN_POINT('Ctrl Pts',(-0.0276384181430455,0.0613429607075467,
-0.105578573808661));
#53442=CARTESIAN_POINT('Ctrl Pts',(-0.0555124500581288,0.0245778251385385,
-0.101595667683768));
#53443=CARTESIAN_POINT('Ctrl Pts',(-0.0569953693200993,0.00288181615537408,
-0.0994650172397295));
#53444=CARTESIAN_POINT('Ctrl Pts',(-0.0569712716703839,4.36736693513245E-5,
-0.0991866224765444));
#53445=CARTESIAN_POINT('Origin',(0.,0.,-0.648563377523455));
#53446=CARTESIAN_POINT('',(-0.0569222642333711,5.20379574683919E-5,-0.176063377523455));
#53447=CARTESIAN_POINT('',(-0.0568358797642761,-1.62751836963598E-5,-0.169186622476544));
#53448=CARTESIAN_POINT('',(-0.056925,-6.31153998696879E-15,-0.648563377523455));
#53449=CARTESIAN_POINT('Ctrl Pts',(-0.0569222642333711,5.20379574683923E-5,
-0.176063377523455));
#53450=CARTESIAN_POINT('Ctrl Pts',(-0.0567901789907606,-0.0143784386554175,
-0.174651020689211));
#53451=CARTESIAN_POINT('Ctrl Pts',(-0.0438880872324678,-0.0479441447327426,
-0.171386408174114));
#53452=CARTESIAN_POINT('Ctrl Pts',(0.0125342308929026,-0.066103964613694,
-0.166269539978162));
#53453=CARTESIAN_POINT('Ctrl Pts',(0.0623349526476669,-0.0253218237929275,
-0.160712772935602));
#53454=CARTESIAN_POINT('Ctrl Pts',(0.0550821824500234,0.0386366957463386,
-0.15515600589304));
#53455=CARTESIAN_POINT('Ctrl Pts',(-0.00258581579222903,0.0672320952997525,
-0.149599238850479));
#53456=CARTESIAN_POINT('Ctrl Pts',(-0.0493360368562338,0.0393852313480028,
-0.144901696060617));
#53457=CARTESIAN_POINT('Ctrl Pts',(-0.0568156845573776,0.0101749327013848,
-0.142056408951609));
#53458=CARTESIAN_POINT('Ctrl Pts',(-0.056833565091417,-1.11797377874701E-5,
-0.141063377523455));
#53459=CARTESIAN_POINT('Ctrl Pts',(-0.0568358797642761,-1.62751836963529E-5,
-0.169186622476544));
#53460=CARTESIAN_POINT('Ctrl Pts',(-0.0568576303807177,-0.00850736920572494,
-0.168358752076641));
#53461=CARTESIAN_POINT('Ctrl Pts',(-0.0510894273931871,-0.035968134601679,
-0.165678625995883));
#53462=CARTESIAN_POINT('Ctrl Pts',(-0.00854793224978894,-0.0667365998802494,
-0.161146244234271));
#53463=CARTESIAN_POINT('Ctrl Pts',(0.0514322603095934,-0.0433769928549986,
-0.155589477191711));
#53464=CARTESIAN_POINT('Ctrl Pts',(0.0643378995797782,0.019684399569185,
-0.150032710149149));
#53465=CARTESIAN_POINT('Ctrl Pts',(0.0183568039000239,0.0647291948037812,
-0.144475943106589));
#53466=CARTESIAN_POINT('Ctrl Pts',(-0.0413216787244819,0.0512311939704846,
-0.139193913882386));
#53467=CARTESIAN_POINT('Ctrl Pts',(-0.0568365259143696,0.0160382040590988,
-0.135764140339039));
#53468=CARTESIAN_POINT('Ctrl Pts',(-0.0569723044751072,-4.33103373571769E-5,
-0.134186622476544));
#53469=CARTESIAN_POINT('Origin',(0.,0.,-0.648563377523455));
#53470=CARTESIAN_POINT('',(-0.0570089748886303,-2.08118398348977E-5,-0.211063377523455));
#53471=CARTESIAN_POINT('',(-0.0569126591974534,5.18768886537315E-5,-0.204186622476544));
#53472=CARTESIAN_POINT('',(-0.056925,-6.31153998696879E-15,-0.648563377523455));
#53473=CARTESIAN_POINT('Ctrl Pts',(-0.0570089748886303,-2.08118398349025E-5,
-0.211063377523455));
#53474=CARTESIAN_POINT('Ctrl Pts',(-0.057014394399661,-0.00117318814847394,
-0.210950143788521));
#53475=CARTESIAN_POINT('Ctrl Pts',(-0.0564604142361575,-0.0211706048259219,
-0.208984654372732));
#53476=CARTESIAN_POINT('Ctrl Pts',(-0.0329783512134566,-0.0586452848315629,
-0.20516690927609));
#53477=CARTESIAN_POINT('Ctrl Pts',(0.0313842223908242,-0.059513625890684,
-0.199610142233529));
#53478=CARTESIAN_POINT('Ctrl Pts',(0.0670216682215793,-0.00591075887945832,
-0.194053375190967));
#53479=CARTESIAN_POINT('Ctrl Pts',(0.0413159984164774,0.0531020654643655,
-0.188496608148407));
#53480=CARTESIAN_POINT('Ctrl Pts',(-0.0222050844590437,0.0635120091470762,
-0.182939841105846));
#53481=CARTESIAN_POINT('Ctrl Pts',(-0.0544230314477119,0.0279202910097429,
-0.178795430897528));
#53482=CARTESIAN_POINT('Ctrl Pts',(-0.0569634040816515,0.00454661741793302,
-0.176503276370065));
#53483=CARTESIAN_POINT('Ctrl Pts',(-0.0569222642333711,5.20379574683923E-5,
-0.176063377523455));
#53484=CARTESIAN_POINT('Ctrl Pts',(-0.0569126591974534,5.18768886537324E-5,
-0.204186622476544));
#53485=CARTESIAN_POINT('Ctrl Pts',(-0.0567857930323549,-0.0140643235191736,
-0.202805619495096));
#53486=CARTESIAN_POINT('Ctrl Pts',(-0.0443475684573707,-0.0473133514809718,
-0.199572360832794));
#53487=CARTESIAN_POINT('Ctrl Pts',(0.0114162724268508,-0.0663061809579219,
-0.194486846489638));
#53488=CARTESIAN_POINT('Ctrl Pts',(0.0618985035444009,-0.0263707445538147,
-0.188930079447077));
#53489=CARTESIAN_POINT('Ctrl Pts',(0.0557267127407225,0.0377011192997421,
-0.183373312404516));
#53490=CARTESIAN_POINT('Ctrl Pts',(-0.00145022720861101,0.067266170921093,
-0.177816545361955));
#53491=CARTESIAN_POINT('Ctrl Pts',(-0.048979108510772,0.040032089808678,
-0.173087648719298));
#53492=CARTESIAN_POINT('Ctrl Pts',(-0.0568089661177235,0.0104903835111149,
-0.170211007757494));
#53493=CARTESIAN_POINT('Ctrl Pts',(-0.0568358797642761,-1.62751836963529E-5,
-0.169186622476544));
#53494=CARTESIAN_POINT('Origin',(0.,0.,-0.648563377523455));
#53495=CARTESIAN_POINT('',(-0.0568606839966886,-3.88794714720325E-5,-0.246063377523455));
#53496=CARTESIAN_POINT('',(-0.057013254179569,-1.52882767560647E-5,-0.239186622476545));
#53497=CARTESIAN_POINT('',(-0.056925,-6.31153998696879E-15,-0.648563377523455));
#53498=CARTESIAN_POINT('Ctrl Pts',(-0.0568606839966886,-3.8879471472038E-5,
-0.246063377523455));
#53499=CARTESIAN_POINT('Ctrl Pts',(-0.0569036124203374,-0.00686603560376843,
-0.245397011206976));
#53500=CARTESIAN_POINT('Ctrl Pts',(-0.0526059144902416,-0.0326179607792761,
-0.242878389209643));
#53501=CARTESIAN_POINT('Ctrl Pts',(-0.0143130139311376,-0.0657417577643039,
-0.238507511531456));
#53502=CARTESIAN_POINT('Ctrl Pts',(0.0474696795615072,-0.0476809249497236,
-0.232950744488896));
#53503=CARTESIAN_POINT('Ctrl Pts',(0.0658046624882197,0.0140209656067212,
-0.227393977446334));
#53504=CARTESIAN_POINT('Ctrl Pts',(0.0239104221278329,0.0628898465207396,
-0.221837210403774));
#53505=CARTESIAN_POINT('Ctrl Pts',(-0.0385687185501853,0.0543744885075883,
-0.216393677096147));
#53506=CARTESIAN_POINT('Ctrl Pts',(-0.0569257430794525,0.0176771621061551,
-0.212802399469374));
#53507=CARTESIAN_POINT('Ctrl Pts',(-0.0570089748886303,-2.08118398349025E-5,
-0.211063377523455));
#53508=CARTESIAN_POINT('Ctrl Pts',(-0.0570132541795689,-1.52882767560661E-5,
-0.239186622476545));
#53509=CARTESIAN_POINT('Ctrl Pts',(-0.0570162374249387,-0.000848410610404804,
-0.239104742594405));
#53510=CARTESIAN_POINT('Ctrl Pts',(-0.0566222054253004,-0.020525226487873,
-0.237170607031412));
#53511=CARTESIAN_POINT('Ctrl Pts',(-0.0339638799205846,-0.0580800806653254,
-0.233384215787566));
#53512=CARTESIAN_POINT('Ctrl Pts',(0.0303748547031255,-0.0600350656792724,
-0.227827448745005));
#53513=CARTESIAN_POINT('Ctrl Pts',(0.066912308428919,-0.00704158292317649,
-0.222270681702444));
#53514=CARTESIAN_POINT('Ctrl Pts',(0.0422067405718221,0.0523968697505238,
-0.216713914659883));
#53515=CARTESIAN_POINT('Ctrl Pts',(-0.0211295124981265,0.0638778882786663,
-0.211157147617322));
#53516=CARTESIAN_POINT('Ctrl Pts',(-0.0541920864480305,0.0285701384591516,
-0.206981383556209));
#53517=CARTESIAN_POINT('Ctrl Pts',(-0.0569559509379992,0.00486888136793312,
-0.20465787517595));
#53518=CARTESIAN_POINT('Ctrl Pts',(-0.0569126591974534,5.18768886537324E-5,
-0.204186622476544));
#53519=CARTESIAN_POINT('Origin',(0.,0.,-0.648563377523455));
#53520=CARTESIAN_POINT('',(-0.0568682500885786,4.24477755887524E-5,-0.281063377523455));
#53521=CARTESIAN_POINT('',(-0.056867718939529,-4.22236051248123E-5,-0.274186622476545));
#53522=CARTESIAN_POINT('',(-0.056925,-6.31153998696879E-15,-0.648563377523455));
#53523=CARTESIAN_POINT('Ctrl Pts',(-0.0568682500885786,4.24477755887522E-5,
-0.281063377523455));
#53524=CARTESIAN_POINT('Ctrl Pts',(-0.0567817400057179,-0.012447566283586,
-0.279843878625431));
#53525=CARTESIAN_POINT('Ctrl Pts',(-0.0465781847879718,-0.0440367559175842,
-0.276772124046554));
#53526=CARTESIAN_POINT('Ctrl Pts',(0.0056131103110498,-0.0670472525489997,
-0.271848113786823));
#53527=CARTESIAN_POINT('Ctrl Pts',(0.0593736866708568,-0.0316481660265529,
-0.266291346744262));
#53528=CARTESIAN_POINT('Ctrl Pts',(0.0587911375337822,0.0327176287224069,
-0.2607345797017));
#53529=CARTESIAN_POINT('Ctrl Pts',(0.00439865432921479,0.0671378650377374,
-0.25517781265914));
#53530=CARTESIAN_POINT('Ctrl Pts',(-0.0470142696024862,0.0433499735423753,
-0.250287411933058));
#53531=CARTESIAN_POINT('Ctrl Pts',(-0.0567842870363749,0.0121109721131533,
-0.24724926688783));
#53532=CARTESIAN_POINT('Ctrl Pts',(-0.0568606839966886,-3.8879471472038E-5,
-0.246063377523455));
#53533=CARTESIAN_POINT('Ctrl Pts',(-0.056867718939529,-4.22236051248167E-5,
-0.274186622476545));
#53534=CARTESIAN_POINT('Ctrl Pts',(-0.0569125008838839,-0.00654612492033858,
-0.273551610012861));
#53535=CARTESIAN_POINT('Ctrl Pts',(-0.0528785336578182,-0.031967267484468,
-0.271064341868323));
#53536=CARTESIAN_POINT('Ctrl Pts',(-0.0154210285602653,-0.0654907076423372,
-0.266724818042933));
#53537=CARTESIAN_POINT('Ctrl Pts',(0.0466578145771441,-0.0484756562434736,
-0.261168051000371));
#53538=CARTESIAN_POINT('Ctrl Pts',(0.0660320251551521,0.0129078489013458,
-0.255611283957811));
#53539=CARTESIAN_POINT('Ctrl Pts',(0.024968913561939,0.062477149942095,
-0.250054516915249));
#53540=CARTESIAN_POINT('Ctrl Pts',(-0.0380057476550708,0.0549750082677155,
-0.244579629754827));
#53541=CARTESIAN_POINT('Ctrl Pts',(-0.0569487515781217,0.0179981672672241,
-0.240956998275259));
#53542=CARTESIAN_POINT('Ctrl Pts',(-0.0570132541795689,-1.52882767560661E-5,
-0.239186622476545));
#53543=CARTESIAN_POINT('Origin',(0.,0.,-0.648563377523455));
#53544=CARTESIAN_POINT('',(-0.0570135171869611,1.48812492774907E-5,-0.316063377523455));
#53545=CARTESIAN_POINT('',(-0.0568611677903335,3.91338492306513E-5,-0.309186622476545));
#53546=CARTESIAN_POINT('',(-0.056925,-6.31153998696879E-15,-0.648563377523455));
#53547=CARTESIAN_POINT('Ctrl Pts',(-0.0570135171869611,1.48812492774924E-5,
-0.316063377523455));
#53548=CARTESIAN_POINT('Ctrl Pts',(-0.0569504835385972,-0.018021304605307,
-0.314290746043887));
#53549=CARTESIAN_POINT('Ctrl Pts',(-0.0379648854061764,-0.0550180793549962,
-0.310665858883465));
#53550=CARTESIAN_POINT('Ctrl Pts',(0.0250447938771848,-0.0624467723856301,
-0.30518871604219));
#53551=CARTESIAN_POINT('Ctrl Pts',(0.0660476583541301,-0.0128276228378236,
-0.299631948999629));
#53552=CARTESIAN_POINT('Ctrl Pts',(0.0465988920167232,0.0485323020734347,
-0.294075181957067));
#53553=CARTESIAN_POINT('Ctrl Pts',(-0.0155005766582128,0.0654719268465212,
-0.288518414914507));
#53554=CARTESIAN_POINT('Ctrl Pts',(-0.0528978808086814,0.0319204558933633,
-0.284181146769969));
#53555=CARTESIAN_POINT('Ctrl Pts',(-0.0569131372482161,0.00652309415123876,
-0.281696134306285));
#53556=CARTESIAN_POINT('Ctrl Pts',(-0.0568682500885786,4.24477755887522E-5,
-0.281063377523455));
#53557=CARTESIAN_POINT('Ctrl Pts',(-0.0568611677903335,3.91338492306548E-5,
-0.309186622476545));
#53558=CARTESIAN_POINT('Ctrl Pts',(-0.0567840831424961,-0.0121335669947618,
-0.307998477431316));
#53559=CARTESIAN_POINT('Ctrl Pts',(-0.0469852991097598,-0.043396111163104,
-0.304958076705234));
#53560=CARTESIAN_POINT('Ctrl Pts',(0.00448021117374274,-0.0671324706620369,
-0.300065420298299));
#53561=CARTESIAN_POINT('Ctrl Pts',(0.0588308389422806,-0.0326461835242353,
-0.294508653255737));
#53562=CARTESIAN_POINT('Ctrl Pts',(0.0593351950206278,0.0317202701945406,
-0.288951886213177));
#53563=CARTESIAN_POINT('Ctrl Pts',(0.00553165596584969,0.067054020696943,
-0.283395119170615));
#53564=CARTESIAN_POINT('Ctrl Pts',(-0.0466077501799208,0.04399070875264,
-0.278473364591738));
#53565=CARTESIAN_POINT('Ctrl Pts',(-0.056781877288955,0.0124249801331489,
-0.275403865693715));
#53566=CARTESIAN_POINT('Ctrl Pts',(-0.056867718939529,-4.22236051248167E-5,
-0.274186622476545));
#53567=CARTESIAN_POINT('Origin',(0.,0.,-0.648563377523455));
#53568=CARTESIAN_POINT('',(-0.0569119761389687,-5.18431700991948E-5,-0.351063377523455));
#53569=CARTESIAN_POINT('',(-0.0570093201057945,2.04236075452674E-5,-0.344186622476545));
#53570=CARTESIAN_POINT('',(-0.056925,-6.31153998696879E-15,-0.648563377523455));
#53571=CARTESIAN_POINT('Ctrl Pts',(-0.0569119761389687,-5.18431700991979E-5,
-0.351063377523455));
#53572=CARTESIAN_POINT('Ctrl Pts',(-0.0569554027342431,-0.00489205285501732,
-0.350589869143196));
#53573=CARTESIAN_POINT('Ctrl Pts',(-0.0541752230501154,-0.0286169003842717,
-0.348264105082084));
#53574=CARTESIAN_POINT('Ctrl Pts',(-0.0210518974052001,-0.0639035108376226,
-0.344086085340117));
#53575=CARTESIAN_POINT('Ctrl Pts',(0.0422703628063335,-0.0523455586459296,
-0.338529318297556));
#53576=CARTESIAN_POINT('Ctrl Pts',(0.0669037060988672,0.00712286402858384,
-0.332972551254995));
#53577=CARTESIAN_POINT('Ctrl Pts',(0.0303019012879613,0.0600719223936441,
-0.327415784212435));
#53578=CARTESIAN_POINT('Ctrl Pts',(-0.0340344121380907,0.0580387790373639,
-0.321859017169872));
#53579=CARTESIAN_POINT('Ctrl Pts',(-0.0566336279638654,0.020478815225617,
-0.31807488160688));
#53580=CARTESIAN_POINT('Ctrl Pts',(-0.0570163485729333,0.000825042249724007,
-0.316143001724741));
#53581=CARTESIAN_POINT('Ctrl Pts',(-0.0570135171869611,1.48812492774924E-5,
-0.316063377523455));
#53582=CARTESIAN_POINT('Ctrl Pts',(-0.0570093201057945,2.04236075452674E-5,
-0.344186622476545));
#53583=CARTESIAN_POINT('Ctrl Pts',(-0.0569273325535133,-0.0177002196552895,
-0.342445344849772));
#53584=CARTESIAN_POINT('Ctrl Pts',(-0.0385285285934815,-0.0544178041351661,
-0.338851811542146));
#53585=CARTESIAN_POINT('Ctrl Pts',(0.0239868036411113,-0.0628607521465771,
-0.333406022553666));
#53586=CARTESIAN_POINT('Ctrl Pts',(0.0658216455765284,-0.0139410144160481,
-0.327849255511104));
#53587=CARTESIAN_POINT('Ctrl Pts',(0.0474117200646131,0.0477385557999543,
-0.322292488468544));
#53588=CARTESIAN_POINT('Ctrl Pts',(-0.0143928672572947,0.0657243203195322,
-0.316735721425982));
#53589=CARTESIAN_POINT('Ctrl Pts',(-0.0526257584487598,0.032571147773634,
-0.31236709942865));
#53590=CARTESIAN_POINT('Ctrl Pts',(-0.056904254057181,0.00684303386737312,
-0.30985073311217));
#53591=CARTESIAN_POINT('Ctrl Pts',(-0.0568611677903335,3.91338492306548E-5,
-0.309186622476545));
#53592=CARTESIAN_POINT('Origin',(0.,0.,-0.648563377523455));
#53593=CARTESIAN_POINT('',(-0.0568360806176596,1.66360965570816E-5,-0.386063377523455));
#53594=CARTESIAN_POINT('',(-0.0569215673661572,-5.20456487798915E-5,-0.379186622476545));
#53595=CARTESIAN_POINT('',(-0.056925,-6.31153998696879E-15,-0.648563377523455));
#53596=CARTESIAN_POINT('Ctrl Pts',(-0.0568360806176596,1.66360965570813E-5,
-0.386063377523455));
#53597=CARTESIAN_POINT('Ctrl Pts',(-0.0568085040742901,-0.0105130658937851,
-0.385036736561652));
#53598=CARTESIAN_POINT('Ctrl Pts',(-0.0489531286766632,-0.0400785985646141,
-0.382157839918994));
#53599=CARTESIAN_POINT('Ctrl Pts',(-0.00136851012122178,-0.0672678843265587,
-0.377426687595484));
#53600=CARTESIAN_POINT('Ctrl Pts',(0.0557724726184293,-0.0376333944757582,
-0.371869920552923));
#53601=CARTESIAN_POINT('Ctrl Pts',(0.0618664234365842,0.0264459209122466,
-0.366313153510362));
#53602=CARTESIAN_POINT('Ctrl Pts',(0.0113357143866367,0.0663200019683107,
-0.360756386467801));
#53603=CARTESIAN_POINT('Ctrl Pts',(-0.0443802898012825,0.0472678976323277,
-0.355673127805499));
#53604=CARTESIAN_POINT('Ctrl Pts',(-0.056785527899603,0.0140417321827706,
-0.35244212482405));
#53605=CARTESIAN_POINT('Ctrl Pts',(-0.0569119761389687,-5.18431700991979E-5,
-0.351063377523455));
#53606=CARTESIAN_POINT('Ctrl Pts',(-0.0569215673661572,-5.2045648779895E-5,
-0.379186622476545));
#53607=CARTESIAN_POINT('Ctrl Pts',(-0.0569628786480138,-0.00456981308281385,
-0.378744467949081));
#53608=CARTESIAN_POINT('Ctrl Pts',(-0.0544066310307784,-0.0279670336518439,
-0.376450057740764));
#53609=CARTESIAN_POINT('Ctrl Pts',(-0.0221279122263006,-0.0635389361718822,
-0.372303391851593));
#53610=CARTESIAN_POINT('Ctrl Pts',(0.0413804763988367,-0.0530518339207716,
-0.366746624809032));
#53611=CARTESIAN_POINT('Ctrl Pts',(0.0670144370045379,0.00599217342164428,
-0.361189857766471));
#53612=CARTESIAN_POINT('Ctrl Pts',(0.031311900511308,0.0595517069085378,
-0.35563309072391));
#53613=CARTESIAN_POINT('Ctrl Pts',(-0.0330495695001504,0.0586051778020126,
-0.350076323681349));
#53614=CARTESIAN_POINT('Ctrl Pts',(-0.0564722426354389,0.0211241581890796,
-0.34626083426556));
#53615=CARTESIAN_POINT('Ctrl Pts',(-0.0570145454752997,0.00114982564897547,
-0.344297600530626));
#53616=CARTESIAN_POINT('Ctrl Pts',(-0.0570093201057945,2.04236075452674E-5,
-0.344186622476545));
#53617=CARTESIAN_POINT('Origin',(0.,0.,-0.648563377523455));
#53618=CARTESIAN_POINT('',(-0.0569729394550437,4.30825583782282E-5,-0.421063377523455));
#53619=CARTESIAN_POINT('',(-0.0568337016952294,1.15506553720647E-5,-0.414186622476544));
#53620=CARTESIAN_POINT('',(-0.056925,-6.31153998696879E-15,-0.648563377523455));
#53621=CARTESIAN_POINT('Ctrl Pts',(-0.0569729394550437,4.30825583782333E-5,
-0.421063377523455));
#53622=CARTESIAN_POINT('Ctrl Pts',(-0.0568374552814163,-0.0160609606593731,
-0.419483603980107));
#53623=CARTESIAN_POINT('Ctrl Pts',(-0.0412849050737077,-0.0512756220641729,
-0.416051574755906));
#53624=CARTESIAN_POINT('Ctrl Pts',(0.0184354247754988,-0.0647068481265139,
-0.41076728985085));
#53625=CARTESIAN_POINT('Ctrl Pts',(0.0643617662685185,-0.0196062266863109,
-0.40521052280829));
#53626=CARTESIAN_POINT('Ctrl Pts',(0.0513795282529356,0.0434394424251984,
-0.399653755765729));
#53627=CARTESIAN_POINT('Ctrl Pts',(-0.00862899881670666,0.0667261677385573,
-0.394096988723167));
#53628=CARTESIAN_POINT('Ctrl Pts',(-0.0511119318649797,0.0359213830672153,
-0.38956686264241));
#53629=CARTESIAN_POINT('Ctrl Pts',(-0.0568582574067744,0.00848452046303413,
-0.386888992242506));
#53630=CARTESIAN_POINT('Ctrl Pts',(-0.0568360806176596,1.66360965570813E-5,
-0.386063377523455));
#53631=CARTESIAN_POINT('Ctrl Pts',(-0.0568337016952294,1.1550655372063E-5,
-0.414186622476544));
#53632=CARTESIAN_POINT('Ctrl Pts',(-0.0568151834460149,-0.0101976377276981,
-0.413191335367536));
#53633=CARTESIAN_POINT('Ctrl Pts',(-0.0493106185827779,-0.0394317914459927,
-0.410343792577675));
#53634=CARTESIAN_POINT('Ctrl Pts',(-0.00250413919046523,-0.0672351857005294,
-0.40564399410696));
#53635=CARTESIAN_POINT('Ctrl Pts',(0.0551290772461912,-0.0385697517672564,
-0.400087227064398));
#53636=CARTESIAN_POINT('Ctrl Pts',(0.0623041440991956,0.0253975301438741,
-0.394530460021838));
#53637=CARTESIAN_POINT('Ctrl Pts',(0.0124539172307667,0.0661191413657922,
-0.388973692979276));
#53638=CARTESIAN_POINT('Ctrl Pts',(-0.0439214343045913,0.0478988281231328,
-0.383859080464179));
#53639=CARTESIAN_POINT('Ctrl Pts',(-0.056789819113961,0.0143558336644252,
-0.380596723629935));
#53640=CARTESIAN_POINT('Ctrl Pts',(-0.0569215673661572,-5.2045648779895E-5,
-0.379186622476545));
#53641=CARTESIAN_POINT('Origin',(0.,0.,-0.648563377523455));
#53642=CARTESIAN_POINT('',(-0.0569706330856471,-4.38941456312225E-5,-0.456063377523455));
#53643=CARTESIAN_POINT('',(-0.0569639325591123,4.59969122256296E-5,-0.449186622476545));
#53644=CARTESIAN_POINT('',(-0.056925,-6.31153998696879E-15,-0.648563377523455));
#53645=CARTESIAN_POINT('Ctrl Pts',(-0.0569706330856471,-4.38941456312194E-5,
-0.456063377523455));
#53646=CARTESIAN_POINT('Ctrl Pts',(-0.0569950085154664,-0.00290511617904001,
-0.455782727079417));
#53647=CARTESIAN_POINT('Ctrl Pts',(-0.0554983653945712,-0.0246244424230611,
-0.453649820954524));
#53648=CARTESIAN_POINT('Ctrl Pts',(-0.0275638766252995,-0.0613764922967096,
-0.449664659148778));
#53649=CARTESIAN_POINT('Ctrl Pts',(0.0366154427383043,-0.0564459954504943,
-0.444107892106218));
#53650=CARTESIAN_POINT('Ctrl Pts',(0.0672816408378267,0.000147989916712509,
-0.438551125063656));
#53651=CARTESIAN_POINT('Ctrl Pts',(0.03636677707249,0.0566065244349891,
-0.432994358021095));
#53652=CARTESIAN_POINT('Ctrl Pts',(-0.0278336114842633,0.0612546418564424,
-0.427437590978534));
#53653=CARTESIAN_POINT('Ctrl Pts',(-0.055549228542257,0.0244556428036377,
-0.42346059747932));
#53654=CARTESIAN_POINT('Ctrl Pts',(-0.0569963080051652,0.00282073644233923,
-0.421335859660961));
#53655=CARTESIAN_POINT('Ctrl Pts',(-0.0569729394550437,4.30825583782333E-5,
-0.421063377523455));
#53656=CARTESIAN_POINT('Ctrl Pts',(-0.0569639325591123,4.59969122256318E-5,
-0.449186622476545));
#53657=CARTESIAN_POINT('Ctrl Pts',(-0.0568253048831882,-0.0157449120098894,
-0.447638202785992));
#53658=CARTESIAN_POINT('Ctrl Pts',(-0.041791862645694,-0.0506568766499107,
-0.444237527414586));
#53659=CARTESIAN_POINT('Ctrl Pts',(0.0173402153203343,-0.0650089058319875,
-0.438984596362326));
#53660=CARTESIAN_POINT('Ctrl Pts',(0.0640215365519545,-0.0206901853312933,
-0.433427829319765));
#53661=CARTESIAN_POINT('Ctrl Pts',(0.0521056812744453,0.042565700843469,
-0.427871062277204));
#53662=CARTESIAN_POINT('Ctrl Pts',(-0.00750109120977298,0.0668623551738915,
-0.422314295234643));
#53663=CARTESIAN_POINT('Ctrl Pts',(-0.0507956988943071,0.0365710802835814,
-0.41775281530109));
#53664=CARTESIAN_POINT('Ctrl Pts',(-0.0568496463984601,0.00880193235444248,
-0.41504359104839));
#53665=CARTESIAN_POINT('Ctrl Pts',(-0.0568337016952294,1.1550655372063E-5,
-0.414186622476544));
#53666=CARTESIAN_POINT('Origin',(0.,0.,-0.648563377523455));
#53667=CARTESIAN_POINT('',(-0.0568353689804243,-1.53335310629876E-5,-0.491063377523455));
#53668=CARTESIAN_POINT('',(-0.0569793078036176,-4.05823445219014E-5,-0.484186622476545));
#53669=CARTESIAN_POINT('',(-0.056925,-6.31153998696879E-15,-0.648563377523455));
#53670=CARTESIAN_POINT('Ctrl Pts',(-0.0568353689804243,-1.53335310629811E-5,
-0.491063377523455));
#53671=CARTESIAN_POINT('Ctrl Pts',(-0.0568559923612236,-0.0085672539106082,
-0.490229594497872));
#53672=CARTESIAN_POINT('Ctrl Pts',(-0.0510302827578428,-0.0360906550071068,
-0.487543555791435));
#53673=CARTESIAN_POINT('Ctrl Pts',(-0.00833536402932787,-0.066763496614655,
-0.483005261404145));
#53674=CARTESIAN_POINT('Ctrl Pts',(0.0515701169003231,-0.0432129907282631,
-0.477448494361583));
#53675=CARTESIAN_POINT('Ctrl Pts',(0.064274898304406,0.019889166643205,
-0.471891727319023));
#53676=CARTESIAN_POINT('Ctrl Pts',(0.0181505921945029,0.06478732343249,
-0.466334960276461));
#53677=CARTESIAN_POINT('Ctrl Pts',(-0.041417849183696,0.0511146760956519,
-0.461058843677939));
#53678=CARTESIAN_POINT('Ctrl Pts',(-0.0568341339139286,0.0159785694809599,
-0.45763498276027));
#53679=CARTESIAN_POINT('Ctrl Pts',(-0.0569706330856471,-4.38941456312194E-5,
-0.456063377523455));
#53680=CARTESIAN_POINT('Ctrl Pts',(-0.0569793078036176,-4.05823445219027E-5,
-0.484186622476545));
#53681=CARTESIAN_POINT('Ctrl Pts',(-0.0569998081283525,-0.00258114455950157,
-0.483937325885302));
#53682=CARTESIAN_POINT('Ctrl Pts',(-0.0556913749191376,-0.0239766562237817,
-0.481835773613205));
#53683=CARTESIAN_POINT('Ctrl Pts',(-0.0285962923612928,-0.0609023247957534,
-0.477881965660254));
#53684=CARTESIAN_POINT('Ctrl Pts',(0.0356571255076543,-0.057056201086242,
-0.472325198617693));
#53685=CARTESIAN_POINT('Ctrl Pts',(0.0672745469504301,-0.000988088271253046,
-0.466768431575132));
#53686=CARTESIAN_POINT('Ctrl Pts',(0.0373173977562224,0.0559843974121422,
-0.461211664532571));
#53687=CARTESIAN_POINT('Ctrl Pts',(-0.0267953527133393,0.0617158808562009,
-0.45565489749001));
#53688=CARTESIAN_POINT('Ctrl Pts',(-0.0553517446039958,0.0251037241258535,
-0.451646550138001));
#53689=CARTESIAN_POINT('Ctrl Pts',(-0.0569911345363634,0.0031445408531103,
-0.449490458466846));
#53690=CARTESIAN_POINT('Ctrl Pts',(-0.0569639325591123,4.59969122256318E-5,
-0.449186622476545));
#53691=CARTESIAN_POINT('Origin',(0.,0.,-0.648563377523455));
#53692=CARTESIAN_POINT('',(-0.0569136073811911,5.1183173943782E-5,-0.526063377523456));
#53693=CARTESIAN_POINT('',(-0.0568383386836465,-2.03536804905466E-5,-0.519186622476545));
#53694=CARTESIAN_POINT('',(-0.056925,-6.31153998696879E-15,-0.648563377523455));
#53695=CARTESIAN_POINT('Ctrl Pts',(-0.0569136073811911,5.11831739437789E-5,
-0.526063377523456));
#53696=CARTESIAN_POINT('Ctrl Pts',(-0.0567858168353036,-0.0141241822318066,
-0.524676461916328));
#53697=CARTESIAN_POINT('Ctrl Pts',(-0.0442628394021531,-0.0474313237476093,
-0.521437290628346));
#53698=CARTESIAN_POINT('Ctrl Pts',(0.0116281096388898,-0.0662701761988158,
-0.516345863659512));
#53699=CARTESIAN_POINT('Ctrl Pts',(0.061981763895487,-0.0261731483262298,
-0.51078909661695));
#53700=CARTESIAN_POINT('Ctrl Pts',(0.0556065904708322,0.0378781889557639,
-0.505232329574389));
#53701=CARTESIAN_POINT('Ctrl Pts',(-0.00166452598691655,0.0672613134374671,
-0.499675562531828));
#53702=CARTESIAN_POINT('Ctrl Pts',(-0.0490469843264066,0.0399101343193825,
-0.49495257851485));
#53703=CARTESIAN_POINT('Ctrl Pts',(-0.0568101773553145,0.0104309058254248,
-0.492081850178726));
#53704=CARTESIAN_POINT('Ctrl Pts',(-0.0568353689804243,-1.53335310629811E-5,
-0.491063377523455));
#53705=CARTESIAN_POINT('Ctrl Pts',(-0.0568383386836465,-2.03536804905492E-5,
-0.519186622476545));
#53706=CARTESIAN_POINT('Ctrl Pts',(-0.0568647265358007,-0.00824955685581068,
-0.518384193303757));
#53707=CARTESIAN_POINT('Ctrl Pts',(-0.0513411570398651,-0.0354405810816032,
-0.515729508450115));
#53708=CARTESIAN_POINT('Ctrl Pts',(-0.00946140608284985,-0.066613336227403,
-0.511222567915621));
#53709=CARTESIAN_POINT('Ctrl Pts',(0.0508330680958483,-0.0440775413718835,
-0.505665800873059));
#53710=CARTESIAN_POINT('Ctrl Pts',(0.0646015856194826,0.0188010149829039,
-0.500109033830499));
#53711=CARTESIAN_POINT('Ctrl Pts',(0.0192419326369567,0.0644716265578821,
-0.494552266787937));
#53712=CARTESIAN_POINT('Ctrl Pts',(-0.0409041756051557,0.0517314628965133,
-0.48924479633662));
#53713=CARTESIAN_POINT('Ctrl Pts',(-0.0568474921951092,0.0162950493418725,
-0.485789581566155));
#53714=CARTESIAN_POINT('Ctrl Pts',(-0.0569793078036176,-4.05823445219027E-5,
-0.484186622476545));
#53715=CARTESIAN_POINT('Origin',(0.,0.,-0.648563377523455));
#53716=CARTESIAN_POINT('',(-0.056925,-6.31153998696879E-15,-0.5608));
#53717=CARTESIAN_POINT('',(-0.0569002140125902,4.52833130624476E-5,-0.554186622476545));
#53718=CARTESIAN_POINT('',(-0.056925,-6.31153998696879E-15,-0.648563377523455));
#53719=CARTESIAN_POINT('',(-0.0568613829974076,-0.00269049226390444,-0.5608));
#53720=CARTESIAN_POINT('Origin',(0.,0.,-0.5608));
#53721=CARTESIAN_POINT('Ctrl Pts',(-0.0568613829974076,-0.00269049226390446,
-0.5608));
#53722=CARTESIAN_POINT('Ctrl Pts',(-0.0559667508352254,-0.0215978211189658,
-0.558947744319147));
#53723=CARTESIAN_POINT('Ctrl Pts',(-0.033852782438917,-0.0581229253359501,
-0.555243232957439));
#53724=CARTESIAN_POINT('Ctrl Pts',(0.0306018951616518,-0.0599703320683201,
-0.549686465914878));
#53725=CARTESIAN_POINT('Ctrl Pts',(0.0669157535097345,-0.00681168427321597,
-0.544129698872316));
#53726=CARTESIAN_POINT('Ctrl Pts',(0.0420494689529653,0.0525221733225254,
-0.538572931829757));
#53727=CARTESIAN_POINT('Ctrl Pts',(-0.0213379694595951,0.0638149374263822,
-0.533016164787193));
#53728=CARTESIAN_POINT('Ctrl Pts',(-0.0542353794736302,0.0284468929477895,
-0.528846313351762));
#53729=CARTESIAN_POINT('Ctrl Pts',(-0.0569564838631769,0.00480732374162209,
-0.526528717597182));
#53730=CARTESIAN_POINT('Ctrl Pts',(-0.0569136073811911,5.11831739437789E-5,
-0.526063377523456));
#53731=CARTESIAN_POINT('Ctrl Pts',(-0.0569002140125902,4.52833130624433E-5,
-0.554186622476545));
#53732=CARTESIAN_POINT('Ctrl Pts',(-0.0567793059135598,-0.0138144038624156,
-0.552831060722212));
#53733=CARTESIAN_POINT('Ctrl Pts',(-0.0447210948641033,-0.046791207995725,
-0.549623243287027));
#53734=CARTESIAN_POINT('Ctrl Pts',(0.0105110504745919,-0.0664618166825911,
-0.544563170170987));
#53735=CARTESIAN_POINT('Ctrl Pts',(0.0615291043141801,-0.0272134801016605,
-0.539006403128426));
#53736=CARTESIAN_POINT('Ctrl Pts',(0.0562392334272427,0.0369325451809627,
-0.533449636085865));
#53737=CARTESIAN_POINT('Ctrl Pts',(-0.000529100216082706,0.0672805255553111,
-0.527892869043304));
#53738=CARTESIAN_POINT('Ctrl Pts',(-0.048683516574914,0.0405561571276554,
-0.52313853117353));
#53739=CARTESIAN_POINT('Ctrl Pts',(-0.0568038151797388,0.0107459991973579,
-0.520236448984611));
#53740=CARTESIAN_POINT('Ctrl Pts',(-0.0568383386836465,-2.03536804905492E-5,
-0.519186622476545));
#53741=CARTESIAN_POINT('Ctrl Pts',(0.0565254421840275,-0.00673275656029218,
-0.572347005383793));
#53742=CARTESIAN_POINT('Ctrl Pts',(0.0587641925568829,0.0120628665447577,
-0.570494749702939));
#53743=CARTESIAN_POINT('Ctrl Pts',(0.04298296994418,0.0517373268281049,
-0.566790238341231));
#53744=CARTESIAN_POINT('Ctrl Pts',(-0.0202825412718916,0.0641991901194383,
-0.561233471298671));
#53745=CARTESIAN_POINT('Ctrl Pts',(-0.06487330649251,0.0177642870332536,
-0.555676704256109));
#53746=CARTESIAN_POINT('Ctrl Pts',(-0.0501426511359929,-0.0448603521282914,
-0.550119937213548));
#53747=CARTESIAN_POINT('Ctrl Pts',(0.0105110504745919,-0.0664618166825911,
-0.544563170170987));
#53748=CARTESIAN_POINT('Ctrl Pts',(0.0615291043141801,-0.0272134801016605,
-0.539006403128426));
#53749=CARTESIAN_POINT('Ctrl Pts',(0.0562392334272427,0.0369325451809627,
-0.533449636085865));
#53750=CARTESIAN_POINT('Ctrl Pts',(-0.000529100216082706,0.0672805255553111,
-0.527892869043304));
#53751=CARTESIAN_POINT('Ctrl Pts',(-0.0568109382145401,0.0360456630403476,
-0.522336102000743));
#53752=CARTESIAN_POINT('Ctrl Pts',(-0.0610964383375367,-0.0281793393520896,
-0.516779334958181));
#53753=CARTESIAN_POINT('Ctrl Pts',(-0.00946140608284985,-0.066613336227403,
-0.511222567915621));
#53754=CARTESIAN_POINT('Ctrl Pts',(0.0508330680958483,-0.0440775413718835,
-0.505665800873059));
#53755=CARTESIAN_POINT('Ctrl Pts',(0.0646015856194826,0.0188010149829039,
-0.500109033830499));
#53756=CARTESIAN_POINT('Ctrl Pts',(0.0192419326369567,0.0644716265578821,
-0.494552266787937));
#53757=CARTESIAN_POINT('Ctrl Pts',(-0.0437292916182991,0.0511330461174107,
-0.488995499745377));
#53758=CARTESIAN_POINT('Ctrl Pts',(-0.0666763062528489,-0.00900619312042977,
-0.483438732702815));
#53759=CARTESIAN_POINT('Ctrl Pts',(-0.0285962923612928,-0.0609023247957534,
-0.477881965660254));
#53760=CARTESIAN_POINT('Ctrl Pts',(0.0356571255076543,-0.057056201086242,
-0.472325198617693));
#53761=CARTESIAN_POINT('Ctrl Pts',(0.0672745469504301,-0.000988088271253046,
-0.466768431575132));
#53762=CARTESIAN_POINT('Ctrl Pts',(0.0373173977562224,0.0559843974121422,
-0.461211664532571));
#53763=CARTESIAN_POINT('Ctrl Pts',(-0.0267953527133393,0.0617158808562009,
-0.45565489749001));
#53764=CARTESIAN_POINT('Ctrl Pts',(-0.0663830439429782,0.0109604926600342,
-0.450098130447448));
#53765=CARTESIAN_POINT('Ctrl Pts',(-0.0452121347354353,-0.0498267376368557,
-0.444541363404887));
#53766=CARTESIAN_POINT('Ctrl Pts',(0.0173402153203343,-0.0650089058319875,
-0.438984596362326));
#53767=CARTESIAN_POINT('Ctrl Pts',(0.0640215365519545,-0.0206901853312933,
-0.433427829319765));
#53768=CARTESIAN_POINT('Ctrl Pts',(0.0521056812744453,0.042565700843469,
-0.427871062277204));
#53769=CARTESIAN_POINT('Ctrl Pts',(-0.00750109120977298,0.0668623551738915,
-0.422314295234643));
#53770=CARTESIAN_POINT('Ctrl Pts',(-0.0602423183129323,0.0299617087960569,
-0.416757528192082));
#53771=CARTESIAN_POINT('Ctrl Pts',(-0.0578453849239086,-0.034362077241173,
-0.411200761149521));
#53772=CARTESIAN_POINT('Ctrl Pts',(-0.00250413919046523,-0.0672351857005294,
-0.40564399410696));
#53773=CARTESIAN_POINT('Ctrl Pts',(0.0551290772461912,-0.0385697517672564,
-0.400087227064398));
#53774=CARTESIAN_POINT('Ctrl Pts',(0.0623041440991956,0.0253975301438741,
-0.394530460021838));
#53775=CARTESIAN_POINT('Ctrl Pts',(0.0124539172307667,0.0661191413657922,
-0.388973692979276));
#53776=CARTESIAN_POINT('Ctrl Pts',(-0.0487950423922266,0.0463236953113581,
-0.383416925936716));
#53777=CARTESIAN_POINT('Ctrl Pts',(-0.0653832227873078,-0.0158705729982893,
-0.377860158894154));
#53778=CARTESIAN_POINT('Ctrl Pts',(-0.0221279122263006,-0.0635389361718822,
-0.372303391851593));
#53779=CARTESIAN_POINT('Ctrl Pts',(0.0413804763988367,-0.0530518339207716,
-0.366746624809032));
#53780=CARTESIAN_POINT('Ctrl Pts',(0.0670144370045379,0.00599217342164428,
-0.361189857766471));
#53781=CARTESIAN_POINT('Ctrl Pts',(0.031311900511308,0.0595517069085378,
-0.35563309072391));
#53782=CARTESIAN_POINT('Ctrl Pts',(-0.0330495695001504,0.0586051778020126,
-0.350076323681349));
#53783=CARTESIAN_POINT('Ctrl Pts',(-0.0671616646846567,0.00401891852819577,
-0.344519556638788));
#53784=CARTESIAN_POINT('Ctrl Pts',(-0.0398025092666771,-0.0542457479018093,
-0.338962789596227));
#53785=CARTESIAN_POINT('Ctrl Pts',(0.0239868036411113,-0.0628607521465771,
-0.333406022553666));
#53786=CARTESIAN_POINT('Ctrl Pts',(0.0658216455765284,-0.0139410144160481,
-0.327849255511104));
#53787=CARTESIAN_POINT('Ctrl Pts',(0.0474117200646131,0.0477385557999543,
-0.322292488468544));
#53788=CARTESIAN_POINT('Ctrl Pts',(-0.0143928672572947,0.0657243203195322,
-0.316735721425982));
#53789=CARTESIAN_POINT('Ctrl Pts',(-0.063024053440091,0.0235543965605395,
-0.311178954383422));
#53790=CARTESIAN_POINT('Ctrl Pts',(-0.0539710324015399,-0.0401742276946618,
-0.30562218734086));
#53791=CARTESIAN_POINT('Ctrl Pts',(0.00448021117374274,-0.0671324706620369,
-0.300065420298299));
#53792=CARTESIAN_POINT('Ctrl Pts',(0.0588308389422806,-0.0326461835242353,
-0.294508653255737));
#53793=CARTESIAN_POINT('Ctrl Pts',(0.0593351950206278,0.0317202701945406,
-0.288951886213177));
#53794=CARTESIAN_POINT('Ctrl Pts',(0.00553165596584969,0.067054020696943,
-0.283395119170615));
#53795=CARTESIAN_POINT('Ctrl Pts',(-0.0533348578040438,0.0410150442200543,
-0.277838352128055));
#53796=CARTESIAN_POINT('Ctrl Pts',(-0.063385422396469,-0.0225638901116765,
-0.272281585085493));
#53797=CARTESIAN_POINT('Ctrl Pts',(-0.0154210285602653,-0.0654907076423372,
-0.266724818042933));
#53798=CARTESIAN_POINT('Ctrl Pts',(0.0466578145771441,-0.0484756562434736,
-0.261168051000371));
#53799=CARTESIAN_POINT('Ctrl Pts',(0.0660320251551521,0.0129078489013458,
-0.255611283957811));
#53800=CARTESIAN_POINT('Ctrl Pts',(0.024968913561939,0.062477149942095,
-0.250054516915249));
#53801=CARTESIAN_POINT('Ctrl Pts',(-0.0389475675843432,0.0548628097039661,
-0.244497749872688));
#53802=CARTESIAN_POINT('Ctrl Pts',(-0.0672163961809798,-0.00296597265533152,
-0.238940982830127));
#53803=CARTESIAN_POINT('Ctrl Pts',(-0.0339638799205846,-0.0580800806653254,
-0.233384215787566));
#53804=CARTESIAN_POINT('Ctrl Pts',(0.0303748547031255,-0.0600350656792724,
-0.227827448745005));
#53805=CARTESIAN_POINT('Ctrl Pts',(0.066912308428919,-0.00704158292317649,
-0.222270681702444));
#53806=CARTESIAN_POINT('Ctrl Pts',(0.0422067405718221,0.0523968697505238,
-0.216713914659883));
#53807=CARTESIAN_POINT('Ctrl Pts',(-0.0211295124981265,0.0638778882786663,
-0.211157147617322));
#53808=CARTESIAN_POINT('Ctrl Pts',(-0.0651264957036645,0.0168932077093837,
-0.20560038057476));
#53809=CARTESIAN_POINT('Ctrl Pts',(-0.0495149632915362,-0.0455533678182764,
-0.2000436135322));
#53810=CARTESIAN_POINT('Ctrl Pts',(0.0114162724268508,-0.0663061809579219,
-0.194486846489638));
#53811=CARTESIAN_POINT('Ctrl Pts',(0.0618985035444009,-0.0263707445538147,
-0.188930079447077));
#53812=CARTESIAN_POINT('Ctrl Pts',(0.0557267127407225,0.0377011192997421,
-0.183373312404516));
#53813=CARTESIAN_POINT('Ctrl Pts',(-0.00145022720861101,0.067266170921093,
-0.177816545361955));
#53814=CARTESIAN_POINT('Ctrl Pts',(-0.0572998135174467,0.0352643202156253,
-0.172259778319394));
#53815=CARTESIAN_POINT('Ctrl Pts',(-0.0607044341923943,-0.0290140065942496,
-0.166703011276833));
#53816=CARTESIAN_POINT('Ctrl Pts',(-0.00854793224978894,-0.0667365998802494,
-0.161146244234271));
#53817=CARTESIAN_POINT('Ctrl Pts',(0.0514322603095934,-0.0433769928549986,
-0.155589477191711));
#53818=CARTESIAN_POINT('Ctrl Pts',(0.0643378995797782,0.019684399569185,
-0.150032710149149));
#53819=CARTESIAN_POINT('Ctrl Pts',(0.0183568039000239,0.0647291948037812,
-0.144475943106589));
#53820=CARTESIAN_POINT('Ctrl Pts',(-0.0444257766806479,0.0505291131709007,
-0.138919176064027));
#53821=CARTESIAN_POINT('Ctrl Pts',(-0.0665466484015406,-0.00991889567187386,
-0.133362409021467));
#53822=CARTESIAN_POINT('Ctrl Pts',(-0.0277591773719423,-0.0612884082229279,
-0.127805641978905));
#53823=CARTESIAN_POINT('Ctrl Pts',(0.0364355162536436,-0.0565623026212381,
-0.122248874936344));
#53824=CARTESIAN_POINT('Ctrl Pts',(0.0672817693522171,-6.62549929698068E-5,
-0.116692107893783));
#53825=CARTESIAN_POINT('Ctrl Pts',(0.0365468441487368,0.0564904338066607,
-0.111135340851222));
#53826=CARTESIAN_POINT('Ctrl Pts',(-0.0276384181430455,0.0613429607075467,
-0.105578573808661));
#53827=CARTESIAN_POINT('Ctrl Pts',(-0.0665269826816367,0.0100499381659545,
-0.1000218067661));
#53828=CARTESIAN_POINT('Ctrl Pts',(-0.044525209609633,-0.0504415187277128,
-0.0944650397235386));
#53829=CARTESIAN_POINT('Ctrl Pts',(0.0182292914472235,-0.0647652241822597,
-0.0889082726809775));
#53830=CARTESIAN_POINT('Ctrl Pts',(0.0642989956139634,-0.0198110704839244,
-0.0833515056384163));
#53831=CARTESIAN_POINT('Ctrl Pts',(0.0515176118264206,0.0432756083068328,
-0.0777947385958553));
#53832=CARTESIAN_POINT('Ctrl Pts',(-0.00841651961310768,0.0667533162213003,
-0.0722379715532942));
#53833=CARTESIAN_POINT('Ctrl Pts',(-0.0606470977391485,0.0291334859096097,
-0.0666812045107331));
#53834=CARTESIAN_POINT('Ctrl Pts',(-0.0573692992813992,-0.0351513622548381,
-0.0611244374681719));
#53835=CARTESIAN_POINT('Ctrl Pts',(-0.00158242957906591,-0.0672632578788742,
-0.055567670425611));
#53836=CARTESIAN_POINT('Ctrl Pts',(0.0556518335368746,-0.0378106591957688,
-0.0500109033830497));
#53837=CARTESIAN_POINT('Ctrl Pts',(0.0619513051118907,0.0262485211196931,
-0.0444541363404888));
#53838=CARTESIAN_POINT('Ctrl Pts',(0.0115449715450025,0.0662840697456999,
-0.0388973692979276));
#53839=CARTESIAN_POINT('Ctrl Pts',(-0.0494216107805867,0.0456498473688679,
-0.0333406022553666));
#53840=CARTESIAN_POINT('Ctrl Pts',(-0.0651663525864486,-0.0167631067946381,
-0.0277838352128054));
#53841=CARTESIAN_POINT('Ctrl Pts',(-0.0212425420460525,-0.0638395728638739,
-0.0222270681702444));
#53842=CARTESIAN_POINT('Ctrl Pts',(0.0420792312090032,-0.0524733655289061,
-0.0166703011276832));
#53843=CARTESIAN_POINT('Ctrl Pts',(0.0669727390520183,0.00689708027414815,
-0.0111135340851222));
#53844=CARTESIAN_POINT('Ctrl Pts',(0.0303982238704425,0.0600019556186538,
-0.00555676704256101));
#53845=CARTESIAN_POINT('Ctrl Pts',(-0.012280390439628,0.0587191202828289,
-0.00185225568085369));
#53846=CARTESIAN_POINT('Ctrl Pts',(-0.0286389268003753,0.0491962142519396,
0.));
#53847=CARTESIAN_POINT('Ctrl Pts',(0.0631453153720266,-0.00752125096056136,
-0.568498003589195));
#53848=CARTESIAN_POINT('Ctrl Pts',(0.0656462528768225,0.013475586971606,
-0.566645747908341));
#53849=CARTESIAN_POINT('Ctrl Pts',(0.0480168414059497,0.057796448693495,
-0.562941236546634));
#53850=CARTESIAN_POINT('Ctrl Pts',(-0.022657893785068,0.0717177601817357,
-0.557384469504073));
#53851=CARTESIAN_POINT('Ctrl Pts',(-0.0724708244538636,0.0198447188333718,
-0.551827702461512));
#53852=CARTESIAN_POINT('Ctrl Pts',(-0.0560150154909626,-0.0501140897512789,
-0.54627093541895));
#53853=CARTESIAN_POINT('Ctrl Pts',(0.0117420328168065,-0.0742453700929372,
-0.54071416837639));
#53854=CARTESIAN_POINT('Ctrl Pts',(0.0687349721887727,-0.0304005367670585,
-0.535157401333827));
#53855=CARTESIAN_POINT('Ctrl Pts',(0.0628255878031463,0.04125783227579,
-0.529600634291268));
#53856=CARTESIAN_POINT('Ctrl Pts',(-0.00059106481465686,0.0751599605493455,
-0.524043867248705));
#53857=CARTESIAN_POINT('Ctrl Pts',(-0.0634642467450084,0.0402670845646169,
-0.518487100206145));
#53858=CARTESIAN_POINT('Ctrl Pts',(-0.0682516353321248,-0.0314795108469903,
-0.512930333163584));
#53859=CARTESIAN_POINT('Ctrl Pts',(-0.0105694612528521,-0.0744146345705331,
-0.507373566121023));
#53860=CARTESIAN_POINT('Ctrl Pts',(0.0567862893631114,-0.0492396015530446,
-0.501816799078462));
#53861=CARTESIAN_POINT('Ctrl Pts',(0.0721672814905979,0.0210028612698777,
-0.496260032035901));
#53862=CARTESIAN_POINT('Ctrl Pts',(0.0214954161839588,0.0720221025125452,
-0.49070326499334));
#53863=CARTESIAN_POINT('Ctrl Pts',(-0.0488505671701414,0.0571213987588882,
-0.485146497950779));
#53864=CARTESIAN_POINT('Ctrl Pts',(-0.0744849792146817,-0.0100609368616591,
-0.479589730908218));
#53865=CARTESIAN_POINT('Ctrl Pts',(-0.031945294540921,-0.0680347885399491,
-0.474032963865656));
#53866=CARTESIAN_POINT('Ctrl Pts',(0.03983304417346,-0.063738233126792,
-0.468476196823096));
#53867=CARTESIAN_POINT('Ctrl Pts',(0.075153281771151,-0.00110380641164368,
-0.462919429780533));
#53868=CARTESIAN_POINT('Ctrl Pts',(0.0416877561525016,0.0625409071368838,
-0.457362662737974));
#53869=CARTESIAN_POINT('Ctrl Pts',(-0.0299334411587596,0.0689436227219545,
-0.451805895695412));
#53870=CARTESIAN_POINT('Ctrl Pts',(-0.0741573720288194,0.0122441105970908,
-0.446249128652851));
#53871=CARTESIAN_POINT('Ctrl Pts',(-0.0505070707313879,-0.0556621043634669,
-0.44069236161029));
#53872=CARTESIAN_POINT('Ctrl Pts',(0.0193709827418336,-0.0726223042605618,
-0.435135594567729));
#53873=CARTESIAN_POINT('Ctrl Pts',(0.0715193010434728,-0.0231132783286642,
-0.429578827525168));
#53874=CARTESIAN_POINT('Ctrl Pts',(0.0582079422932654,0.047550704602036,
-0.424022060482607));
#53875=CARTESIAN_POINT('Ctrl Pts',(-0.00837956770923311,0.0746928169128921,
-0.418465293440046));
#53876=CARTESIAN_POINT('Ctrl Pts',(-0.067297486611914,0.0334706192098838,
-0.412908526397484));
#53877=CARTESIAN_POINT('Ctrl Pts',(-0.0646198407779753,-0.0383863287113727,
-0.407351759354924));
#53878=CARTESIAN_POINT('Ctrl Pts',(-0.00279740684562234,-0.0751093108008694,
-0.401794992312362));
#53879=CARTESIAN_POINT('Ctrl Pts',(0.0615854177229808,-0.0430867772999472,
-0.396238225269801));
#53880=CARTESIAN_POINT('Ctrl Pts',(0.069600779332596,0.0283719151702384,
-0.39068145822724));
#53881=CARTESIAN_POINT('Ctrl Pts',(0.0139124348394066,0.0738625629867309,
-0.385124691184679));
#53882=CARTESIAN_POINT('Ctrl Pts',(-0.054509584027972,0.051748809679546,
-0.379567924142117));
#53883=CARTESIAN_POINT('Ctrl Pts',(-0.0730404586575827,-0.0177292259625151,
-0.374011157099557));
#53884=CARTESIAN_POINT('Ctrl Pts',(-0.024719381964413,-0.0709801818075876,
-0.368454390056995));
#53885=CARTESIAN_POINT('Ctrl Pts',(0.0462266747766825,-0.0592649018664049,
-0.362897623014435));
#53886=CARTESIAN_POINT('Ctrl Pts',(0.0748627095273941,0.00669393578986403,
-0.357340855971873));
#53887=CARTESIAN_POINT('Ctrl Pts',(0.0349789361443122,0.0665259955232103,
-0.351784088929313));
#53888=CARTESIAN_POINT('Ctrl Pts',(-0.0369201090404981,0.0654686154014289,
-0.346227321886751));
#53889=CARTESIAN_POINT('Ctrl Pts',(-0.0750271795064581,0.00448958677919307,
-0.34067055484419));
#53890=CARTESIAN_POINT('Ctrl Pts',(-0.0444639069263677,-0.0605986388872351,
-0.335113787801629));
#53891=CARTESIAN_POINT('Ctrl Pts',(0.0267959740280068,-0.0702225735076171,
-0.329557020759068));
#53892=CARTESIAN_POINT('Ctrl Pts',(0.0735302265253239,-0.0155736906761628,
-0.324000253716507));
#53893=CARTESIAN_POINT('Ctrl Pts',(0.0529642564504562,0.0533293689517563,
-0.318443486673946));
#53894=CARTESIAN_POINT('Ctrl Pts',(-0.0160784614317684,0.0734215031998758,
-0.312886719631385));
#53895=CARTESIAN_POINT('Ctrl Pts',(-0.0704049995317425,0.0263129263875688,
-0.307329952588823));
#53896=CARTESIAN_POINT('Ctrl Pts',(-0.0602917505864667,-0.0448791584743024,
-0.301773185546263));
#53897=CARTESIAN_POINT('Ctrl Pts',(0.00500490286441585,-0.074994566479579,
-0.296216418503701));
#53898=CARTESIAN_POINT('Ctrl Pts',(0.0657207044310556,-0.0364694812580068,
-0.290659651461141));
#53899=CARTESIAN_POINT('Ctrl Pts',(0.0662841272438023,0.0354351312918364,
-0.285102884418579));
#53900=CARTESIAN_POINT('Ctrl Pts',(0.00617948567931561,0.0749069289911245,
-0.279546117376018));
#53901=CARTESIAN_POINT('Ctrl Pts',(-0.0595810715711688,0.0458184456804626,
-0.273989350333457));
#53902=CARTESIAN_POINT('Ctrl Pts',(-0.070808689548742,-0.0252064185978917,
-0.268432583290896));
#53903=CARTESIAN_POINT('Ctrl Pts',(-0.0172270339545294,-0.0731605314036999,
-0.262875816248335));
#53904=CARTESIAN_POINT('Ctrl Pts',(0.0521220587085613,-0.0541527935578907,
-0.257319049205774));
#53905=CARTESIAN_POINT('Ctrl Pts',(0.0737652443213244,0.014419527882618,
-0.251762282163213));
#53906=CARTESIAN_POINT('Ctrl Pts',(0.0278931019457125,0.0697940464365575,
-0.246205515120652));
#53907=CARTESIAN_POINT('Ctrl Pts',(-0.0435088403214929,0.0612879667473238,
-0.240648748078091));
#53908=CARTESIAN_POINT('Ctrl Pts',(-0.0750883207812995,-0.00331332708722427,
-0.235091981035529));
#53909=CARTESIAN_POINT('Ctrl Pts',(-0.0379414972440325,-0.0648820224794459,
-0.229535213992968));
#53910=CARTESIAN_POINT('Ctrl Pts',(0.0339321499399129,-0.067065961967286,
-0.223978446950407));
#53911=CARTESIAN_POINT('Ctrl Pts',(0.0747486203514977,-0.00786624495487712,
-0.218421679907846));
#53912=CARTESIAN_POINT('Ctrl Pts',(0.047149705358451,0.0585332327721041,
-0.212864912865285));
#53913=CARTESIAN_POINT('Ctrl Pts',(-0.0236040564885372,0.0713588296668868,
-0.207308145822724));
#53914=CARTESIAN_POINT('Ctrl Pts',(-0.0727536654537641,0.0188716246567578,
-0.201751378780163));
#53915=CARTESIAN_POINT('Ctrl Pts',(-0.0553138171391768,-0.0508882666990576,
-0.196194611737602));
#53916=CARTESIAN_POINT('Ctrl Pts',(0.0127532681729312,-0.0740715073766511,
-0.190637844695041));
#53917=CARTESIAN_POINT('Ctrl Pts',(0.0691476329303646,-0.0294591057956617,
-0.18508107765248));
#53918=CARTESIAN_POINT('Ctrl Pts',(0.0622530441991593,0.0421164165387684,
-0.179524310609919));
#53919=CARTESIAN_POINT('Ctrl Pts',(-0.00162006790058625,0.0751439247985451,
-0.173967543567357));
#53920=CARTESIAN_POINT('Ctrl Pts',(-0.0640103757797735,0.0393942362121858,
-0.168410776524797));
#53921=CARTESIAN_POINT('Ctrl Pts',(-0.06781372234258,-0.0324119286079217,
-0.162854009482235));
#53922=CARTESIAN_POINT('Ctrl Pts',(-0.00954900761208391,-0.0745523340193503,
-0.157297242439674));
#53923=CARTESIAN_POINT('Ctrl Pts',(0.05745565487081,-0.0484570095851997,
-0.151740475397113));
#53924=CARTESIAN_POINT('Ctrl Pts',(0.0718727143453798,0.0219897018170759,
-0.146183708354552));
#53925=CARTESIAN_POINT('Ctrl Pts',(0.0205066272231135,0.0723098353897895,
-0.140626941311991));
#53926=CARTESIAN_POINT('Ctrl Pts',(-0.0496286197994466,0.0564467373162272,
-0.13507017426943));
#53927=CARTESIAN_POINT('Ctrl Pts',(-0.0743401367226111,-0.0110805288935828,
-0.129513407226869));
#53928=CARTESIAN_POINT('Ctrl Pts',(-0.0310101423693891,-0.0684660874175319,
-0.123956640184308));
#53929=CARTESIAN_POINT('Ctrl Pts',(0.0407025947198872,-0.0631864926515402,
-0.118399873141746));
#53930=CARTESIAN_POINT('Ctrl Pts',(0.0751613500112382,-7.40143246023484E-5,
-0.112843106099186));
#53931=CARTESIAN_POINT('Ctrl Pts',(0.0408269605766383,0.0631062070529388,
-0.107286339056624));
#53932=CARTESIAN_POINT('Ctrl Pts',(-0.030875240645524,0.0685270287160431,
-0.101729572014063));
#53933=CARTESIAN_POINT('Ctrl Pts',(-0.0743181678880937,0.0112269181883187,
-0.0961728049715021));
#53934=CARTESIAN_POINT('Ctrl Pts',(-0.0497396976330133,-0.0563488844109461,
-0.090616037928941));
#53935=CARTESIAN_POINT('Ctrl Pts',(0.0203641813839491,-0.0723500842826564,
-0.08505927088638));
#53936=CARTESIAN_POINT('Ctrl Pts',(0.0718292542131685,-0.022131207562997,
-0.0795025038438188));
#53937=CARTESIAN_POINT('Ctrl Pts',(0.0575510021735351,0.0483437515721617,
-0.0739457368012578));
#53938=CARTESIAN_POINT('Ctrl Pts',(-0.00940220482617748,0.0745710080639356,
-0.0683889697586965));
#53939=CARTESIAN_POINT('Ctrl Pts',(-0.0677496710360767,0.0325454005235305,
-0.0628322027161357));
#53940=CARTESIAN_POINT('Ctrl Pts',(-0.0640879992411595,-0.0392680493875954,
-0.0572754356735743));
#53941=CARTESIAN_POINT('Ctrl Pts',(-0.00176775290848452,-0.0751406706007451,
-0.0517186686310135));
#53942=CARTESIAN_POINT('Ctrl Pts',(0.0621693956550852,-0.0422387849982311,
-0.0461619015884522));
#53943=CARTESIAN_POINT('Ctrl Pts',(0.069206618256308,0.0293225683888702,
-0.0406051345458912));
#53944=CARTESIAN_POINT('Ctrl Pts',(0.0128970396515766,0.074046806650481,
-0.0350483675033301));
#53945=CARTESIAN_POINT('Ctrl Pts',(-0.0552095318206196,0.0509960452747527,
-0.029491600460769));
#53946=CARTESIAN_POINT('Ctrl Pts',(-0.0727981901020628,-0.0187262872126889,
-0.0239348334182079));
#53947=CARTESIAN_POINT('Ctrl Pts',(-0.0237303232840627,-0.0713160270127682,
-0.0183780663756468));
#53948=CARTESIAN_POINT('Ctrl Pts',(0.0470072629711461,-0.0586186872128659,
-0.0128212993330857));
#53949=CARTESIAN_POINT('Ctrl Pts',(0.0748161281958647,0.00770481914390555,
-0.00726453229052467));
#53950=CARTESIAN_POINT('Ctrl Pts',(0.0339582559442764,0.0670289742828201,
-0.00170776524796349));
#53951=CARTESIAN_POINT('Ctrl Pts',(-0.0137185857773087,0.065595902046299,
0.00199674611374385));
#53952=CARTESIAN_POINT('Ctrl Pts',(-0.031992922033913,0.0549577383921174,
0.00384900179459754));
#53953=CARTESIAN_POINT('Ctrl Pts',(0.0697651885600256,-0.00830974536083054,
-0.564649001794598));
#53954=CARTESIAN_POINT('Ctrl Pts',(0.0725283131967621,0.0148883073984543,
-0.562796746113744));
#53955=CARTESIAN_POINT('Ctrl Pts',(0.0530507128677194,0.0638555705588852,
-0.559092234752036));
#53956=CARTESIAN_POINT('Ctrl Pts',(-0.0250332462982443,0.0792363302440328,
-0.553535467709476));
#53957=CARTESIAN_POINT('Ctrl Pts',(-0.0800683424152172,0.0219251506334903,
-0.547978700666914));
#53958=CARTESIAN_POINT('Ctrl Pts',(-0.0618873798459324,-0.0553678273742666,
-0.542421933624354));
#53959=CARTESIAN_POINT('Ctrl Pts',(0.0129730151590211,-0.0820289235032833,
-0.536865166581792));
#53960=CARTESIAN_POINT('Ctrl Pts',(0.0759408400633652,-0.0335875934324565,
-0.53130839953923));
#53961=CARTESIAN_POINT('Ctrl Pts',(0.0694119421790499,0.0455831193706172,
-0.525751632496671));
#53962=CARTESIAN_POINT('Ctrl Pts',(-0.000653029413231036,0.08303939554338,
-0.520194865454108));
#53963=CARTESIAN_POINT('Ctrl Pts',(-0.0701175552754767,0.044488506088886,
-0.514638098411548));
#53964=CARTESIAN_POINT('Ctrl Pts',(-0.0754068323267131,-0.0347796823418909,
-0.509081331368986));
#53965=CARTESIAN_POINT('Ctrl Pts',(-0.0116775164228544,-0.0822159329136632,
-0.503524564326426));
#53966=CARTESIAN_POINT('Ctrl Pts',(0.0627395106303746,-0.0544016617342056,
-0.497967797283864));
#53967=CARTESIAN_POINT('Ctrl Pts',(0.079732977361713,0.0232047075568513,
-0.492411030241303));
#53968=CARTESIAN_POINT('Ctrl Pts',(0.0237488997309608,0.0795725784672084,
-0.486854263198742));
#53969=CARTESIAN_POINT('Ctrl Pts',(-0.0539718427219837,0.0631097514003656,
-0.481297496156181));
#53970=CARTESIAN_POINT('Ctrl Pts',(-0.0822936521765144,-0.0111156806028886,
-0.475740729113621));
#53971=CARTESIAN_POINT('Ctrl Pts',(-0.0352942967205491,-0.0751672522841446,
-0.470183962071058));
#53972=CARTESIAN_POINT('Ctrl Pts',(0.0440089628392656,-0.070420265167342,
-0.464627195028499));
#53973=CARTESIAN_POINT('Ctrl Pts',(0.0830320165918719,-0.00121952455203425,
-0.459070427985936));
#53974=CARTESIAN_POINT('Ctrl Pts',(0.0460581145487806,0.0690974168616255,
-0.453513660943376));
#53975=CARTESIAN_POINT('Ctrl Pts',(-0.0330715296041798,0.0761713645877082,
-0.447956893900814));
#53976=CARTESIAN_POINT('Ctrl Pts',(-0.0819317001146608,0.0135277285341473,
-0.442400126858254));
#53977=CARTESIAN_POINT('Ctrl Pts',(-0.0558020067273405,-0.061497471090078,
-0.436843359815692));
#53978=CARTESIAN_POINT('Ctrl Pts',(0.0214017501633328,-0.0802357026891362,
-0.431286592773131));
#53979=CARTESIAN_POINT('Ctrl Pts',(0.0790170655349912,-0.0255363713260351,
-0.42572982573057));
#53980=CARTESIAN_POINT('Ctrl Pts',(0.0643102033120854,0.052535708360603,
-0.420173058688009));
#53981=CARTESIAN_POINT('Ctrl Pts',(-0.00925804420869325,0.0825232786518928,
-0.414616291645448));
#53982=CARTESIAN_POINT('Ctrl Pts',(-0.0743526549108956,0.0369795296237106,
-0.409059524602887));
#53983=CARTESIAN_POINT('Ctrl Pts',(-0.0713942966320421,-0.0424105801815723,
-0.403502757560325));
#53984=CARTESIAN_POINT('Ctrl Pts',(-0.00309067450077944,-0.0829834359012095,
-0.397945990517765));
#53985=CARTESIAN_POINT('Ctrl Pts',(0.0680417581997704,-0.0476038028326378,
-0.392389223475203));
#53986=CARTESIAN_POINT('Ctrl Pts',(0.0768974145659965,0.0313463001966025,
-0.386832456432643));
#53987=CARTESIAN_POINT('Ctrl Pts',(0.0153709524480465,0.0816059846076698,
-0.381275689390081));
#53988=CARTESIAN_POINT('Ctrl Pts',(-0.0602241256637174,0.0571739240477337,
-0.37571892234752));
#53989=CARTESIAN_POINT('Ctrl Pts',(-0.0806976945278576,-0.0195878789267407,
-0.370162155304959));
#53990=CARTESIAN_POINT('Ctrl Pts',(-0.0273108517025254,-0.0784214274432931,
-0.364605388262398));
#53991=CARTESIAN_POINT('Ctrl Pts',(0.0510728731545283,-0.0654779698120381,
-0.359048621219837));
#53992=CARTESIAN_POINT('Ctrl Pts',(0.0827109820502502,0.00739569815808381,
-0.353491854177276));
#53993=CARTESIAN_POINT('Ctrl Pts',(0.0386459717773164,0.0735002841378828,
-0.347935087134715));
#53994=CARTESIAN_POINT('Ctrl Pts',(-0.0407906485808458,0.0723320530008452,
-0.342378320092154));
#53995=CARTESIAN_POINT('Ctrl Pts',(-0.0828926943282594,0.00496025503019042,
-0.336821553049593));
#53996=CARTESIAN_POINT('Ctrl Pts',(-0.0491253045860583,-0.066951529872661,
-0.331264786007031));
#53997=CARTESIAN_POINT('Ctrl Pts',(0.0296051444149024,-0.077584394868657,
-0.325708018964471));
#53998=CARTESIAN_POINT('Ctrl Pts',(0.0812388074741194,-0.0172063669362776,
-0.320151251921909));
#53999=CARTESIAN_POINT('Ctrl Pts',(0.0585167928362994,0.0589201821035582,
-0.314594484879348));
#54000=CARTESIAN_POINT('Ctrl Pts',(-0.0177640556062421,0.0811186860802194,
-0.309037717836787));
#54001=CARTESIAN_POINT('Ctrl Pts',(-0.0777859456233938,0.0290714562145981,
-0.303480950794226));
#54002=CARTESIAN_POINT('Ctrl Pts',(-0.0666124687713937,-0.0495840892539429,
-0.297924183751665));
#54003=CARTESIAN_POINT('Ctrl Pts',(0.00552959455508908,-0.0828566622971212,
-0.292367416709103));
#54004=CARTESIAN_POINT('Ctrl Pts',(0.0726105699198304,-0.0402927789917783,
-0.286810649666543));
#54005=CARTESIAN_POINT('Ctrl Pts',(0.0732330594669769,0.0391499923891321,
-0.281253882623981));
#54006=CARTESIAN_POINT('Ctrl Pts',(0.00682731539278151,0.0827598372853061,
-0.275697115581421));
#54007=CARTESIAN_POINT('Ctrl Pts',(-0.0658272853382939,0.0506218471408707,
-0.270140348538859));
#54008=CARTESIAN_POINT('Ctrl Pts',(-0.0782319567010151,-0.0278489470841068,
-0.264583581496299));
#54009=CARTESIAN_POINT('Ctrl Pts',(-0.0190330393487936,-0.0808303551650625,
-0.259026814453737));
#54010=CARTESIAN_POINT('Ctrl Pts',(0.0575863028399786,-0.0598299308723078,
-0.253470047411176));
#54011=CARTESIAN_POINT('Ctrl Pts',(0.0814984634874966,0.0159312068638903,
-0.247913280368615));
#54012=CARTESIAN_POINT('Ctrl Pts',(0.0308172903294861,0.07711094293102,
-0.242356513326054));
#54013=CARTESIAN_POINT('Ctrl Pts',(-0.0480701130586427,0.0677131237906815,
-0.236799746283493));
#54014=CARTESIAN_POINT('Ctrl Pts',(-0.0829602453816192,-0.00366068151911704,
-0.231242979240932));
#54015=CARTESIAN_POINT('Ctrl Pts',(-0.0419191145674805,-0.0716839642935664,
-0.225686212198371));
#54016=CARTESIAN_POINT('Ctrl Pts',(0.0374894451767004,-0.0740968582552996,
-0.22012944515581));
#54017=CARTESIAN_POINT('Ctrl Pts',(0.0825849322740763,-0.00869090698657777,
-0.214572678113249));
#54018=CARTESIAN_POINT('Ctrl Pts',(0.05209267014508,0.0646695957936844,
-0.209015911070688));
#54019=CARTESIAN_POINT('Ctrl Pts',(-0.0260786004789479,0.0788397710551074,
-0.203459144028126));
#54020=CARTESIAN_POINT('Ctrl Pts',(-0.0803808352038637,0.020850041604132,
-0.197902376985565));
#54021=CARTESIAN_POINT('Ctrl Pts',(-0.0611126709868174,-0.0562231655798389,
-0.192345609943004));
#54022=CARTESIAN_POINT('Ctrl Pts',(0.0140902639190115,-0.0818368337953801,
-0.186788842900443));
#54023=CARTESIAN_POINT('Ctrl Pts',(0.0763967623163283,-0.0325474670375087,
-0.181232075857882));
#54024=CARTESIAN_POINT('Ctrl Pts',(0.0687793756575961,0.0465317137777947,
-0.175675308815321));
#54025=CARTESIAN_POINT('Ctrl Pts',(-0.00178990859256147,0.0830216786759971,
-0.17011854177276));
#54026=CARTESIAN_POINT('Ctrl Pts',(-0.0707209380421003,0.0435241522087464,
-0.164561774730199));
#54027=CARTESIAN_POINT('Ctrl Pts',(-0.0749230104927655,-0.0358098506215939,
-0.159005007687638));
#54028=CARTESIAN_POINT('Ctrl Pts',(-0.010550082974379,-0.0823680681584513,
-0.153448240645076));
#54029=CARTESIAN_POINT('Ctrl Pts',(0.0634790494320266,-0.0535370263154007,
-0.147891473602516));
#54030=CARTESIAN_POINT('Ctrl Pts',(0.0794075291109813,0.0242950040649667,
-0.142334706559954));
#54031=CARTESIAN_POINT('Ctrl Pts',(0.0226564505462031,0.0798904759757979,
-0.136777939517394));
#54032=CARTESIAN_POINT('Ctrl Pts',(-0.0548314629182453,0.0623643614615536,
-0.131221172474832));
#54033=CARTESIAN_POINT('Ctrl Pts',(-0.0821336250436817,-0.0122421621152916,
-0.125664405432271));
#54034=CARTESIAN_POINT('Ctrl Pts',(-0.034261107366836,-0.0756437666121359,
-0.12010763838971));
#54035=CARTESIAN_POINT('Ctrl Pts',(0.0449696731861309,-0.0698106826818423,
-0.114550871347149));
#54036=CARTESIAN_POINT('Ctrl Pts',(0.0830409306702594,-8.1773656234945E-5,
-0.108994104304588));
#54037=CARTESIAN_POINT('Ctrl Pts',(0.0451070770045397,0.069721980299217,
-0.103437337262027));
#54038=CARTESIAN_POINT('Ctrl Pts',(-0.0341120631480026,0.0757110967245396,
-0.0978805702194658));
#54039=CARTESIAN_POINT('Ctrl Pts',(-0.0821093530945509,0.0124038982106829,
-0.0923238031769044));
#54040=CARTESIAN_POINT('Ctrl Pts',(-0.0549541856563936,-0.0622562500941794,
-0.0867670361343436));
#54041=CARTESIAN_POINT('Ctrl Pts',(0.0224990713206748,-0.079934944383053,
-0.0812102690917824));
#54042=CARTESIAN_POINT('Ctrl Pts',(0.0793595128123734,-0.0244513446420697,
-0.0756535020492213));
#54043=CARTESIAN_POINT('Ctrl Pts',(0.0635843925206498,0.0534118948374907,
-0.0700967350066603));
#54044=CARTESIAN_POINT('Ctrl Pts',(-0.0103878900392474,0.0823886999065706,
-0.064539967964099));
#54045=CARTESIAN_POINT('Ctrl Pts',(-0.0748522443330048,0.0359573151374515,
-0.0589832009215382));
#54046=CARTESIAN_POINT('Ctrl Pts',(-0.0708066992009198,-0.0433847365203528,
-0.0534264338789768));
#54047=CARTESIAN_POINT('Ctrl Pts',(-0.00195307623790311,-0.0830180833226157,
-0.0478696668364159));
#54048=CARTESIAN_POINT('Ctrl Pts',(0.0686869577732957,-0.0466669108006935,
-0.0423128997938547));
#54049=CARTESIAN_POINT('Ctrl Pts',(0.0764619314007254,0.0323966156580473,
-0.0367561327512937));
#54050=CARTESIAN_POINT('Ctrl Pts',(0.0142491077581508,0.0818095435552619,
-0.0311993657087326));
#54051=CARTESIAN_POINT('Ctrl Pts',(-0.0609974528606526,0.0563422431806374,
-0.0256425986661715));
#54052=CARTESIAN_POINT('Ctrl Pts',(-0.080430027617677,-0.0206894676307396,
-0.0200858316236103));
#54053=CARTESIAN_POINT('Ctrl Pts',(-0.0262181045220728,-0.0787924811616626,
-0.0145290645810493));
#54054=CARTESIAN_POINT('Ctrl Pts',(0.051935294733289,-0.0647640088968256,
-0.00897229753848818));
#54055=CARTESIAN_POINT('Ctrl Pts',(0.0826595173397112,0.00851255801366293,
-0.00341553049592713));
#54056=CARTESIAN_POINT('Ctrl Pts',(0.0375182880181104,0.0740559929469865,
0.00214123654663404));
#54057=CARTESIAN_POINT('Ctrl Pts',(-0.0151567811149895,0.0724726838097691,
0.00584574790834138));
#54058=CARTESIAN_POINT('Ctrl Pts',(-0.0353469172674506,0.0607192625322951,
0.00769800358919507));
#54059=CARTESIAN_POINT('Ctrl Pts',(0.0763850617480247,-0.00909823976109972,
-0.5608));
#54060=CARTESIAN_POINT('Ctrl Pts',(0.0794103735167017,0.0163010278253026,
-0.558947744319146));
#54061=CARTESIAN_POINT('Ctrl Pts',(0.0580845843294891,0.0699146924242753,
-0.555243232957439));
#54062=CARTESIAN_POINT('Ctrl Pts',(-0.0274085988114208,0.0867549003063301,
-0.549686465914878));
#54063=CARTESIAN_POINT('Ctrl Pts',(-0.0876658603765707,0.0240055824336086,
-0.544129698872316));
#54064=CARTESIAN_POINT('Ctrl Pts',(-0.0677597442009021,-0.0606215649972542,
-0.538572931829756));
#54065=CARTESIAN_POINT('Ctrl Pts',(0.0142039975012356,-0.0898124769136294,
-0.533016164787195));
#54066=CARTESIAN_POINT('Ctrl Pts',(0.0831467079379578,-0.0367746500978545,
-0.527459397744632));
#54067=CARTESIAN_POINT('Ctrl Pts',(0.0759982965549535,0.0499084064654446,
-0.521902630702073));
#54068=CARTESIAN_POINT('Ctrl Pts',(-0.000714994011805219,0.0909188305374142,
-0.51634586365951));
#54069=CARTESIAN_POINT('Ctrl Pts',(-0.076770863805945,0.0487099276131553,
-0.510789096616951));
#54070=CARTESIAN_POINT('Ctrl Pts',(-0.0825620293213013,-0.0380798538367916,
-0.505232329574389));
#54071=CARTESIAN_POINT('Ctrl Pts',(-0.0127855715928567,-0.0900172312567932,
-0.499675562531827));
#54072=CARTESIAN_POINT('Ctrl Pts',(0.0686927318976377,-0.0595637219153667,
-0.494118795489267));
#54073=CARTESIAN_POINT('Ctrl Pts',(0.0872986732328282,0.0254065538438251,
-0.488562028446705));
#54074=CARTESIAN_POINT('Ctrl Pts',(0.0260023832779629,0.0871230544218715,
-0.483005261404145));
#54075=CARTESIAN_POINT('Ctrl Pts',(-0.059093118273826,0.0690981040418431,
-0.477448494361583));
#54076=CARTESIAN_POINT('Ctrl Pts',(-0.0901023251383473,-0.012170424344118,
-0.471891727319023));
#54077=CARTESIAN_POINT('Ctrl Pts',(-0.0386432989001772,-0.0822997160283402,
-0.46633496027646));
#54078=CARTESIAN_POINT('Ctrl Pts',(0.0481848815050713,-0.077102297207892,
-0.460778193233902));
#54079=CARTESIAN_POINT('Ctrl Pts',(0.0909107514125927,-0.00133524269242489,
-0.455221426191338));
#54080=CARTESIAN_POINT('Ctrl Pts',(0.0504284729450598,0.0756539265863672,
-0.449664659148779));
#54081=CARTESIAN_POINT('Ctrl Pts',(-0.0362096180496001,0.0833991064534618,
-0.444107892106217));
#54082=CARTESIAN_POINT('Ctrl Pts',(-0.089706028200502,0.0148113464712039,
-0.438551125063656));
#54083=CARTESIAN_POINT('Ctrl Pts',(-0.0610969427232932,-0.0673328378166892,
-0.432994358021095));
#54084=CARTESIAN_POINT('Ctrl Pts',(0.0234325175848321,-0.0878491011177105,
-0.427437590978534));
#54085=CARTESIAN_POINT('Ctrl Pts',(0.0865148300265095,-0.027959464323406,
-0.421880823935973));
#54086=CARTESIAN_POINT('Ctrl Pts',(0.0704124643309056,0.0575207121191699,
-0.416324056893412));
#54087=CARTESIAN_POINT('Ctrl Pts',(-0.0101365207081535,0.0903537403908936,
-0.41076728985085));
#54088=CARTESIAN_POINT('Ctrl Pts',(-0.0814078232098771,0.0404884400375374,
-0.405210522808289));
#54089=CARTESIAN_POINT('Ctrl Pts',(-0.0781687524861088,-0.0464348316517719,
-0.399653755765728));
#54090=CARTESIAN_POINT('Ctrl Pts',(-0.00338394215593656,-0.0908575610015496,
-0.394096988723167));
#54091=CARTESIAN_POINT('Ctrl Pts',(0.07449809867656,-0.0521208283653285,
-0.388540221680606));
#54092=CARTESIAN_POINT('Ctrl Pts',(0.084194049799397,0.0343206852229668,
-0.382983454638044));
#54093=CARTESIAN_POINT('Ctrl Pts',(0.0168294700566864,0.0893494062286084,
-0.377426687595484));
#54094=CARTESIAN_POINT('Ctrl Pts',(-0.0659386672994629,0.0625990384159216,
-0.371869920552922));
#54095=CARTESIAN_POINT('Ctrl Pts',(-0.0883549303981324,-0.0214465318909665,
-0.366313153510362));
#54096=CARTESIAN_POINT('Ctrl Pts',(-0.0299023214406378,-0.0858626730789984,
-0.3607563864678));
#54097=CARTESIAN_POINT('Ctrl Pts',(0.055919071532374,-0.0716910377576715,
-0.35519961942524));
#54098=CARTESIAN_POINT('Ctrl Pts',(0.0905592545731065,0.00809746052630369,
-0.349642852382678));
#54099=CARTESIAN_POINT('Ctrl Pts',(0.0423130074103206,0.0804745727525552,
-0.344086085340117));
#54100=CARTESIAN_POINT('Ctrl Pts',(-0.0446611881211935,0.0791954906002617,
-0.338529318297556));
#54101=CARTESIAN_POINT('Ctrl Pts',(-0.0907582091500607,0.00543092328118761,
-0.332972551254996));
#54102=CARTESIAN_POINT('Ctrl Pts',(-0.053786702245749,-0.0733044208580867,
-0.327415784212434));
#54103=CARTESIAN_POINT('Ctrl Pts',(0.032414314801798,-0.084946216229697,
-0.321859017169873));
#54104=CARTESIAN_POINT('Ctrl Pts',(0.0889473884229148,-0.0188390431963924,
-0.316302250127312));
#54105=CARTESIAN_POINT('Ctrl Pts',(0.0640693292221425,0.0645109952553602,
-0.310745483084751));
#54106=CARTESIAN_POINT('Ctrl Pts',(-0.0194496497807158,0.088815868960563,
-0.30518871604219));
#54107=CARTESIAN_POINT('Ctrl Pts',(-0.0851668917150452,0.0318299860416274,
-0.299631948999629));
#54108=CARTESIAN_POINT('Ctrl Pts',(-0.0729331869563206,-0.0542890200335835,
-0.294075181957068));
#54109=CARTESIAN_POINT('Ctrl Pts',(0.00605428624576221,-0.0907187581146632,
-0.288518414914506));
#54110=CARTESIAN_POINT('Ctrl Pts',(0.0795004354086054,-0.0441160767255499,
-0.282961647871945));
#54111=CARTESIAN_POINT('Ctrl Pts',(0.0801819916901514,0.0428648534864279,
-0.277404880829384));
#54112=CARTESIAN_POINT('Ctrl Pts',(0.00747514510624739,0.0906127455794876,
-0.271848113786823));
#54113=CARTESIAN_POINT('Ctrl Pts',(-0.0720734991054189,0.0554252486012789,
-0.266291346744262));
#54114=CARTESIAN_POINT('Ctrl Pts',(-0.0856552238532882,-0.0304914755703219,
-0.2607345797017));
#54115=CARTESIAN_POINT('Ctrl Pts',(-0.0208390447430576,-0.0885001789264252,
-0.25517781265914));
#54116=CARTESIAN_POINT('Ctrl Pts',(0.0630505469713957,-0.0655070681867248,
-0.249621045616578));
#54117=CARTESIAN_POINT('Ctrl Pts',(0.0892316826536689,0.0174428858451625,
-0.244064278574018));
#54118=CARTESIAN_POINT('Ctrl Pts',(0.0337414787132595,0.0844278394254827,
-0.238507511531456));
#54119=CARTESIAN_POINT('Ctrl Pts',(-0.0526313857957924,0.0741382808340391,
-0.232950744488896));
#54120=CARTESIAN_POINT('Ctrl Pts',(-0.090832169981939,-0.00400803595100973,
-0.227393977446334));
#54121=CARTESIAN_POINT('Ctrl Pts',(-0.0458967318909284,-0.078485906107687,
-0.221837210403773));
#54122=CARTESIAN_POINT('Ctrl Pts',(0.0410467404134879,-0.0811277545433131,
-0.216280443361212));
#54123=CARTESIAN_POINT('Ctrl Pts',(0.0904212441966549,-0.00951556901827846,
-0.210723676318651));
#54124=CARTESIAN_POINT('Ctrl Pts',(0.0570356349317089,0.0708059588152648,
-0.20516690927609));
#54125=CARTESIAN_POINT('Ctrl Pts',(-0.0285531444693586,0.086320712443328,
-0.199610142233528));
#54126=CARTESIAN_POINT('Ctrl Pts',(-0.0880080049539633,0.0228284585515061,
-0.194053375190968));
#54127=CARTESIAN_POINT('Ctrl Pts',(-0.066911524834458,-0.0615580644606202,
-0.188496608148406));
#54128=CARTESIAN_POINT('Ctrl Pts',(0.0154272596650918,-0.0896021602141092,
-0.182939841105846));
#54129=CARTESIAN_POINT('Ctrl Pts',(0.0836458917022921,-0.0356358282793559,
-0.177383074063284));
#54130=CARTESIAN_POINT('Ctrl Pts',(0.0753057071160328,0.0509470110168211,
-0.171826307020724));
#54131=CARTESIAN_POINT('Ctrl Pts',(-0.00195974928453672,0.0908994325534489,
-0.166269539978162));
#54132=CARTESIAN_POINT('Ctrl Pts',(-0.0774315003044271,0.0476540682053071,
-0.160712772935601));
#54133=CARTESIAN_POINT('Ctrl Pts',(-0.0820322986429512,-0.0392077726352661,
-0.15515600589304));
#54134=CARTESIAN_POINT('Ctrl Pts',(-0.0115511583366739,-0.0901838022975522,
-0.149599238850479));
#54135=CARTESIAN_POINT('Ctrl Pts',(0.0695024439932433,-0.0586170430456018,
-0.144042471807918));
#54136=CARTESIAN_POINT('Ctrl Pts',(0.0869423438765829,0.0266003063128576,
-0.138485704765357));
#54137=CARTESIAN_POINT('Ctrl Pts',(0.0248062738692927,0.0874711165618063,
-0.132928937722796));
#54138=CARTESIAN_POINT('Ctrl Pts',(-0.060034306037044,0.06828198560688,
-0.127372170680234));
#54139=CARTESIAN_POINT('Ctrl Pts',(-0.0899271133647523,-0.0134037953370005,
-0.121815403637674));
#54140=CARTESIAN_POINT('Ctrl Pts',(-0.0375120723642829,-0.0828214458067399,
-0.116258636595112));
#54141=CARTESIAN_POINT('Ctrl Pts',(0.0492367516523744,-0.0764348727121444,
-0.110701869552552));
#54142=CARTESIAN_POINT('Ctrl Pts',(0.0909205113292806,-8.95329878673978E-5,
-0.10514510250999));
#54143=CARTESIAN_POINT('Ctrl Pts',(0.0493871934324411,0.0763377535454949,
-0.0995883354674292));
#54144=CARTESIAN_POINT('Ctrl Pts',(-0.0373488856504812,0.0828951647330362,
-0.0940315684248683));
#54145=CARTESIAN_POINT('Ctrl Pts',(-0.0899005383010079,0.013580878233047,
-0.0884748013823069));
#54146=CARTESIAN_POINT('Ctrl Pts',(-0.0601686736797739,-0.0681636157774126,
-0.0829180343397461));
#54147=CARTESIAN_POINT('Ctrl Pts',(0.0246339612574005,-0.0875198044834496,
-0.0773612672971848));
#54148=CARTESIAN_POINT('Ctrl Pts',(0.0868897714115783,-0.0267714817211423,
-0.0718045002546238));
#54149=CARTESIAN_POINT('Ctrl Pts',(0.0696177828677645,0.0584800381028195,
-0.0662477332120627));
#54150=CARTESIAN_POINT('Ctrl Pts',(-0.0113735752523172,0.0902063917492059,
-0.0606909661695015));
#54151=CARTESIAN_POINT('Ctrl Pts',(-0.0819548176299329,0.0393692297513722,
-0.0551341991269405));
#54152=CARTESIAN_POINT('Ctrl Pts',(-0.0775253991606801,-0.0475014236531102,
-0.0495774320843793));
#54153=CARTESIAN_POINT('Ctrl Pts',(-0.00213839956732174,-0.0908954960444865,
-0.0440206650418183));
#54154=CARTESIAN_POINT('Ctrl Pts',(0.0752045198915063,-0.0510950366031558,
-0.0384638979992572));
#54155=CARTESIAN_POINT('Ctrl Pts',(0.0837172445451427,0.0354706629272246,
-0.0329071309566961));
#54156=CARTESIAN_POINT('Ctrl Pts',(0.0156011758647249,0.0895722804600428,
-0.0273503639141351));
#54157=CARTESIAN_POINT('Ctrl Pts',(-0.0667853739006856,0.0616884410865223,
-0.0217935968715739));
#54158=CARTESIAN_POINT('Ctrl Pts',(-0.0880618651332911,-0.0226526480487904,
-0.0162368298290128));
#54159=CARTESIAN_POINT('Ctrl Pts',(-0.0287058857600831,-0.0862689353105569,
-0.0106800627864517));
#54160=CARTESIAN_POINT('Ctrl Pts',(0.0568633264954318,-0.0709093305807852,
-0.00512329574389066));
#54161=CARTESIAN_POINT('Ctrl Pts',(0.0905029064835577,0.00932029688342027,
0.000433471298670411));
#54162=CARTESIAN_POINT('Ctrl Pts',(0.0410783200919443,0.0810830116111529,
0.00599023834123158));
#54163=CARTESIAN_POINT('Ctrl Pts',(-0.0165949764526702,0.0793494655732392,
0.00969474970293892));
#54164=CARTESIAN_POINT('Ctrl Pts',(-0.0387009125009883,0.0664807866724729,
0.0115470053837926));
#54165=CARTESIAN_POINT('',(0.0769008389612107,0.00192784648297797,0.));
#54166=CARTESIAN_POINT('Ctrl Pts',(0.0770242870977014,0.00196088950922314,
-1.56125112837913E-17));
#54167=CARTESIAN_POINT('Ctrl Pts',(0.0767355444305697,0.00393482941033669,
-2.03122860241009E-17));
#54168=CARTESIAN_POINT('Ctrl Pts',(0.0763650804585085,0.00589328886515121,
4.04310519118361E-17));
#54169=CARTESIAN_POINT('Ctrl Pts',(0.0759106818058855,0.00783195085873916,
3.12250225675825E-17));
#54170=CARTESIAN_POINT('Ctrl Pts',(0.0749514899506794,0.011924279881973,
1.18503374704373E-17));
#54171=CARTESIAN_POINT('Ctrl Pts',(0.0736187376959688,0.0159288611658458,
-4.04200893462907E-17));
#54172=CARTESIAN_POINT('Ctrl Pts',(0.0719425060131334,0.0198063602908007,
-8.67361737988404E-18));
#54173=CARTESIAN_POINT('Ctrl Pts',(0.070871047943992,0.0222848826621795,
1.16189316176618E-17));
#54174=CARTESIAN_POINT('Ctrl Pts',(0.0696591442633312,0.0247101164831124,
2.15812243806632E-17));
#54175=CARTESIAN_POINT('Ctrl Pts',(0.0683207983996043,0.0270604039630841,
1.90819582357449E-17));
#54176=CARTESIAN_POINT('Ctrl Pts',(0.0667211506419413,0.0298695672736282,
1.60947293042127E-17));
#54177=CARTESIAN_POINT('Ctrl Pts',(0.0649390499018336,0.032576338574731,
-1.48038691071277E-16));
#54178=CARTESIAN_POINT('Ctrl Pts',(0.06298781283264,0.0351614966284854,
-1.6306400674182E-16));
#54179=CARTESIAN_POINT('Ctrl Pts',(0.0610180171756984,0.0377712426133224,
-1.78232231054124E-16));
#54180=CARTESIAN_POINT('Ctrl Pts',(0.0588721823446311,0.0402598580152677,
-6.31405163010684E-17));
#54181=CARTESIAN_POINT('Ctrl Pts',(0.0565835086679188,0.0425851086778113,
-3.46944695195361E-17));
#54182=CARTESIAN_POINT('Ctrl Pts',(0.0526077988759246,0.0466243572268643,
1.47198388126686E-17));
#54183=CARTESIAN_POINT('Ctrl Pts',(0.0481933888539555,0.0501870891976839,
-4.56922916309108E-18));
#54184=CARTESIAN_POINT('Ctrl Pts',(0.0434112988581259,0.0531552124976776,
5.20417042793042E-18));
#54185=CARTESIAN_POINT('Ctrl Pts',(0.0406871449609811,0.054846026485272,
1.07716617565028E-17));
#54186=CARTESIAN_POINT('Ctrl Pts',(0.0378378243539425,0.0563447142077944,
-1.15248730856744E-16));
#54187=CARTESIAN_POINT('Ctrl Pts',(0.0349064264744822,0.0576115805932702,
-8.15320033709099E-17));
#54188=CARTESIAN_POINT('Ctrl Pts',(0.0333579064157681,0.0582808067066427,
-6.37210370766907E-17));
#54189=CARTESIAN_POINT('Ctrl Pts',(0.0317852908376245,0.0588862744051351,
-6.38585590855274E-17));
#54190=CARTESIAN_POINT('Ctrl Pts',(0.0301905740463167,0.0594245974561285,
-6.33174068731535E-17));
#54191=CARTESIAN_POINT('Ctrl Pts',(0.0271332970740427,0.0604566319066448,
-6.31473102947789E-17));
#54192=CARTESIAN_POINT('Ctrl Pts',(0.0239946807002247,0.0612421909225445,
1.57144674071977E-16));
#54193=CARTESIAN_POINT('Ctrl Pts',(0.0208030260208049,0.0617831377165539,
1.62196645003831E-16));
#54194=CARTESIAN_POINT('Ctrl Pts',(0.0186151991120485,0.0621539478670914,
1.65659688176464E-16));
#54195=CARTESIAN_POINT('Ctrl Pts',(0.0164005708805104,0.062409806097221,
-6.83477658214862E-17));
#54196=CARTESIAN_POINT('Ctrl Pts',(0.0141748740344104,0.0625496135305,-5.8113236445223E-17));
#54197=CARTESIAN_POINT('Ctrl Pts',(0.00874673157748686,0.0628905829961777,
-3.31527466411991E-17));
#54198=CARTESIAN_POINT('Ctrl Pts',(0.00329440124118755,0.0625432479469995,
1.08495009030099E-16));
#54199=CARTESIAN_POINT('Ctrl Pts',(-0.0020407491023474,0.0615174160184291,
1.04950770296597E-16));
#54200=CARTESIAN_POINT('Ctrl Pts',(-0.0041885001110211,0.061104450793937,
1.0352397970501E-16));
#54201=CARTESIAN_POINT('Ctrl Pts',(-0.00631700386563472,0.0605810109679865,
-2.68752568833808E-17));
#54202=CARTESIAN_POINT('Ctrl Pts',(-0.0084154806475312,0.0599458611255486,
-3.07913416985883E-17));
#54203=CARTESIAN_POINT('Ctrl Pts',(-0.0105364069326447,0.0593039164505187,
-3.47493207865443E-17));
#54204=CARTESIAN_POINT('Ctrl Pts',(-0.0126184161606321,0.0585501961183772,
-1.85078928243005E-17));
#54205=CARTESIAN_POINT('Ctrl Pts',(-0.0146468443017921,0.0576869532301707,
-2.64545330086463E-17));
#54206=CARTESIAN_POINT('Ctrl Pts',(-0.0192232633510667,0.0557393559169726,
-4.43832704282387E-17));
#54207=CARTESIAN_POINT('Ctrl Pts',(-0.0235379545271893,0.0532336481116517,
-3.79989797786901E-17));
#54208=CARTESIAN_POINT('Ctrl Pts',(-0.0274528972419724,0.0501564562137779,
-2.07624716030974E-17));
#54209=CARTESIAN_POINT('Ctrl Pts',(-0.027852503585005,0.0498423608385185,
-1.90031053746486E-17));
#54210=CARTESIAN_POINT('Ctrl Pts',(-0.028247905322877,0.0495222895177995,
-1.23650236939171E-18));
#54211=CARTESIAN_POINT('Ctrl Pts',(-0.0286389268003753,0.0491962142519396,
0.));
#54212=CARTESIAN_POINT('Ctrl Pts',(-0.0769126606442387,-6.94072219677582E-5,
-0.0176396170927523));
#54213=CARTESIAN_POINT('Ctrl Pts',(-0.076971024511457,-0.0065279364822696,
-0.0171720213381724));
#54214=CARTESIAN_POINT('Ctrl Pts',(-0.0762252932793503,-0.0129732902276908,
-0.0167044255835926));
#54215=CARTESIAN_POINT('Ctrl Pts',(-0.074623120032322,-0.0191985144031997,
-0.0162368298290128));
#54216=CARTESIAN_POINT('Ctrl Pts',(-0.0682765386755549,-0.043858077136046,
-0.0143845741481591));
#54217=CARTESIAN_POINT('Ctrl Pts',(-0.0484912122178188,-0.0650635062233016,
-0.0125323184673054));
#54218=CARTESIAN_POINT('Ctrl Pts',(-0.0243370136130319,-0.0731062866453006,
-0.0106800627864517));
#54219=CARTESIAN_POINT('Ctrl Pts',(-0.000182815008244568,-0.0811490670672997,
-0.00882780710559804));
#54220=CARTESIAN_POINT('Ctrl Pts',(0.0283402557435934,-0.0760291988240425,
-0.00697555142474438));
#54221=CARTESIAN_POINT('Ctrl Pts',(0.0482083877842003,-0.0600976601250463,
-0.00512329574389069));
#54222=CARTESIAN_POINT('Ctrl Pts',(0.0665266501016693,-0.0454089060734496,
-0.00341553049592711));
#54223=CARTESIAN_POINT('Ctrl Pts',(0.0774876123484423,-0.0215294799140155,
-0.00170776524796349));
#54224=CARTESIAN_POINT('Ctrl Pts',(0.0770242870977013,0.00196088950922531,
1.00613961606655E-16));
#54225=CARTESIAN_POINT('',(-0.0213030042343889,0.0527886127454549,-0.5608));
#54226=CARTESIAN_POINT('Ctrl Pts',(-0.0213168644878943,0.0528821598543764,
-0.5608));
#54227=CARTESIAN_POINT('Ctrl Pts',(-0.0200400288559082,0.0536782786774046,
-0.5608));
#54228=CARTESIAN_POINT('Ctrl Pts',(-0.0187323017072707,0.0544185816222459,
-0.5608));
#54229=CARTESIAN_POINT('Ctrl Pts',(-0.0173965430020956,0.0551003306193025,
-0.5608));
#54230=CARTESIAN_POINT('Ctrl Pts',(-0.0144915803430684,0.0565829751804841,
-0.5608));
#54231=CARTESIAN_POINT('Ctrl Pts',(-0.0114545109907711,0.0577892023762642,
-0.5608));
#54232=CARTESIAN_POINT('Ctrl Pts',(-0.00832330515556293,0.0587308479779915,
-0.5608));
#54233=CARTESIAN_POINT('Ctrl Pts',(-0.00621786685346983,0.059364015141447,
-0.5608));
#54234=CARTESIAN_POINT('Ctrl Pts',(-0.00407091670421551,0.0598766588631911,
-0.5608));
#54235=CARTESIAN_POINT('Ctrl Pts',(-0.00190319110591001,0.0602702142526908,
-0.5608));
#54236=CARTESIAN_POINT('Ctrl Pts',(0.00195266903242079,0.060970254211523,
-0.5608));
#54237=CARTESIAN_POINT('Ctrl Pts',(0.00588166571401474,0.061296842042279,
-0.5608));
#54238=CARTESIAN_POINT('Ctrl Pts',(0.00982578190433832,0.0612640784166091,
-0.5608));
#54239=CARTESIAN_POINT('Ctrl Pts',(0.0120694902474667,0.0612454400153249,
-0.5608));
#54240=CARTESIAN_POINT('Ctrl Pts',(0.0143086737138421,0.0611103104399024,
-0.5608));
#54241=CARTESIAN_POINT('Ctrl Pts',(0.0165324227803292,0.0608624325775255,
-0.5608));
#54242=CARTESIAN_POINT('Ctrl Pts',(0.020213063703421,0.0604521572375861,
-0.5608));
#54243=CARTESIAN_POINT('Ctrl Pts',(0.023851531624229,0.0597335279680504,
-0.5608));
#54244=CARTESIAN_POINT('Ctrl Pts',(0.027403304404835,0.0587159243115919,
-0.5608));
#54245=CARTESIAN_POINT('Ctrl Pts',(0.029552326701873,0.0581002168656603,
-0.5608));
#54246=CARTESIAN_POINT('Ctrl Pts',(0.0316696966121409,0.0573748722106627,
-0.5608));
#54247=CARTESIAN_POINT('Ctrl Pts',(0.0337457330178675,0.0565401986057516,
-0.5608));
#54248=CARTESIAN_POINT('Ctrl Pts',(0.0357573291778275,0.0557314332999855,
-0.5608));
#54249=CARTESIAN_POINT('Ctrl Pts',(0.0377218002147095,0.0548232331313804,
-0.5608));
#54250=CARTESIAN_POINT('Ctrl Pts',(0.0396284595471832,0.0538189834925058,
-0.5608));
#54251=CARTESIAN_POINT('Ctrl Pts',(0.0407788604385921,0.0532130600010453,
-0.5608));
#54252=CARTESIAN_POINT('Ctrl Pts',(0.0419084909952876,0.0525720444311966,
-0.5608));
#54253=CARTESIAN_POINT('Ctrl Pts',(0.0430155335449313,0.0518963074449715,
-0.5608));
#54254=CARTESIAN_POINT('Ctrl Pts',(0.0469905641944571,0.0494699551497256,
-0.5608));
#54255=CARTESIAN_POINT('Ctrl Pts',(0.0506750453636331,0.0465978050955386,
-0.5608));
#54256=CARTESIAN_POINT('Ctrl Pts',(0.0540463165810115,0.0433542137292111,
-0.5608));
#54257=CARTESIAN_POINT('Ctrl Pts',(0.05564618250959,0.0418149393787913,
-0.5608));
#54258=CARTESIAN_POINT('Ctrl Pts',(0.0571743672102615,0.0401920536871288,
-0.5608));
#54259=CARTESIAN_POINT('Ctrl Pts',(0.0586198127704844,0.0385033456845963,
-0.5608));
#54260=CARTESIAN_POINT('Ctrl Pts',(0.0616266630685766,0.0349904550572784,
-0.5608));
#54261=CARTESIAN_POINT('Ctrl Pts',(0.0642868952611629,0.0311838839229392,
-0.5608));
#54262=CARTESIAN_POINT('Ctrl Pts',(0.0665797585803528,0.027151816035101,
-0.5608));
#54263=CARTESIAN_POINT('Ctrl Pts',(0.0678796009979006,0.0248660047409082,
-0.5608));
#54264=CARTESIAN_POINT('Ctrl Pts',(0.0690612345731456,0.0225073874127262,
-0.5608));
#54265=CARTESIAN_POINT('Ctrl Pts',(0.0701192745487128,0.0200863361487867,
-0.5608));
#54266=CARTESIAN_POINT('Ctrl Pts',(0.071030260471914,0.0180017801095736,
-0.5608));
#54267=CARTESIAN_POINT('Ctrl Pts',(0.0718473902749254,0.0158753395167728,
-0.5608));
#54268=CARTESIAN_POINT('Ctrl Pts',(0.0725655572330888,0.0137219177577617,
-0.5608));
#54269=CARTESIAN_POINT('Ctrl Pts',(0.0745600844141832,0.00774133318493183,
-0.5608));
#54270=CARTESIAN_POINT('Ctrl Pts',(0.0758018690746804,0.00153804309463624,
-0.5608));
#54271=CARTESIAN_POINT('Ctrl Pts',(0.0762248566852573,-0.00474661219965071,
-0.5608));
#54272=CARTESIAN_POINT('Ctrl Pts',(0.0763222229870443,-0.00619325893045234,
-0.5608));
#54273=CARTESIAN_POINT('Ctrl Pts',(0.0763760168749407,-0.00764432619612087,
-0.5608));
#54274=CARTESIAN_POINT('Ctrl Pts',(0.0763850617480247,-0.00909823976109944,
-0.5608));
#54275=CARTESIAN_POINT('Ctrl Pts',(-0.0213168644878947,0.0528821598543762,
-0.5608));
#54276=CARTESIAN_POINT('Ctrl Pts',(-0.0374049180327334,0.0462896122782152,
-0.559092234752037));
#54277=CARTESIAN_POINT('Ctrl Pts',(-0.0541768854252427,0.02761762516725,
-0.556887775577551));
#54278=CARTESIAN_POINT('Ctrl Pts',(-0.0569445161760761,0.00512363730287358,
-0.554683316403066));
#54279=CARTESIAN_POINT('Ctrl Pts',(-0.0569002140125902,4.52833130624442E-5,
-0.554186622476545));
#54280=CARTESIAN_POINT('Origin',(-8.56069748352724E-18,0.,-0.5608));
#54281=CARTESIAN_POINT('Ctrl Pts',(0.0402076065502267,-0.0657262044767394,
-0.5608));
#54282=CARTESIAN_POINT('Ctrl Pts',(0.0383936167831799,-0.066556416417856,
-0.5608));
#54283=CARTESIAN_POINT('Ctrl Pts',(0.0365482166471986,-0.0673096127760332,
-0.5608));
#54284=CARTESIAN_POINT('Ctrl Pts',(0.0346738275063863,-0.0679815896617125,
-0.5608));
#54285=CARTESIAN_POINT('Ctrl Pts',(0.0307171719732606,-0.0694000683569653,
-0.5608));
#54286=CARTESIAN_POINT('Ctrl Pts',(0.0266311929689044,-0.0704572681754979,
-0.5608));
#54287=CARTESIAN_POINT('Ctrl Pts',(0.0224652565211834,-0.0711570679346724,
-0.5608));
#54288=CARTESIAN_POINT('Ctrl Pts',(0.0198023631532829,-0.0716043844410448,
-0.5608));
#54289=CARTESIAN_POINT('Ctrl Pts',(0.0171078889170027,-0.0719048428903344,
-0.5608));
#54290=CARTESIAN_POINT('Ctrl Pts',(0.0144076243887813,-0.0720584304502345,
-0.5608));
#54291=CARTESIAN_POINT('Ctrl Pts',(0.0111801511265865,-0.0722420049622138,
-0.5608));
#54292=CARTESIAN_POINT('Ctrl Pts',(0.00793949242691801,-0.0722167745237351,
-0.5608));
#54293=CARTESIAN_POINT('Ctrl Pts',(0.00470902027438889,-0.0719834737466585,
-0.5608));
#54294=CARTESIAN_POINT('Ctrl Pts',(0.0014478283809384,-0.0717479544271862,
-0.5608));
#54295=CARTESIAN_POINT('Ctrl Pts',(-0.00180733306330198,-0.0712988329734778,
-0.5608));
#54296=CARTESIAN_POINT('Ctrl Pts',(-0.00500296882198629,-0.0706410311799038,
-0.5608));
#54297=CARTESIAN_POINT('Ctrl Pts',(-0.0105541900807911,-0.0694983467263818,
-0.5608));
#54298=CARTESIAN_POINT('Ctrl Pts',(-0.0159437658000986,-0.0677284487236317,
-0.5608));
#54299=CARTESIAN_POINT('Ctrl Pts',(-0.0210339685484103,-0.0653267882248462,
-0.5608));
#54300=CARTESIAN_POINT('Ctrl Pts',(-0.0239336398211533,-0.0639586647335923,
-0.5608));
#54301=CARTESIAN_POINT('Ctrl Pts',(-0.0267400378694071,-0.0623810675864798,
-0.5608));
#54302=CARTESIAN_POINT('Ctrl Pts',(-0.0293964253216744,-0.0606086000260937,
-0.5608));
#54303=CARTESIAN_POINT('Ctrl Pts',(-0.0307996708239191,-0.0596722881451354,
-0.5608));
#54304=CARTESIAN_POINT('Ctrl Pts',(-0.0321624853084298,-0.0586811031556425,
-0.5608));
#54305=CARTESIAN_POINT('Ctrl Pts',(-0.033480942421694,-0.0576348792224091,
-0.5608));
#54306=CARTESIAN_POINT('Ctrl Pts',(-0.0360085918225298,-0.0556291353333036,
-0.5608));
#54307=CARTESIAN_POINT('Ctrl Pts',(-0.0383735280098577,-0.0534211778677626,
-0.5608));
#54308=CARTESIAN_POINT('Ctrl Pts',(-0.040561936721919,-0.0510357775345927,
-0.5608));
#54309=CARTESIAN_POINT('Ctrl Pts',(-0.0420620578929242,-0.0494006215779431,
-0.5608));
#54310=CARTESIAN_POINT('Ctrl Pts',(-0.0434802420446818,-0.0476805031262554,
-0.5608));
#54311=CARTESIAN_POINT('Ctrl Pts',(-0.0448070177436098,-0.0458880324564179,
-0.5608));
#54312=CARTESIAN_POINT('Ctrl Pts',(-0.0480428217484688,-0.0415164692926221,
-0.5608));
#54313=CARTESIAN_POINT('Ctrl Pts',(-0.0507139486815803,-0.0367505873557775,
-0.5608));
#54314=CARTESIAN_POINT('Ctrl Pts',(-0.0527518145139489,-0.0317143920503034,
-0.5608));
#54315=CARTESIAN_POINT('Ctrl Pts',(-0.0535721880095819,-0.0296869959961479,
-0.5608));
#54316=CARTESIAN_POINT('Ctrl Pts',(-0.0542893617667917,-0.0276157278638674,
-0.5608));
#54317=CARTESIAN_POINT('Ctrl Pts',(-0.0548964411856249,-0.0255089656800579,
-0.5608));
#54318=CARTESIAN_POINT('Ctrl Pts',(-0.0555100186045104,-0.0233796533317132,
-0.5608));
#54319=CARTESIAN_POINT('Ctrl Pts',(-0.0560086146086451,-0.0212222738601327,
-0.5608));
#54320=CARTESIAN_POINT('Ctrl Pts',(-0.0563861523156285,-0.0190503620714463,
-0.5608));
#54321=CARTESIAN_POINT('Ctrl Pts',(-0.0572379279437924,-0.0141502382059215,
-0.5608));
#54322=CARTESIAN_POINT('Ctrl Pts',(-0.0574789598668102,-0.00916656265595418,
-0.5608));
#54323=CARTESIAN_POINT('Ctrl Pts',(-0.0570230227323766,-0.00420793446946095,
-0.5608));
#54324=CARTESIAN_POINT('Ctrl Pts',(-0.0569764839929469,-0.00370179384683607,
-0.5608));
#54325=CARTESIAN_POINT('Ctrl Pts',(-0.0569226437332971,-0.00319593569578702,
-0.5608));
#54326=CARTESIAN_POINT('Ctrl Pts',(-0.0568613829974075,-0.00269049226390578,
-0.5608));
#54327=CARTESIAN_POINT('Origin',(0.,0.,-0.5608));
#54328=CARTESIAN_POINT('Origin',(0.,0.,-0.648563377523455));
#54329=CARTESIAN_POINT('Ctrl Pts',(-0.0768390318326848,-0.00363576842162011,
-0.572347005383793));
#54330=CARTESIAN_POINT('Ctrl Pts',(-0.0756300800702637,-0.0291859883983543,
-0.570494749702939));
#54331=CARTESIAN_POINT('Ctrl Pts',(-0.0457466014776253,-0.0785438038026859,
-0.566790238341232));
#54332=CARTESIAN_POINT('Ctrl Pts',(0.0413535491490546,-0.0810402774590353,
-0.56123347129867));
#54333=CARTESIAN_POINT('Ctrl Pts',(0.0904258996703788,-0.00920489789578024,
-0.55567670425611));
#54334=CARTESIAN_POINT('Ctrl Pts',(0.0568231075837852,0.070975286479318,
-0.550119937213548));
#54335=CARTESIAN_POINT('Ctrl Pts',(-0.0288348405916419,0.0862356444712252,
-0.544563170170988));
#54336=CARTESIAN_POINT('Ctrl Pts',(-0.0880765772585221,0.0225447831988859,
-0.539006403128426));
#54337=CARTESIAN_POINT('Ctrl Pts',(-0.0667171067556589,-0.0617690697919249,
-0.533449636085865));
#54338=CARTESIAN_POINT('Ctrl Pts',(0.0157135236534292,-0.0895535055615975,
-0.527892869043304));
#54339=CARTESIAN_POINT('Ctrl Pts',(0.0837584047019811,-0.0353688086955708,
-0.522336102000743));
#54340=CARTESIAN_POINT('Ctrl Pts',(0.0751433811500897,0.0511862922340276,
-0.516779334958182));
#54341=CARTESIAN_POINT('Ctrl Pts',(-0.00224933968455702,0.0908928684440432,
-0.511222567915621));
#54342=CARTESIAN_POINT('Ctrl Pts',(-0.0775827744759656,0.0474071916605113,
-0.50566580087306));
#54343=CARTESIAN_POINT('Ctrl Pts',(-0.0819070771081818,-0.039468751630768,
-0.500109033830498));
#54344=CARTESIAN_POINT('Ctrl Pts',(-0.0112639065077944,-0.0902201489166854,
-0.494552266787938));
#54345=CARTESIAN_POINT('Ctrl Pts',(0.0696887350471192,-0.0583954204966491,
-0.488995499745376));
#54346=CARTESIAN_POINT('Ctrl Pts',(0.0868572077657704,0.0268770161445482,
-0.483438732702816));
#54347=CARTESIAN_POINT('Ctrl Pts',(0.0245276118500181,0.087549668072802,
-0.477881965660254));
#54348=CARTESIAN_POINT('Ctrl Pts',(-0.060251430791017,0.0680904724858967,
-0.472325198617693));
#54349=CARTESIAN_POINT('Ctrl Pts',(-0.0898839785216628,-0.0136900809031243,
-0.466768431575132));
#54350=CARTESIAN_POINT('Ctrl Pts',(-0.0372481547545244,-0.0829404772933564,
-0.461211664532571));
#54351=CARTESIAN_POINT('Ctrl Pts',(0.0494798934149131,-0.076277702240305,
-0.455654897490009));
#54352=CARTESIAN_POINT('Ctrl Pts',(0.0909203376627111,0.000199984617355618,
-0.450098130447449));
#54353=CARTESIAN_POINT('Ctrl Pts',(0.049143861682941,0.0764946313950189,
-0.444541363404887));
#54354=CARTESIAN_POINT('Ctrl Pts',(-0.0376126581190482,0.0827758159825542,
-0.438984596362327));
#54355=CARTESIAN_POINT('Ctrl Pts',(-0.0899433319377845,0.0132945407773614,
-0.433427829319765));
#54356=CARTESIAN_POINT('Ctrl Pts',(-0.0599513127724785,-0.0683548671821957,
-0.427871062277205));
#54357=CARTESIAN_POINT('Ctrl Pts',(0.0249125173624084,-0.0874409186145301,
-0.422314295234643));
#54358=CARTESIAN_POINT('Ctrl Pts',(0.0869745958753753,-0.0264946682098307,
-0.416757528192082));
#54359=CARTESIAN_POINT('Ctrl Pts',(0.0694311850831299,0.0587014336154286,
-0.411200761149521));
#54360=CARTESIAN_POINT('Ctrl Pts',(-0.0116607067891965,0.090169704932605,
-0.40564399410696));
#54361=CARTESIAN_POINT('Ctrl Pts',(-0.0820798699193133,0.0391080902720935,
-0.400087227064399));
#54362=CARTESIAN_POINT('Ctrl Pts',(-0.077373553700188,-0.0477480990029214,
-0.394530460021838));
#54363=CARTESIAN_POINT('Ctrl Pts',(-0.00184932175801734,-0.0909017479459029,
-0.388973692979277));
#54364=CARTESIAN_POINT('Ctrl Pts',(0.0753675442454562,-0.0508554917882798,
-0.383416925936715));
#54365=CARTESIAN_POINT('Ctrl Pts',(0.0836025405860219,0.0357374170605961,
-0.377860158894155));
#54366=CARTESIAN_POINT('Ctrl Pts',(0.0153183984047813,0.0896208370911247,
-0.372303391851593));
#54367=CARTESIAN_POINT('Ctrl Pts',(-0.0669862584792194,0.0614767349943143,
-0.366746624809033));
#54368=CARTESIAN_POINT('Ctrl Pts',(-0.0879802093044121,-0.0229353557058732,
-0.361189857766471));
#54369=CARTESIAN_POINT('Ctrl Pts',(-0.0284482601299106,-0.0863553372188681,
-0.35563309072391));
#54370=CARTESIAN_POINT('Ctrl Pts',(0.0571216101691189,-0.0707366200937766,
-0.350076323681349));
#54371=CARTESIAN_POINT('Ctrl Pts',(0.0904096195284211,0.00962540738513244,
-0.344519556638788));
#54372=CARTESIAN_POINT('Ctrl Pts',(0.0409481555832509,0.0811775604766097,
-0.338962789596227));
#54373=CARTESIAN_POINT('Ctrl Pts',(-0.045992044861177,0.0784300935871637,
-0.333406022553666));
#54374=CARTESIAN_POINT('Ctrl Pts',(-0.0908369737149324,0.00389768866334984,
-0.327849255511104));
#54375=CARTESIAN_POINT('Ctrl Pts',(-0.0525412835649756,-0.0742021650084995,
-0.322292488468544));
#54376=CARTESIAN_POINT('Ctrl Pts',(0.0338440187791357,-0.0843867890340737,
-0.316735721425982));
#54377=CARTESIAN_POINT('Ctrl Pts',(0.0892528084126734,-0.0173344731980629,
-0.311178954383422));
#54378=CARTESIAN_POINT('Ctrl Pts',(0.0629709225891355,0.0655836159332256,
-0.30562218734086));
#54379=CARTESIAN_POINT('Ctrl Pts',(-0.020946541228509,0.0884747996955411,
-0.300065420298299));
#54380=CARTESIAN_POINT('Ctrl Pts',(-0.0856922038235555,0.0303873982839258,
-0.294508653255739));
#54381=CARTESIAN_POINT('Ctrl Pts',(-0.0720061157964265,-0.0555127648249965,
-0.288951886213176));
#54382=CARTESIAN_POINT('Ctrl Pts',(0.00758521757887318,-0.0906035995139536,
-0.283395119170616));
#54383=CARTESIAN_POINT('Ctrl Pts',(0.080234006976822,-0.0427674162774302,
-0.277838352128054));
#54384=CARTESIAN_POINT('Ctrl Pts',(0.0794467853278221,0.0442126234426178,
-0.272281585085494));
#54385=CARTESIAN_POINT('Ctrl Pts',(0.00594407526174785,0.0907260477475264,
-0.266724818042932));
#54386=CARTESIAN_POINT('Ctrl Pts',(-0.0729990857182597,0.0542003805789396,
-0.261168051000372));
#54387=CARTESIAN_POINT('Ctrl Pts',(-0.0851281629049463,-0.031933425294394,
-0.25561128395781));
#54388=CARTESIAN_POINT('Ctrl Pts',(-0.019341740828334,-0.0888394328681432,
-0.250054516915249));
#54389=CARTESIAN_POINT('Ctrl Pts',(0.0641476521786357,-0.064433116412079,
-0.244497749872688));
#54390=CARTESIAN_POINT('Ctrl Pts',(0.0889244385051616,0.0189470843969588,
-0.238940982830127));
#54391=CARTESIAN_POINT('Ctrl Pts',(0.0323110974472321,0.0849855326061983,
-0.233384215787566));
#54392=CARTESIAN_POINT('Ctrl Pts',(-0.0538757149912223,0.0732390271971729,
-0.227827448745005));
#54393=CARTESIAN_POINT('Ctrl Pts',(-0.0907515463340875,-0.00554117393482795,
-0.222270681702444));
#54394=CARTESIAN_POINT('Ctrl Pts',(-0.0445649480385644,-0.0792496888127868,
-0.216713914659883));
#54395=CARTESIAN_POINT('Ctrl Pts',(0.0424107388215024,-0.0804231123696258,
-0.211157147617321));
#54396=CARTESIAN_POINT('Ctrl Pts',(0.0905690264021953,-0.0079874418410624,
-0.20560038057476));
#54397=CARTESIAN_POINT('Ctrl Pts',(0.0558319398891111,0.0717589176257572,
-0.200043613532199));
#54398=CARTESIAN_POINT('Ctrl Pts',(-0.0300066073256354,0.0858262855272531,
-0.194486846489638));
#54399=CARTESIAN_POINT('Ctrl Pts',(-0.088380920482232,0.0213391814588081,
-0.188930079447077));
#54400=CARTESIAN_POINT('Ctrl Pts',(-0.0658625735630241,-0.0626790967886454,
-0.183373312404516));
#54401=CARTESIAN_POINT('Ctrl Pts',(0.0169380010792513,-0.089328897284294,
-0.177816545361955));
#54402=CARTESIAN_POINT('Ctrl Pts',(0.0842356826073205,-0.0342183802419164,
-0.172259778319394));
#54403=CARTESIAN_POINT('Ctrl Pts',(0.0744347278870117,0.052211292407325,
-0.166703011276833));
#54404=CARTESIAN_POINT('Ctrl Pts',(-0.00349431497263191,0.0908533848209656,
-0.161146244234271));
#54405=CARTESIAN_POINT('Ctrl Pts',(-0.0782251060929565,0.0463398375912083,
-0.155589477191711));
#54406=CARTESIAN_POINT('Ctrl Pts',(-0.0813585786607769,-0.0405873064859364,
-0.150032710149149));
#54407=CARTESIAN_POINT('Ctrl Pts',(-0.0100267502373365,-0.0903659894557529,
-0.144475943106589));
#54408=CARTESIAN_POINT('Ctrl Pts',(0.0704822908518116,-0.0574351325482238,
-0.138919176064027));
#54409=CARTESIAN_POINT('Ctrl Pts',(0.0864808021551291,0.0280645438402883,
-0.133362409021466));
#54410=CARTESIAN_POINT('Ctrl Pts',(0.0233257803388205,0.0878775042030495,
-0.127805641978905));
#54411=CARTESIAN_POINT('Ctrl Pts',(-0.0611786960722008,0.0672585677921695,
-0.122248874936344));
#54412=CARTESIAN_POINT('Ctrl Pts',(-0.0896879702034033,-0.0149203120679575,
-0.116692107893783));
#54413=CARTESIAN_POINT('Ctrl Pts',(-0.0361082782663861,-0.0834430347416967,
-0.111135340851222));
#54414=CARTESIAN_POINT('Ctrl Pts',(0.0505203439252101,-0.0755926104834019,
-0.105578573808661));
#54415=CARTESIAN_POINT('Ctrl Pts',(0.0909090609484884,0.00144568087120341,
-0.1000218067661));
#54416=CARTESIAN_POINT('Ctrl Pts',(0.0480911874950899,0.0771607789491207,
-0.0944650397235385));
#54417=CARTESIAN_POINT('Ctrl Pts',(-0.0387432610833752,0.0822527097324212,
-0.0889082726809775));
#54418=CARTESIAN_POINT('Ctrl Pts',(-0.0901170244962536,0.0120609627886696,
-0.0833515056384163));
#54419=CARTESIAN_POINT('Ctrl Pts',(-0.0590091735361575,-0.069169851083726,
-0.0777947385958553));
#54420=CARTESIAN_POINT('Ctrl Pts',(0.0261082775077724,-0.087091385804074,
-0.0722379715532941));
#54421=CARTESIAN_POINT('Ctrl Pts',(0.0873293337077548,-0.025300517597168,
-0.0666812045107331));
#54422=CARTESIAN_POINT('Ctrl Pts',(0.068620590974884,0.0596471923669532,
-0.0611244374681719));
#54423=CARTESIAN_POINT('Ctrl Pts',(-0.0128954238312897,0.0900015126958784,
-0.055567670425611));
#54424=CARTESIAN_POINT('Ctrl Pts',(-0.0826072687683161,0.0379797595227237,
-0.0500109033830497));
#54425=CARTESIAN_POINT('Ctrl Pts',(-0.0767134573427241,-0.0488035925573516,
-0.0444541363404888));
#54426=CARTESIAN_POINT('Ctrl Pts',(-0.000601088932553975,-0.0909188044845557,
-0.0388973692979275));
#54427=CARTESIAN_POINT('Ctrl Pts',(0.076052321356028,-0.0498176186446183,
-0.0333406022553666));
#54428=CARTESIAN_POINT('Ctrl Pts',(0.0831143936316547,0.0368786114239041,
-0.0277838352128053));
#54429=CARTESIAN_POINT('Ctrl Pts',(0.0140713189020179,0.0898240214567205,
-0.0222270681702444));
#54430=CARTESIAN_POINT('Ctrl Pts',(-0.0677885288000042,0.0605498871972536,
-0.0166703011276831));
#54431=CARTESIAN_POINT('Ctrl Pts',(-0.0877227621557321,-0.0241321279134182,
-0.0111135340851222));
#54432=CARTESIAN_POINT('Ctrl Pts',(-0.0271300943677211,-0.0867515915827831,
-0.00555676704256098));
#54433=CARTESIAN_POINT('Ctrl Pts',(0.0294658500759831,-0.0755214844234609,
-0.00185225568085369));
#54434=CARTESIAN_POINT('Ctrl Pts',(0.0491442338326719,-0.0591802323922411,
0.));
#54435=CARTESIAN_POINT('Ctrl Pts',(-0.0701798155542591,-0.00332067636904823,
-0.568498003589195));
#54436=CARTESIAN_POINT('Ctrl Pts',(-0.0690756369919176,-0.0266565993052248,
-0.566645747908341));
#54437=CARTESIAN_POINT('Ctrl Pts',(-0.0417819951313892,-0.071736844313774,
-0.562941236546634));
#54438=CARTESIAN_POINT('Ctrl Pts',(0.037769664486587,-0.0740169623287969,
-0.557384469504073));
#54439=CARTESIAN_POINT('Ctrl Pts',(0.0825891842834973,-0.0084071600215922,
-0.551827702461512));
#54440=CARTESIAN_POINT('Ctrl Pts',(0.0518985613735119,0.0648242487603872,
-0.546270935418951));
#54441=CARTESIAN_POINT('Ctrl Pts',(-0.0263358835476263,0.0787620754562775,
-0.540714168376389));
#54442=CARTESIAN_POINT('Ctrl Pts',(-0.0804434647239304,0.0205909508341243,
-0.535157401333829));
#54443=CARTESIAN_POINT('Ctrl Pts',(-0.0609351020536189,-0.0564158842395974,
-0.529600634291267));
#54444=CARTESIAN_POINT('Ctrl Pts',(0.0143517189819161,-0.0817923957740036,
-0.524043867248707));
#54445=CARTESIAN_POINT('Ctrl Pts',(0.0764995244331497,-0.0323035885724571,
-0.518487100206145));
#54446=CARTESIAN_POINT('Ctrl Pts',(0.0686311175903372,0.0467502578079397,
-0.512930333163584));
#54447=CARTESIAN_POINT('Ctrl Pts',(-0.00205440178534356,0.0830156834418511,
-0.507373566121023));
#54448=CARTESIAN_POINT('Ctrl Pts',(-0.0708591021131913,0.0432986710962806,
-0.501816799078462));
#54449=CARTESIAN_POINT('Ctrl Pts',(-0.074808641219703,-0.0360482120029261,
-0.496260032035901));
#54450=CARTESIAN_POINT('Ctrl Pts',(-0.0102877256816388,-0.0824012648160085,
-0.49070326499334));
#54451=CARTESIAN_POINT('Ctrl Pts',(0.0636491956648538,-0.0533346105738538,
-0.485146497950778));
#54452=CARTESIAN_POINT('Ctrl Pts',(0.079329771278649,0.0245477329774338,
-0.479589730908218));
#54453=CARTESIAN_POINT('Ctrl Pts',(0.0224019386315129,0.0799622198593647,
-0.474032963865656));
#54454=CARTESIAN_POINT('Ctrl Pts',(-0.0550297706639658,0.0621894457294541,
-0.468476196823095));
#54455=CARTESIAN_POINT('Ctrl Pts',(-0.0820942284602035,-0.0125036368859546,
-0.462919429780535));
#54456=CARTESIAN_POINT('Ctrl Pts',(-0.0340200620447827,-0.0757524822944741,
-0.457362662737973));
#54457=CARTESIAN_POINT('Ctrl Pts',(0.0451917431893769,-0.0696671333103681,
-0.451805895695412));
#54458=CARTESIAN_POINT('Ctrl Pts',(0.0830407720544162,0.000182653050474542,
-0.446249128652851));
#54459=CARTESIAN_POINT('Ctrl Pts',(0.0448848334794573,0.0698652624083424,
-0.44069236161029));
#54460=CARTESIAN_POINT('Ctrl Pts',(-0.0343529759074532,0.0756020912738502,
-0.435135594567729));
#54461=CARTESIAN_POINT('Ctrl Pts',(-0.0821484380421907,0.012142376047441,
-0.429578827525167));
#54462=CARTESIAN_POINT('Ctrl Pts',(-0.0547556622234602,-0.0624309267915823,
-0.424022060482607));
#54463=CARTESIAN_POINT('Ctrl Pts',(0.0227534865001052,-0.0798628951185247,
-0.418465293440045));
#54464=CARTESIAN_POINT('Ctrl Pts',(0.0794369860064231,-0.0241985210353241,
-0.412908526397485));
#54465=CARTESIAN_POINT('Ctrl Pts',(0.0634139661397318,0.0536141032186852,
-0.407351759354923));
#54466=CARTESIAN_POINT('Ctrl Pts',(-0.0106501374650332,0.0823551925345891,
-0.401794992312362));
#54467=CARTESIAN_POINT('Ctrl Pts',(-0.0749664590282454,0.0357188071805889,
-0.396238225269801));
#54468=CARTESIAN_POINT('Ctrl Pts',(-0.0706680133513467,-0.0436100338742971,
-0.390681458227241));
#54469=CARTESIAN_POINT('Ctrl Pts',(-0.00168905121241881,-0.0830237934061215,
-0.385124691184679));
#54470=CARTESIAN_POINT('Ctrl Pts',(0.0688358537031139,-0.0464481260174393,
-0.379567924142118));
#54471=CARTESIAN_POINT('Ctrl Pts',(0.076357168202876,0.032640251677813,
-0.374011157099557));
#54472=CARTESIAN_POINT('Ctrl Pts',(0.0139908370653997,0.0818538920501867,
-0.368454390056996));
#54473=CARTESIAN_POINT('Ctrl Pts',(-0.0611809278776191,0.0561488844910692,
-0.362897623014435));
#54474=CARTESIAN_POINT('Ctrl Pts',(-0.0803554484503843,-0.0209476745700599,
-0.357340855971873));
#54475=CARTESIAN_POINT('Ctrl Pts',(-0.0259828058883404,-0.0788713950917863,
-0.351784088929313));
#54476=CARTESIAN_POINT('Ctrl Pts',(0.0521711943815237,-0.0646062662778276,
-0.346227321886752));
#54477=CARTESIAN_POINT('Ctrl Pts',(0.0825743150519032,0.00879122626628292,
-0.34067055484419));
#54478=CARTESIAN_POINT('Ctrl Pts',(0.0373994041514876,0.0741423477822878,
-0.33511378780163));
#54479=CARTESIAN_POINT('Ctrl Pts',(-0.0420061672868148,0.0716329887372305,
-0.329557020759068));
#54480=CARTESIAN_POINT('Ctrl Pts',(-0.0829646328014945,0.00355989742397316,
-0.324000253716507));
#54481=CARTESIAN_POINT('Ctrl Pts',(-0.0479878194926123,-0.0677714714751015,
-0.318443486673946));
#54482=CARTESIAN_POINT('Ctrl Pts',(0.0309109438118187,-0.0770734501512592,
-0.312886719631385));
#54483=CARTESIAN_POINT('Ctrl Pts',(0.081517758393159,-0.0158321897446498,
-0.307329952588824));
#54484=CARTESIAN_POINT('Ctrl Pts',(0.057513579064998,0.0598998446466287,
-0.301773185546262));
#54485=CARTESIAN_POINT('Ctrl Pts',(-0.0191312197050768,0.0808071754125344,
-0.296216418503702));
#54486=CARTESIAN_POINT('Ctrl Pts',(-0.0782657318206477,0.027753889603702,
-0.29065965146114));
#54487=CARTESIAN_POINT('Ctrl Pts',(-0.0657657417700864,-0.0507017788148143,
-0.28510288441858));
#54488=CARTESIAN_POINT('Ctrl Pts',(0.00692784848959868,-0.082751483858969,
-0.279546117376018));
#54489=CARTESIAN_POINT('Ctrl Pts',(0.0732805668748336,-0.0390609995271377,
-0.273989350333457));
#54490=CARTESIAN_POINT('Ctrl Pts',(0.0725615693964754,0.0403809585358808,
-0.268432583290896));
#54491=CARTESIAN_POINT('Ctrl Pts',(0.00542893495090355,0.0828633201775967,
-0.262875816248335));
#54492=CARTESIAN_POINT('Ctrl Pts',(-0.066672656450076,0.0495031316933198,
-0.257319049205774));
#54493=CARTESIAN_POINT('Ctrl Pts',(-0.0777505732262594,-0.029165930956239,
-0.251762282163213));
#54494=CARTESIAN_POINT('Ctrl Pts',(-0.0176654985292686,-0.08114020783353,
-0.246205515120651));
#54495=CARTESIAN_POINT('Ctrl Pts',(0.0585883279729262,-0.0588490525912939,
-0.240648748078091));
#54496=CARTESIAN_POINT('Ctrl Pts',(0.0812178464995143,0.017305044800213,
-0.235091981035529));
#54497=CARTESIAN_POINT('Ctrl Pts',(0.0295108723407657,0.0776203039110454,
-0.229535213992969));
#54498=CARTESIAN_POINT('Ctrl Pts',(-0.0492066030864478,0.0668918035206761,
-0.223978446950407));
#54499=CARTESIAN_POINT('Ctrl Pts',(-0.0828866089419013,-0.0050609508660535,
-0.218421679907846));
#54500=CARTESIAN_POINT('Ctrl Pts',(-0.0407027490968618,-0.0723815541523789,
-0.212864912865285));
#54501=CARTESIAN_POINT('Ctrl Pts',(0.0387352333446096,-0.0734532835433118,
-0.207308145822724));
#54502=CARTESIAN_POINT('Ctrl Pts',(0.0827199070086567,-0.00729521418719437,
-0.201751378780163));
#54503=CARTESIAN_POINT('Ctrl Pts',(0.0509932927315665,0.0655399669052933,
-0.196194611737602));
#54504=CARTESIAN_POINT('Ctrl Pts',(-0.0274060997034382,0.0783881934005274,
-0.190637844695041));
#54505=CARTESIAN_POINT('Ctrl Pts',(-0.0807214321943126,0.0194898319661148,
-0.18508107765248));
#54506=CARTESIAN_POINT('Ctrl Pts',(-0.0601546265529035,-0.0572470442016113,
-0.179524310609918));
#54507=CARTESIAN_POINT('Ctrl Pts',(0.0154700776838018,-0.0815872530607607,
-0.173967543567358));
#54508=CARTESIAN_POINT('Ctrl Pts',(0.0769354392874359,-0.0312528614255867,
-0.168410776524796));
#54509=CARTESIAN_POINT('Ctrl Pts',(0.0679838794080156,0.0476864268536628,
-0.162854009482235));
#54510=CARTESIAN_POINT('Ctrl Pts',(-0.0031914819124976,0.0829796216472279,
-0.157297242439674));
#54511=CARTESIAN_POINT('Ctrl Pts',(-0.0714457663817268,0.0423238187337744,
-0.151740475397113));
#54512=CARTESIAN_POINT('Ctrl Pts',(-0.0743076781160228,-0.0370698278607881,
-0.146183708354552));
#54513=CARTESIAN_POINT('Ctrl Pts',(-0.00915778694084917,-0.0825344661576702,
-0.140626941311991));
#54514=CARTESIAN_POINT('Ctrl Pts',(0.0643739783524676,-0.0524575455003868,
-0.13507017426943));
#54515=CARTESIAN_POINT('Ctrl Pts',(0.0789859866720714,0.0256323441791222,
-0.129513407226869));
#54516=CARTESIAN_POINT('Ctrl Pts',(0.0213042632473828,0.0802616442352845,
-0.123956640184308));
#54517=CARTESIAN_POINT('Ctrl Pts',(-0.0558766749631382,0.0614296376401015,
-0.118399873141747));
#54518=CARTESIAN_POINT('Ctrl Pts',(-0.0819152071048523,-0.0136272506819364,
-0.112843106099185));
#54519=CARTESIAN_POINT('Ctrl Pts',(-0.0329789723826125,-0.0762114858528055,
-0.107286339056624));
#54520=CARTESIAN_POINT('Ctrl Pts',(0.0461420235763678,-0.0690414146880683,
-0.101729572014063));
#54521=CARTESIAN_POINT('Ctrl Pts',(0.083030472630994,0.00132039166126336,
-0.096172804971502));
#54522=CARTESIAN_POINT('Ctrl Pts',(0.0439233887738163,0.0704736786177055,
-0.090616037928941));
#54523=CARTESIAN_POINT('Ctrl Pts',(-0.0353855957311171,0.0751243197653603,
-0.0850592708863799));
#54524=CARTESIAN_POINT('Ctrl Pts',(-0.0823070776219169,0.0110157054784169,
-0.0795025038438189));
#54525=CARTESIAN_POINT('Ctrl Pts',(-0.0538951730130365,-0.0631752805207342,
-0.0739457368012577));
#54526=CARTESIAN_POINT('Ctrl Pts',(0.0238456166902865,-0.0795436543943393,
-0.0683889697586967));
#54527=CARTESIAN_POINT('Ctrl Pts',(0.0797609806619091,-0.0231078608884972,
-0.0628322027161355));
#54528=CARTESIAN_POINT('Ctrl Pts',(0.0626736217646239,0.0544778982608371,
-0.0572754356735745));
#54529=CARTESIAN_POINT('Ctrl Pts',(-0.011777848371965,0.0822015765939713,
-0.0517186686310134));
#54530=CARTESIAN_POINT('Ctrl Pts',(-0.0754481511196702,0.0346882626515089,
-0.0461619015884522));
#54531=CARTESIAN_POINT('Ctrl Pts',(-0.07006512391469,-0.0445740536075221,
-0.0406051345458912));
#54532=CARTESIAN_POINT('Ctrl Pts',(-0.00054899586072548,-0.0830393717483792,
-0.0350483675033299));
#54533=CARTESIAN_POINT('Ctrl Pts',(0.0694612849477496,-0.0455001996308929,
-0.0294916004607691));
#54534=CARTESIAN_POINT('Ctrl Pts',(0.0759113262602619,0.0336825450021603,
-0.0239348334182077));
#54535=CARTESIAN_POINT('Ctrl Pts',(0.0128518350842712,0.0820394675443192,
-0.0183780663756468));
#54536=CARTESIAN_POINT('Ctrl Pts',(-0.0619136698421449,0.0553023614949671,
-0.0128212993330856));
#54537=CARTESIAN_POINT('Ctrl Pts',(-0.0801203128301351,-0.0220407291125593,
-0.00726453229052462));
#54538=CARTESIAN_POINT('Ctrl Pts',(-0.0247788783029195,-0.0792333082693582,
-0.00170776524796345));
#54539=CARTESIAN_POINT('Ctrl Pts',(0.0269122069104775,-0.068976452732553,
0.00199674611374385));
#54540=CARTESIAN_POINT('Ctrl Pts',(0.0448851733770188,-0.0540514071388779,
0.00384900179459754));
#54541=CARTESIAN_POINT('Ctrl Pts',(-0.0635205992758333,-0.00300558431647635,
-0.564649001794598));
#54542=CARTESIAN_POINT('Ctrl Pts',(-0.0625211939135715,-0.0241272102120953,
-0.562796746113744));
#54543=CARTESIAN_POINT('Ctrl Pts',(-0.0378173887851531,-0.0649298848248621,
-0.559092234752037));
#54544=CARTESIAN_POINT('Ctrl Pts',(0.0341857798241194,-0.0669936471985585,
-0.553535467709475));
#54545=CARTESIAN_POINT('Ctrl Pts',(0.0747524688966159,-0.00760942214740409,
-0.547978700666915));
#54546=CARTESIAN_POINT('Ctrl Pts',(0.0469740151632386,0.0586732110414563,
-0.542421933624353));
#54547=CARTESIAN_POINT('Ctrl Pts',(-0.0238369265036107,0.0712885064413299,
-0.536865166581792));
#54548=CARTESIAN_POINT('Ctrl Pts',(-0.0728103521893386,0.0186371184693627,
-0.531308399539231));
#54549=CARTESIAN_POINT('Ctrl Pts',(-0.0551530973515789,-0.0510626986872698,
-0.52575163249667));
#54550=CARTESIAN_POINT('Ctrl Pts',(0.012989914310403,-0.0740312859864097,
-0.520194865454109));
#54551=CARTESIAN_POINT('Ctrl Pts',(0.0692406441643183,-0.0292383684493435,
-0.514638098411548));
#54552=CARTESIAN_POINT('Ctrl Pts',(0.0621188540305847,0.0423142233818518,
-0.509081331368986));
#54553=CARTESIAN_POINT('Ctrl Pts',(-0.00185946388613005,0.0751384984396591,
-0.503524564326426));
#54554=CARTESIAN_POINT('Ctrl Pts',(-0.064135429750417,0.0391901505320498,
-0.497967797283864));
#54555=CARTESIAN_POINT('Ctrl Pts',(-0.0677102053312242,-0.0326276723750841,
-0.492411030241303));
#54556=CARTESIAN_POINT('Ctrl Pts',(-0.00931154485548331,-0.0745823807153317,
-0.486854263198743));
#54557=CARTESIAN_POINT('Ctrl Pts',(0.0576096562825884,-0.0482738006510584,
-0.481297496156181));
#54558=CARTESIAN_POINT('Ctrl Pts',(0.0718023347915276,0.0222184498103195,
-0.47574072911362));
#54559=CARTESIAN_POINT('Ctrl Pts',(0.0202762654130079,0.0723747716459273,
-0.470183962071059));
#54560=CARTESIAN_POINT('Ctrl Pts',(-0.0498081105369146,0.0562884189730116,
-0.464627195028498));
#54561=CARTESIAN_POINT('Ctrl Pts',(-0.0743044783987442,-0.0113171928687849,
-0.459070427985937));
#54562=CARTESIAN_POINT('Ctrl Pts',(-0.0307919693350411,-0.0685644872955918,
-0.453513660943375));
#54563=CARTESIAN_POINT('Ctrl Pts',(0.0409035929638406,-0.0630565643804312,
-0.447956893900815));
#54564=CARTESIAN_POINT('Ctrl Pts',(0.0751612064461215,0.000165321483593517,
-0.442400126858254));
#54565=CARTESIAN_POINT('Ctrl Pts',(0.0406258052759737,0.0632358934216658,
-0.436843359815692));
#54566=CARTESIAN_POINT('Ctrl Pts',(-0.0310932936958583,0.0684283665651463,
-0.431286592773132));
#54567=CARTESIAN_POINT('Ctrl Pts',(-0.0743535441465968,0.0109902113175206,
-0.42572982573057));
#54568=CARTESIAN_POINT('Ctrl Pts',(-0.049560011674442,-0.0565069864009689,
-0.42017305868801));
#54569=CARTESIAN_POINT('Ctrl Pts',(0.020594455637802,-0.0722848716225193,
-0.414616291645448));
#54570=CARTESIAN_POINT('Ctrl Pts',(0.0718993761374708,-0.0219023738608175,
-0.409059524602887));
#54571=CARTESIAN_POINT('Ctrl Pts',(0.0573967471963337,0.0485267728219418,
-0.403502757560326));
#54572=CARTESIAN_POINT('Ctrl Pts',(-0.00963956814086993,0.0745406801365732,
-0.397945990517764));
#54573=CARTESIAN_POINT('Ctrl Pts',(-0.0678530481371775,0.0323295240890841,
-0.392389223475204));
#54574=CARTESIAN_POINT('Ctrl Pts',(-0.0639624730025055,-0.0394719687456726,
-0.386832456432642));
#54575=CARTESIAN_POINT('Ctrl Pts',(-0.00152878066682028,-0.0751458388663401,
-0.381275689390082));
#54576=CARTESIAN_POINT('Ctrl Pts',(0.0623041631607716,-0.0420407602465988,
-0.375718922347521));
#54577=CARTESIAN_POINT('Ctrl Pts',(0.0691117958197301,0.0295430862950298,
-0.370162155304959));
#54578=CARTESIAN_POINT('Ctrl Pts',(0.0126632757260182,0.0740869470092486,
-0.364605388262398));
#54579=CARTESIAN_POINT('Ctrl Pts',(-0.0553755972760191,0.0508210339878241,
-0.359048621219837));
#54580=CARTESIAN_POINT('Ctrl Pts',(-0.0727306875963563,-0.0189599934342466,
-0.353491854177276));
#54581=CARTESIAN_POINT('Ctrl Pts',(-0.0235173516467703,-0.0713874529647044,
-0.347935087134715));
#54582=CARTESIAN_POINT('Ctrl Pts',(0.0472207785939286,-0.0584759124618787,
-0.342378320092153));
#54583=CARTESIAN_POINT('Ctrl Pts',(0.0747390105753852,0.00795704514743341,
-0.336821553049593));
#54584=CARTESIAN_POINT('Ctrl Pts',(0.0338506527197245,0.0671071350879659,
-0.331264786007032));
#54585=CARTESIAN_POINT('Ctrl Pts',(-0.0380202897124528,0.0648358838872972,
-0.325708018964471));
#54586=CARTESIAN_POINT('Ctrl Pts',(-0.0750922918880565,0.00322210618459649,
-0.320151251921909));
#54587=CARTESIAN_POINT('Ctrl Pts',(-0.043434355420249,-0.0613407779417036,
-0.314594484879349));
#54588=CARTESIAN_POINT('Ctrl Pts',(0.0279778688445018,-0.0697601112684447,
-0.309037717836787));
#54589=CARTESIAN_POINT('Ctrl Pts',(0.0737827083736445,-0.0143299062912367,
-0.303480950794226));
#54590=CARTESIAN_POINT('Ctrl Pts',(0.0520562355408607,0.0542160733600317,
-0.297924183751665));
#54591=CARTESIAN_POINT('Ctrl Pts',(-0.0173158981816449,0.0731395511295278,
-0.292367416709104));
#54592=CARTESIAN_POINT('Ctrl Pts',(-0.0708392598177398,0.0251203809234781,
-0.286810649666543));
#54593=CARTESIAN_POINT('Ctrl Pts',(-0.0595253677437465,-0.045890792804632,
-0.281253882623981));
#54594=CARTESIAN_POINT('Ctrl Pts',(0.00627047940032424,-0.0748993682039843,
-0.275697115581421));
#54595=CARTESIAN_POINT('Ctrl Pts',(0.0663271267728453,-0.0353545827768454,
-0.27014034853886));
#54596=CARTESIAN_POINT('Ctrl Pts',(0.0656763534651288,0.0365492936291439,
-0.264583581496299));
#54597=CARTESIAN_POINT('Ctrl Pts',(0.00491379464005916,0.075000592607667,
-0.259026814453737));
#54598=CARTESIAN_POINT('Ctrl Pts',(-0.0603462271818922,0.0448058828077,
-0.253470047411177));
#54599=CARTESIAN_POINT('Ctrl Pts',(-0.0703729835475725,-0.0263984366180838,
-0.247913280368615));
#54600=CARTESIAN_POINT('Ctrl Pts',(-0.0159892562302031,-0.073440982798917,
-0.242356513326054));
#54601=CARTESIAN_POINT('Ctrl Pts',(0.0530290037672167,-0.0532649887705087,
-0.236799746283493));
#54602=CARTESIAN_POINT('Ctrl Pts',(0.073511254493867,0.0156630052034671,
-0.231242979240932));
#54603=CARTESIAN_POINT('Ctrl Pts',(0.0267106472342993,0.0702550752158925,
-0.225686212198371));
#54604=CARTESIAN_POINT('Ctrl Pts',(-0.0445374911816733,0.0605445798441793,
-0.22012944515581));
#54605=CARTESIAN_POINT('Ctrl Pts',(-0.0750216715497152,-0.00458072779727913,
-0.214572678113249));
#54606=CARTESIAN_POINT('Ctrl Pts',(-0.0368405501551592,-0.0655134194919708,
-0.209015911070687));
#54607=CARTESIAN_POINT('Ctrl Pts',(0.0350597278677169,-0.066483454716998,
-0.203459144028127));
#54608=CARTESIAN_POINT('Ctrl Pts',(0.074870787615118,-0.00660298653332633,
-0.197902376985565));
#54609=CARTESIAN_POINT('Ctrl Pts',(0.0461546455740219,0.0593210161848294,
-0.192345609943004));
#54610=CARTESIAN_POINT('Ctrl Pts',(-0.0248055920812409,0.0709501012738018,
-0.186788842900443));
#54611=CARTESIAN_POINT('Ctrl Pts',(-0.0730619439063931,0.0176404824734215,
-0.181232075857882));
#54612=CARTESIAN_POINT('Ctrl Pts',(-0.0544466795427829,-0.0518149916145772,
-0.175675308815321));
#54613=CARTESIAN_POINT('Ctrl Pts',(0.0140021542883522,-0.0738456088372273,
-0.17011854177276));
#54614=CARTESIAN_POINT('Ctrl Pts',(0.0696351959675514,-0.0282873426092572,
-0.164561774730199));
#54615=CARTESIAN_POINT('Ctrl Pts',(0.0615330309290195,0.0431615613000007,
-0.159005007687638));
#54616=CARTESIAN_POINT('Ctrl Pts',(-0.00288864885236336,0.0751058584734902,
-0.153448240645077));
#54617=CARTESIAN_POINT('Ctrl Pts',(-0.0646664266704969,0.0383077998763405,
-0.147891473602516));
#54618=CARTESIAN_POINT('Ctrl Pts',(-0.0672567775712689,-0.0335523492356398,
-0.142334706559954));
#54619=CARTESIAN_POINT('Ctrl Pts',(-0.00828882364436172,-0.0747029428595875,
-0.136777939517393));
#54620=CARTESIAN_POINT('Ctrl Pts',(0.0582656658531234,-0.0474799584525497,
-0.131221172474832));
#54621=CARTESIAN_POINT('Ctrl Pts',(0.0714911711890138,0.023200144517956,
-0.125664405432271));
#54622=CARTESIAN_POINT('Ctrl Pts',(0.019282746155945,0.0726457842675196,
-0.12010763838971));
#54623=CARTESIAN_POINT('Ctrl Pts',(-0.0505746538540758,0.0556007074880334,
-0.114550871347149));
#54624=CARTESIAN_POINT('Ctrl Pts',(-0.0741424440063013,-0.0123341892959154,
-0.108994104304588));
#54625=CARTESIAN_POINT('Ctrl Pts',(-0.0298496664988389,-0.0689799369639143,
-0.103437337262027));
#54626=CARTESIAN_POINT('Ctrl Pts',(0.0417637032275256,-0.0624902188927347,
-0.0978805702194657));
#54627=CARTESIAN_POINT('Ctrl Pts',(0.0751518843134995,0.00119510245132327,
-0.0923238031769045));
#54628=CARTESIAN_POINT('Ctrl Pts',(0.0397555900525427,0.0637865782862904,
-0.0867670361343434));
#54629=CARTESIAN_POINT('Ctrl Pts',(-0.032027930378859,0.0679959297982993,
-0.0812102690917824));
#54630=CARTESIAN_POINT('Ctrl Pts',(-0.0744971307475801,0.00997044816816438,
-0.0756535020492212));
#54631=CARTESIAN_POINT('Ctrl Pts',(-0.0487811724899154,-0.0571807099577425,
-0.0700967350066602));
#54632=CARTESIAN_POINT('Ctrl Pts',(0.0215829558728007,-0.0719959229846046,
-0.064539967964099));
#54633=CARTESIAN_POINT('Ctrl Pts',(0.0721926276160632,-0.0209152041798264,
-0.058983200921538));
#54634=CARTESIAN_POINT('Ctrl Pts',(0.0567266525543639,0.0493086041547209,
-0.0534264338789769));
#54635=CARTESIAN_POINT('Ctrl Pts',(-0.0106602729126405,0.0744016404920643,
-0.0478696668364159));
#54636=CARTESIAN_POINT('Ctrl Pts',(-0.0682890334710242,0.031396765780294,
-0.0423128997938546));
#54637=CARTESIAN_POINT('Ctrl Pts',(-0.063416790486656,-0.0403445146576926,
-0.0367561327512936));
#54638=CARTESIAN_POINT('Ctrl Pts',(-0.000496902788896909,-0.0751599390122028,
-0.0311993657087325));
#54639=CARTESIAN_POINT('Ctrl Pts',(0.062870248539471,-0.0411827806171674,
-0.0256425986661715));
#54640=CARTESIAN_POINT('Ctrl Pts',(0.0687082588888692,0.0304864785804164,
-0.0200858316236103));
#54641=CARTESIAN_POINT('Ctrl Pts',(0.0116323512665244,0.074254913631918,
-0.0145290645810492));
#54642=CARTESIAN_POINT('Ctrl Pts',(-0.0560388108842856,0.0500548357926805,
-0.0089722975384881));
#54643=CARTESIAN_POINT('Ctrl Pts',(-0.0725178635045378,-0.0199493303117004,
-0.00341553049592708));
#54644=CARTESIAN_POINT('Ctrl Pts',(-0.0224276622381181,-0.0717150249559334,
0.00214123654663408));
#54645=CARTESIAN_POINT('Ctrl Pts',(0.0243585637449721,-0.0624314210416452,
0.00584574790834138));
#54646=CARTESIAN_POINT('Ctrl Pts',(0.0406261129213658,-0.0489225818855146,
0.00769800358919507));
#54647=CARTESIAN_POINT('Ctrl Pts',(-0.0568613829974076,-0.00269049226390446,
-0.5608));
#54648=CARTESIAN_POINT('Ctrl Pts',(-0.0559667508352254,-0.0215978211189658,
-0.558947744319147));
#54649=CARTESIAN_POINT('Ctrl Pts',(-0.033852782438917,-0.0581229253359501,
-0.555243232957439));
#54650=CARTESIAN_POINT('Ctrl Pts',(0.0306018951616518,-0.0599703320683201,
-0.549686465914878));
#54651=CARTESIAN_POINT('Ctrl Pts',(0.0669157535097345,-0.00681168427321597,
-0.544129698872316));
#54652=CARTESIAN_POINT('Ctrl Pts',(0.0420494689529653,0.0525221733225254,
-0.538572931829757));
#54653=CARTESIAN_POINT('Ctrl Pts',(-0.0213379694595951,0.0638149374263822,
-0.533016164787193));
#54654=CARTESIAN_POINT('Ctrl Pts',(-0.0651772396547469,0.0166832861046011,
-0.527459397744635));
#54655=CARTESIAN_POINT('Ctrl Pts',(-0.0493710926495389,-0.0457095131349423,
-0.521902630702072));
#54656=CARTESIAN_POINT('Ctrl Pts',(0.0116281096388898,-0.0662701761988158,
-0.516345863659512));
#54657=CARTESIAN_POINT('Ctrl Pts',(0.061981763895487,-0.0261731483262298,
-0.51078909661695));
#54658=CARTESIAN_POINT('Ctrl Pts',(0.0556065904708322,0.0378781889557639,
-0.505232329574389));
#54659=CARTESIAN_POINT('Ctrl Pts',(-0.00166452598691655,0.0672613134374671,
-0.499675562531828));
#54660=CARTESIAN_POINT('Ctrl Pts',(-0.0574117573876428,0.035081629967819,
-0.494118795489267));
#54661=CARTESIAN_POINT('Ctrl Pts',(-0.0606117694427453,-0.0292071327472421,
-0.488562028446706));
#54662=CARTESIAN_POINT('Ctrl Pts',(-0.00833536402932787,-0.066763496614655,
-0.483005261404145));
#54663=CARTESIAN_POINT('Ctrl Pts',(0.0515701169003231,-0.0432129907282631,
-0.477448494361583));
#54664=CARTESIAN_POINT('Ctrl Pts',(0.064274898304406,0.019889166643205,
-0.471891727319023));
#54665=CARTESIAN_POINT('Ctrl Pts',(0.0181505921945029,0.06478732343249,
-0.466334960276461));
#54666=CARTESIAN_POINT('Ctrl Pts',(-0.0445864504098636,0.050387392216569,
-0.4607781932339));
#54667=CARTESIAN_POINT('Ctrl Pts',(-0.0665147283372848,-0.0101307488516152,
-0.45522142619134));
#54668=CARTESIAN_POINT('Ctrl Pts',(-0.0275638766252995,-0.0613764922967096,
-0.449664659148778));
#54669=CARTESIAN_POINT('Ctrl Pts',(0.0366154427383043,-0.0564459954504943,
-0.444107892106218));
#54670=CARTESIAN_POINT('Ctrl Pts',(0.0672816408378267,0.000147989916712509,
-0.438551125063656));
#54671=CARTESIAN_POINT('Ctrl Pts',(0.03636677707249,0.0566065244349891,
-0.432994358021095));
#54672=CARTESIAN_POINT('Ctrl Pts',(-0.0278336114842633,0.0612546418564424,
-0.427437590978534));
#54673=CARTESIAN_POINT('Ctrl Pts',(-0.0665586502510029,0.00983804658760028,
-0.421880823935972));
#54674=CARTESIAN_POINT('Ctrl Pts',(-0.0443643611254238,-0.0505830460103554,
-0.416324056893412));
#54675=CARTESIAN_POINT('Ctrl Pts',(0.0184354247754988,-0.0647068481265139,
-0.41076728985085));
#54676=CARTESIAN_POINT('Ctrl Pts',(0.0643617662685185,-0.0196062266863109,
-0.40521052280829));
#54677=CARTESIAN_POINT('Ctrl Pts',(0.0513795282529356,0.0434394424251984,
-0.399653755765729));
#54678=CARTESIAN_POINT('Ctrl Pts',(-0.00862899881670666,0.0667261677385573,
-0.394096988723167));
#54679=CARTESIAN_POINT('Ctrl Pts',(-0.0607396372461095,0.0289402409975793,
-0.388540221680607));
#54680=CARTESIAN_POINT('Ctrl Pts',(-0.0572569326536643,-0.0353339036170481,
-0.382983454638045));
#54681=CARTESIAN_POINT('Ctrl Pts',(-0.00136851012122178,-0.0672678843265587,
-0.377426687595484));
#54682=CARTESIAN_POINT('Ctrl Pts',(0.0557724726184293,-0.0376333944757582,
-0.371869920552923));
#54683=CARTESIAN_POINT('Ctrl Pts',(0.0618664234365842,0.0264459209122466,
-0.366313153510362));
#54684=CARTESIAN_POINT('Ctrl Pts',(0.0113357143866367,0.0663200019683107,
-0.360756386467801));
#54685=CARTESIAN_POINT('Ctrl Pts',(-0.0495702666744188,0.0454931834845789,
-0.35519961942524));
#54686=CARTESIAN_POINT('Ctrl Pts',(-0.0651059267423285,-0.0169723122984332,
-0.349642852382678));
#54687=CARTESIAN_POINT('Ctrl Pts',(-0.0210518974052001,-0.0639035108376226,
-0.344086085340117));
#54688=CARTESIAN_POINT('Ctrl Pts',(0.0422703628063335,-0.0523455586459296,
-0.338529318297556));
#54689=CARTESIAN_POINT('Ctrl Pts',(0.0669037060988672,0.00712286402858384,
-0.332972551254995));
#54690=CARTESIAN_POINT('Ctrl Pts',(0.0303019012879613,0.0600719223936441,
-0.327415784212435));
#54691=CARTESIAN_POINT('Ctrl Pts',(-0.0340344121380907,0.0580387790373639,
-0.321859017169872));
#54692=CARTESIAN_POINT('Ctrl Pts',(-0.0672199509746185,0.00288431494521986,
-0.316302250127312));
#54693=CARTESIAN_POINT('Ctrl Pts',(-0.0388808913478858,-0.0549100844083057,
-0.310745483084751));
#54694=CARTESIAN_POINT('Ctrl Pts',(0.0250447938771848,-0.0624467723856301,
-0.30518871604219));
#54695=CARTESIAN_POINT('Ctrl Pts',(0.0660476583541301,-0.0128276228378236,
-0.299631948999629));
#54696=CARTESIAN_POINT('Ctrl Pts',(0.0465988920167232,0.0485323020734347,
-0.294075181957067));
#54697=CARTESIAN_POINT('Ctrl Pts',(-0.0155005766582128,0.0654719268465212,
-0.288518414914507));
#54698=CARTESIAN_POINT('Ctrl Pts',(-0.0634127878148319,0.0224868722432543,
-0.282961647871945));
#54699=CARTESIAN_POINT('Ctrl Pts',(-0.0532849937174065,-0.0410798067944498,
-0.277404880829384));
#54700=CARTESIAN_POINT('Ctrl Pts',(0.0056131103110498,-0.0670472525489997,
-0.271848113786823));
#54701=CARTESIAN_POINT('Ctrl Pts',(0.0593736866708568,-0.0316481660265529,
-0.266291346744262));
#54702=CARTESIAN_POINT('Ctrl Pts',(0.0587911375337822,0.0327176287224069,
-0.2607345797017));
#54703=CARTESIAN_POINT('Ctrl Pts',(0.00439865432921479,0.0671378650377374,
-0.25517781265914));
#54704=CARTESIAN_POINT('Ctrl Pts',(-0.0540197979137084,0.0401086339220801,
-0.249621045616579));
#54705=CARTESIAN_POINT('Ctrl Pts',(-0.0629953938688856,-0.0236309422799287,
-0.244064278574018));
#54706=CARTESIAN_POINT('Ctrl Pts',(-0.0143130139311376,-0.0657417577643039,
-0.238507511531456));
#54707=CARTESIAN_POINT('Ctrl Pts',(0.0474696795615072,-0.0476809249497236,
-0.232950744488896));
#54708=CARTESIAN_POINT('Ctrl Pts',(0.0658046624882197,0.0140209656067212,
-0.227393977446334));
#54709=CARTESIAN_POINT('Ctrl Pts',(0.0239104221278329,0.0628898465207396,
-0.221837210403774));
#54710=CARTESIAN_POINT('Ctrl Pts',(-0.0398683792768989,0.0541973561676825,
-0.216280443361212));
#54711=CARTESIAN_POINT('Ctrl Pts',(-0.0671567341575291,-0.00410050472850469,
-0.210723676318652));
#54712=CARTESIAN_POINT('Ctrl Pts',(-0.0329783512134566,-0.0586452848315629,
-0.20516690927609));
#54713=CARTESIAN_POINT('Ctrl Pts',(0.0313842223908242,-0.059513625890684,
-0.199610142233529));
#54714=CARTESIAN_POINT('Ctrl Pts',(0.0670216682215793,-0.00591075887945832,
-0.194053375190967));
#54715=CARTESIAN_POINT('Ctrl Pts',(0.0413159984164774,0.0531020654643655,
-0.188496608148407));
#54716=CARTESIAN_POINT('Ctrl Pts',(-0.0222050844590437,0.0635120091470762,
-0.182939841105846));
#54717=CARTESIAN_POINT('Ctrl Pts',(-0.0654024556184737,0.0157911329807281,
-0.177383074063285));
#54718=CARTESIAN_POINT('Ctrl Pts',(-0.0487387325326623,-0.046382939027543,
-0.171826307020724));
#54719=CARTESIAN_POINT('Ctrl Pts',(0.0125342308929026,-0.066103964613694,
-0.166269539978162));
#54720=CARTESIAN_POINT('Ctrl Pts',(0.0623349526476669,-0.0253218237929275,
-0.160712772935602));
#54721=CARTESIAN_POINT('Ctrl Pts',(0.0550821824500234,0.0386366957463386,
-0.15515600589304));
#54722=CARTESIAN_POINT('Ctrl Pts',(-0.00258581579222903,0.0672320952997525,
-0.149599238850479));
#54723=CARTESIAN_POINT('Ctrl Pts',(-0.0578870869592672,0.0342917810189067,
-0.144042471807918));
#54724=CARTESIAN_POINT('Ctrl Pts',(-0.0602058770265148,-0.0300348706104915,
-0.138485704765357));
#54725=CARTESIAN_POINT('Ctrl Pts',(-0.00741986034787437,-0.0668714195615047,
-0.132928937722796));
#54726=CARTESIAN_POINT('Ctrl Pts',(0.0521573533537793,-0.0425023714047127,
-0.127372170680235));
#54727=CARTESIAN_POINT('Ctrl Pts',(0.0639963557059561,0.0207679448567898,
-0.121815403637674));
#54728=CARTESIAN_POINT('Ctrl Pts',(0.0172612290645072,0.0650299242997547,
-0.116258636595113));
#54729=CARTESIAN_POINT('Ctrl Pts',(-0.0452726327450133,0.0497717773359655,
-0.110701869552551));
#54730=CARTESIAN_POINT('Ctrl Pts',(-0.0663696809077504,-0.0110411279098944,
-0.10514510250999));
#54731=CARTESIAN_POINT('Ctrl Pts',(-0.0267203606150653,-0.061748388075023,
-0.0995883354674292));
#54732=CARTESIAN_POINT('Ctrl Pts',(0.0373853828786833,-0.055939023097401,
-0.0940315684248681));
#54733=CARTESIAN_POINT('Ctrl Pts',(0.0672732959960052,0.00106981324138322,
-0.088474801382307));
#54734=CARTESIAN_POINT('Ctrl Pts',(0.035587791331269,0.0570994779548752,
-0.0829180343397459));
#54735=CARTESIAN_POINT('Ctrl Pts',(-0.0286702650266008,0.0608675398312384,
-0.0773612672971849));
#54736=CARTESIAN_POINT('Ctrl Pts',(-0.0666871838732434,0.00892519085791185,
-0.0718045002546237));
#54737=CARTESIAN_POINT('Ctrl Pts',(-0.0436671719667944,-0.0511861393947508,
-0.0662477332120627));
#54738=CARTESIAN_POINT('Ctrl Pts',(0.0193202950553148,-0.0644481915748698,
-0.0606909661695014));
#54739=CARTESIAN_POINT('Ctrl Pts',(0.0646242745702175,-0.0187225474711557,
-0.0551341991269405));
#54740=CARTESIAN_POINT('Ctrl Pts',(0.0507796833441037,0.0441393100486048,
-0.0495774320843793));
#54741=CARTESIAN_POINT('Ctrl Pts',(-0.00954269745331579,0.0666017043901573,
-0.0440206650418183));
#54742=CARTESIAN_POINT('Ctrl Pts',(-0.0611299158223783,0.0281052689090792,
-0.0384638979992571));
#54743=CARTESIAN_POINT('Ctrl Pts',(-0.0567684570586219,-0.036114975707863,
-0.0329071309566961));
#54744=CARTESIAN_POINT('Ctrl Pts',(-0.000444809717068389,-0.0672805062760264,
-0.0273503639141349));
#54745=CARTESIAN_POINT('Ctrl Pts',(0.0562792121311924,-0.036865361603442,
-0.021793596871574));
#54746=CARTESIAN_POINT('Ctrl Pts',(0.0615051915174765,0.0272904121586725,
-0.0162368298290127));
#54747=CARTESIAN_POINT('Ctrl Pts',(0.0104128674487777,0.0664703597195168,
-0.0106800627864517));
#54748=CARTESIAN_POINT('Ctrl Pts',(-0.0501639519264263,0.044807310090394,
-0.00512329574389055));
#54749=CARTESIAN_POINT('Ctrl Pts',(-0.0649154141789406,-0.0178579315108415,
0.00043347129867045));
#54750=CARTESIAN_POINT('Ctrl Pts',(-0.0200764461733167,-0.0641967416425085,
0.00599023834123162));
#54751=CARTESIAN_POINT('Ctrl Pts',(0.0218049205794665,-0.0558863893507373,
0.00969474970293892));
#54752=CARTESIAN_POINT('Ctrl Pts',(0.0363670524657127,-0.0437937566321514,
0.0115470053837926));
#54753=CARTESIAN_POINT('',(0.0491442338326711,-0.0591802323922418,0.));
#54754=CARTESIAN_POINT('Ctrl Pts',(-0.05597698479429,-0.0108401358572846,
1.04083408558608E-17));
#54755=CARTESIAN_POINT('Ctrl Pts',(-0.0559515023807956,-0.0123446174890954,
1.17559405793022E-17));
#54756=CARTESIAN_POINT('Ctrl Pts',(-0.0558623774955055,-0.0138447025863335,
3.0034649799714E-17));
#54757=CARTESIAN_POINT('Ctrl Pts',(-0.055708865632993,-0.0153365024293318,
4.68375338513738E-17));
#54758=CARTESIAN_POINT('Ctrl Pts',(-0.0553750133694311,-0.0185808168830483,
8.34714469153916E-17));
#54759=CARTESIAN_POINT('Ctrl Pts',(-0.0547373288205537,-0.0217858319569694,
3.70891418926431E-17));
#54760=CARTESIAN_POINT('Ctrl Pts',(-0.0538263802290202,-0.0249261037145957,
4.5102810375397E-17));
#54761=CARTESIAN_POINT('Ctrl Pts',(-0.0532138536290939,-0.0270376388774144,
5.04912429985968E-17));
#54762=CARTESIAN_POINT('Ctrl Pts',(-0.0524775926510349,-0.0291185320549929,
-1.9163422263778E-17));
#54763=CARTESIAN_POINT('Ctrl Pts',(-0.0516300698525238,-0.0311521551872357,
-1.21430643318376E-17));
#54764=CARTESIAN_POINT('Ctrl Pts',(-0.0501225335147105,-0.0347694747149932,
3.44440081553474E-19));
#54765=CARTESIAN_POINT('Ctrl Pts',(-0.0482617497084152,-0.0382452636414351,
1.86132677700906E-16));
#54766=CARTESIAN_POINT('Ctrl Pts',(-0.0460910809893396,-0.0415384799097066,
1.2490009027033E-16));
#54767=CARTESIAN_POINT('Ctrl Pts',(-0.0448562377753026,-0.0434119144534002,
9.00662879484486E-17));
#54768=CARTESIAN_POINT('Ctrl Pts',(-0.0435260602506697,-0.0452182508027399,
8.80667632144303E-17));
#54769=CARTESIAN_POINT('Ctrl Pts',(-0.0421096187004071,-0.046950364248589,
9.36750677027476E-17));
#54770=CARTESIAN_POINT('Ctrl Pts',(-0.0397651997051909,-0.0498172666375831,
1.02957636101656E-16));
#54771=CARTESIAN_POINT('Ctrl Pts',(-0.0371848385423227,-0.0524812110416646,
9.99035557290718E-17));
#54772=CARTESIAN_POINT('Ctrl Pts',(-0.0344006017048867,-0.0549099186113641,
1.37910516340156E-16));
#54773=CARTESIAN_POINT('Ctrl Pts',(-0.0327159861626315,-0.0563794195045698,
1.60906805915247E-16));
#54774=CARTESIAN_POINT('Ctrl Pts',(-0.030956531645651,-0.0577627741542382,
6.77527425510591E-17));
#54775=CARTESIAN_POINT('Ctrl Pts',(-0.0291277574335744,-0.0590520230017192,
8.41340885848751E-17));
#54776=CARTESIAN_POINT('Ctrl Pts',(-0.0273557380977418,-0.0603012608088524,
1.00007049679358E-16));
#54777=CARTESIAN_POINT('Ctrl Pts',(-0.0255258512225868,-0.0614569060963195,
-2.78362784928054E-17));
#54778=CARTESIAN_POINT('Ctrl Pts',(-0.0236467459224507,-0.0625118270565618,
-8.67361737988404E-19));
#54779=CARTESIAN_POINT('Ctrl Pts',(-0.0225129729697565,-0.063148321909653,
1.54045461629985E-17));
#54780=CARTESIAN_POINT('Ctrl Pts',(-0.0213610269805812,-0.0637483119177658,
2.74020614788251E-17));
#54781=CARTESIAN_POINT('Ctrl Pts',(-0.0201922068122268,-0.0643104725864732,
2.08166817117217E-17));
#54782=CARTESIAN_POINT('Ctrl Pts',(-0.0159953557649841,-0.06632900773419,
-2.89476499819983E-18));
#54783=CARTESIAN_POINT('Ctrl Pts',(-0.0115821440144441,-0.0678613924765087,
8.36577011636678E-17));
#54784=CARTESIAN_POINT('Ctrl Pts',(-0.00702730608058084,-0.0689290076177083,
3.29597460435593E-17));
#54785=CARTESIAN_POINT('Ctrl Pts',(-0.00486576782889167,-0.0694356537375689,
8.90058721821139E-18));
#54786=CARTESIAN_POINT('Ctrl Pts',(-0.00267298950544152,-0.0698366915944207,
1.55243141773906E-16));
#54787=CARTESIAN_POINT('Ctrl Pts',(-0.000469913444744201,-0.0701325044915826,
1.50487261540988E-16));
#54788=CARTESIAN_POINT('Ctrl Pts',(0.00411297771785086,-0.0707478615082424,
1.40593966489296E-16));
#54789=CARTESIAN_POINT('Ctrl Pts',(0.00875406260761827,-0.0709126569904891,
-5.24987388074468E-17));
#54790=CARTESIAN_POINT('Ctrl Pts',(0.0133848262570198,-0.0706465207975322,
-8.15320033709099E-17));
#54791=CARTESIAN_POINT('Ctrl Pts',(0.01601004384827,-0.0704956460243166,
-9.79911972823228E-17));
#54792=CARTESIAN_POINT('Ctrl Pts',(0.0186321482126508,-0.0702059750708208,
-2.51203942901452E-17));
#54793=CARTESIAN_POINT('Ctrl Pts',(0.021239506109343,-0.0697786235236676,
-9.54097911787244E-18));
#54794=CARTESIAN_POINT('Ctrl Pts',(0.0234844735095893,-0.0694106685555288,
3.87309005192856E-18));
#54795=CARTESIAN_POINT('Ctrl Pts',(0.0257136024412654,-0.0689411634638083,
9.07880977736139E-19));
#54796=CARTESIAN_POINT('Ctrl Pts',(0.0279116068143838,-0.0683739194742597,
-6.28837260041593E-18));
#54797=CARTESIAN_POINT('Ctrl Pts',(0.0340160087394049,-0.0667985425805166,
-2.62741491223654E-17));
#54798=CARTESIAN_POINT('Ctrl Pts',(0.0398983402063176,-0.0644702353768579,
1.18194476211714E-16));
#54799=CARTESIAN_POINT('Ctrl Pts',(0.0454040549742523,-0.061410347827305,
1.31080042653497E-16));
#54800=CARTESIAN_POINT('Ctrl Pts',(0.0466714005203764,-0.0607060006133608,
1.34046136235822E-16));
#54801=CARTESIAN_POINT('Ctrl Pts',(0.0479187804398171,-0.0599626729111359,
-2.46165589825557E-18));
#54802=CARTESIAN_POINT('Ctrl Pts',(0.0491442338326719,-0.0591802323922411,
0.));
#54803=CARTESIAN_POINT('Ctrl Pts',(0.0491442338326711,-0.0591802323922418,
-7.97972798949331E-17));
#54804=CARTESIAN_POINT('Ctrl Pts',(0.0294658500759823,-0.0755214844234611,
-0.00185225568085374));
#54805=CARTESIAN_POINT('Ctrl Pts',(0.00116787785413063,-0.0811365380031219,
-0.00370451136170736));
#54806=CARTESIAN_POINT('Ctrl Pts',(-0.0230798862214635,-0.0735074875147251,
-0.00555676704256102));
#54807=CARTESIAN_POINT('Ctrl Pts',(-0.047327650297058,-0.0658784370263282,
-0.00740902272341471));
#54808=CARTESIAN_POINT('Ctrl Pts',(-0.0675252062263949,-0.0450052824698734,
-0.00926127840426843));
#54809=CARTESIAN_POINT('Ctrl Pts',(-0.0743016119651088,-0.0204550360065341,
-0.0111135340851221));
#54810=CARTESIAN_POINT('Ctrl Pts',(-0.0761269997977368,-0.0138418367811431,
-0.0116124836924973));
#54811=CARTESIAN_POINT('Ctrl Pts',(-0.0769785170734933,-0.00696181902737242,
-0.0121114332998725));
#54812=CARTESIAN_POINT('Ctrl Pts',(-0.0769167618896329,-6.73610264414135E-5,
-0.0126103829072477));
#54813=CARTESIAN_POINT('Origin',(0.,0.,-0.2904));
#54814=CARTESIAN_POINT('Origin',(0.,0.,0.));
#54815=CARTESIAN_POINT('Origin',(-0.0288,-0.1152,0.0585));
#54816=CARTESIAN_POINT('',(0.0288,-0.1152,0.13));
#54817=CARTESIAN_POINT('',(-0.0288,-0.1152,0.13));
#54818=CARTESIAN_POINT('',(-0.0144,-0.1152,0.13));
#54819=CARTESIAN_POINT('',(0.0288,-0.1152,0.0585));
#54820=CARTESIAN_POINT('',(0.0288,-0.1152,0.0585));
#54821=CARTESIAN_POINT('',(-0.0288,-0.1152,0.0585));
#54822=CARTESIAN_POINT('',(-0.0288,-0.1152,0.0585));
#54823=CARTESIAN_POINT('',(-0.0288,-0.1152,0.0585));
#54824=CARTESIAN_POINT('Origin',(0.0288,-0.1152,0.0585));
#54825=CARTESIAN_POINT('',(0.0288,0.1152,0.13));
#54826=CARTESIAN_POINT('',(0.0288,0.0288,0.13));
#54827=CARTESIAN_POINT('',(0.0288,-0.0576,0.13));
#54828=CARTESIAN_POINT('',(0.0288,0.1152,0.0585));
#54829=CARTESIAN_POINT('',(0.0288,0.1152,0.0585));
#54830=CARTESIAN_POINT('',(0.0288,0.0288,0.0585));
#54831=CARTESIAN_POINT('',(0.0288,-0.1152,0.0585));
#54832=CARTESIAN_POINT('',(0.0288,0.0288,0.0585));
#54833=CARTESIAN_POINT('Origin',(-0.0288,0.1152,0.0585));
#54834=CARTESIAN_POINT('',(-0.0288,0.0288,0.13));
#54835=CARTESIAN_POINT('',(-0.0288,0.1152,0.13));
#54836=CARTESIAN_POINT('',(-0.0288,0.0576,0.13));
#54837=CARTESIAN_POINT('',(-0.0288,0.0288,0.0585));
#54838=CARTESIAN_POINT('',(-0.0288,0.0288,0.0585));
#54839=CARTESIAN_POINT('',(-0.0288,0.1152,0.0585));
#54840=CARTESIAN_POINT('',(-0.0288,0.1152,0.0585));
#54841=CARTESIAN_POINT('',(-0.0288,0.1152,0.0585));
#54842=CARTESIAN_POINT('Origin',(-0.0288,0.1152,0.0585));
#54843=CARTESIAN_POINT('',(-0.0288,-0.0288,0.13));
#54844=CARTESIAN_POINT('',(-0.0288,0.0576,0.13));
#54845=CARTESIAN_POINT('',(-0.0288,-0.0288,0.0585));
#54846=CARTESIAN_POINT('',(-0.0288,0.1152,0.0585));
#54847=CARTESIAN_POINT('',(-0.0288,-0.0288,0.0585));
#54848=CARTESIAN_POINT('Origin',(0.0288,0.1152,0.0585));
#54849=CARTESIAN_POINT('',(0.0144,0.1152,0.13));
#54850=CARTESIAN_POINT('',(0.0288,0.1152,0.0585));
#54851=CARTESIAN_POINT('Origin',(0.0288,-0.1152,0.0585));
#54852=CARTESIAN_POINT('',(0.0288,-0.0288,0.13));
#54853=CARTESIAN_POINT('',(0.0288,-0.0576,0.13));
#54854=CARTESIAN_POINT('',(0.0288,-0.0288,0.0585));
#54855=CARTESIAN_POINT('',(0.0288,-0.0288,0.0585));
#54856=CARTESIAN_POINT('',(0.0288,-0.1152,0.0585));
#54857=CARTESIAN_POINT('Origin',(0.,0.,0.13));
#54858=CARTESIAN_POINT('',(-0.1275,-1.56142466891288E-17,0.13));
#54859=CARTESIAN_POINT('Origin',(0.,0.,0.13));
#54860=CARTESIAN_POINT('',(-0.1152,-0.0288,0.13));
#54861=CARTESIAN_POINT('',(-0.0576,-0.0288,0.13));
#54862=CARTESIAN_POINT('',(-0.1152,0.0288,0.13));
#54863=CARTESIAN_POINT('',(-0.1152,0.0144,0.13));
#54864=CARTESIAN_POINT('',(0.0576,0.0288,0.13));
#54865=CARTESIAN_POINT('',(0.1152,0.0288,0.13));
#54866=CARTESIAN_POINT('',(0.0576,0.0288,0.13));
#54867=CARTESIAN_POINT('',(0.1152,-0.0288,0.13));
#54868=CARTESIAN_POINT('',(0.1152,-0.0144,0.13));
#54869=CARTESIAN_POINT('',(-0.0576,-0.0288,0.13));
#54870=CARTESIAN_POINT('Origin',(-0.1152,-0.0288,0.0585));
#54871=CARTESIAN_POINT('',(-0.1152,-0.0288,0.0585));
#54872=CARTESIAN_POINT('',(-0.1152,-0.0288,0.0585));
#54873=CARTESIAN_POINT('',(-0.1152,-0.0288,0.0585));
#54874=CARTESIAN_POINT('Origin',(0.1152,0.0288,0.0585));
#54875=CARTESIAN_POINT('',(-0.1152,0.0288,0.0585));
#54876=CARTESIAN_POINT('',(-0.1152,0.0288,0.0585));
#54877=CARTESIAN_POINT('',(0.1152,0.0288,0.0585));
#54878=CARTESIAN_POINT('Origin',(0.1152,0.0288,0.0585));
#54879=CARTESIAN_POINT('',(0.1152,0.0288,0.0585));
#54880=CARTESIAN_POINT('',(0.1152,0.0288,0.0585));
#54881=CARTESIAN_POINT('',(0.1152,0.0288,0.0585));
#54882=CARTESIAN_POINT('Origin',(-0.1152,-0.0288,0.0585));
#54883=CARTESIAN_POINT('',(0.1152,-0.0288,0.0585));
#54884=CARTESIAN_POINT('',(0.1152,-0.0288,0.0585));
#54885=CARTESIAN_POINT('',(-0.1152,-0.0288,0.0585));
#54886=CARTESIAN_POINT('Origin',(-0.1152,0.0288,0.0585));
#54887=CARTESIAN_POINT('',(-0.1152,0.0288,0.0585));
#54888=CARTESIAN_POINT('Origin',(0.1152,-0.0288,0.0585));
#54889=CARTESIAN_POINT('',(0.1152,-0.0288,0.0585));
#54890=CARTESIAN_POINT('Origin',(0.,0.,0.0585));
#54891=CARTESIAN_POINT('Origin',(0.0608,0.,-0.6));
#54892=CARTESIAN_POINT('',(-0.0608,-7.44585253881591E-18,-0.6));
#54893=CARTESIAN_POINT('Origin',(0.,0.,-0.6));
#54894=CARTESIAN_POINT('Origin',(0.,0.,-0.5904));
#54895=CARTESIAN_POINT('',(-0.0704,-8.62151346599737E-18,-0.5904));
#54896=CARTESIAN_POINT('Origin',(0.16,0.,0.));
#54897=CARTESIAN_POINT('',(-0.16,-1.95943487863577E-17,0.));
#54898=CARTESIAN_POINT('Origin',(0.,0.,0.));
#54899=CARTESIAN_POINT('Origin',(0.,0.,0.039));
#54900=CARTESIAN_POINT('',(-0.16,-1.95943487863577E-17,0.078));
#54901=CARTESIAN_POINT('Origin',(0.,0.,0.078));
#54902=CARTESIAN_POINT('',(-0.16,-1.95943487863577E-17,0.039));
#54903=CARTESIAN_POINT('Origin',(0.,0.,0.104));
#54904=CARTESIAN_POINT('',(-0.14375,-1.76042977377432E-17,0.104));
#54905=CARTESIAN_POINT('',(0.,0.,0.));
#54906=CARTESIAN_POINT('',(0.,0.,0.));
#54907=CARTESIAN_POINT('',(0.,0.,0.));
#54908=CARTESIAN_POINT('',(0.,0.,0.));
#54909=CARTESIAN_POINT('',(0.,0.,0.));
#54910=CARTESIAN_POINT('',(0.,0.,0.));
#54911=CARTESIAN_POINT('',(0.,-1.6,10.1));
#54912=CARTESIAN_POINT('',(0.,-1.6,0.));
#54913=CARTESIAN_POINT('',(0.,-1.6,0.));
#54914=CARTESIAN_POINT('',(0.,-1.6,0.));
#54915=CARTESIAN_POINT('',(0.,-1.6,10.935));
#54916=CARTESIAN_POINT('',(0.,-1.6,10.935));
#54917=CARTESIAN_POINT('',(0.,0.,0.));
#54918=CARTESIAN_POINT('',(2.0818995585505E-16,3.4,2.));
#54919=CARTESIAN_POINT('',(4.17279956956878,1.11809827484289,12.2));
#54920=CARTESIAN_POINT('',(0.,1.28,13.18));
#54921=CARTESIAN_POINT('',(2.0818995585505E-16,3.4,10.1));
#54922=CARTESIAN_POINT('',(0.55,-1.6,11.06));
#54923=CARTESIAN_POINT('',(0.65,-1.6,10.4));
#54924=CARTESIAN_POINT('',(0.1,-1.6,10.58));
#54925=CARTESIAN_POINT('',(-2.94448637286709,-1.7,2.));
#54926=CARTESIAN_POINT('',(2.94448637286709,-1.7,2.));
#54927=CARTESIAN_POINT('',(2.0818995585505E-16,3.4,11.4));
#54928=CARTESIAN_POINT('',(-2.94448637286709,-1.7,11.4));
#54929=CARTESIAN_POINT('',(2.94448637286709,-1.7,11.4));
#54930=CARTESIAN_POINT('',(3.05470129472589,3.05470129472589,12.2));
#54931=CARTESIAN_POINT('',(1.11809827484289,4.17279956956878,12.2));
#54932=CARTESIAN_POINT('',(-1.11809827484289,4.17279956956878,12.2));
#54933=CARTESIAN_POINT('',(-3.05470129472589,3.05470129472589,12.2));
#54934=CARTESIAN_POINT('',(-4.17279956956877,1.11809827484289,12.2));
#54935=CARTESIAN_POINT('',(-4.17279956956878,-1.11809827484289,12.2));
#54936=CARTESIAN_POINT('',(-3.05470129472589,-3.05470129472589,12.2));
#54937=CARTESIAN_POINT('',(-1.11809827484289,-4.17279956956878,12.2));
#54938=CARTESIAN_POINT('',(1.11809827484289,-4.17279956956878,12.2));
#54939=CARTESIAN_POINT('',(3.05470129472588,-3.05470129472589,12.2));
#54940=CARTESIAN_POINT('',(4.17279956956878,-1.11809827484289,12.2));
#54941=CARTESIAN_POINT('',(4.32,0.,0.5));
#54942=CARTESIAN_POINT('',(2.16,3.74122974434878,0.5));
#54943=CARTESIAN_POINT('',(-2.16,3.74122974434878,0.5));
#54944=CARTESIAN_POINT('',(-4.32,5.29047417231657E-16,0.5));
#54945=CARTESIAN_POINT('',(-2.16,-3.74122974434877,0.5));
#54946=CARTESIAN_POINT('',(2.16,-3.74122974434878,0.5));
#54947=CARTESIAN_POINT('',(0.,-1.28,13.18));
#54948=CARTESIAN_POINT('',(-2.94448637286709,-1.7,10.1));
#54949=CARTESIAN_POINT('',(2.94448637286709,-1.7,10.1));
#54950=CARTESIAN_POINT('',(2.0818995585505E-16,3.4,3.16));
#54951=CARTESIAN_POINT('',(-2.94448637286709,-1.7,3.16));
#54952=CARTESIAN_POINT('',(2.94448637286709,-1.7,3.16));
#54953=CARTESIAN_POINT('',(2.90118510267787,0.0750000000000004,10.55));
#54954=CARTESIAN_POINT('',(-0.275,-1.12368602791856,11.06));
#54955=CARTESIAN_POINT('',(-0.275,-2.07631397208144,11.06));
#54956=CARTESIAN_POINT('',(2.12156986040721,0.225333209967908,10.935));
#54957=CARTESIAN_POINT('',(2.64156986040721,-0.675333209967908,10.935));
#54958=CARTESIAN_POINT('',(-0.65,-1.6,10.4));
#54959=UNCERTAINTY_MEASURE_WITH_UNIT(LENGTH_MEASURE(0.001),#55003,
'DISTANCE_ACCURACY_VALUE',
'Maximum model space distance between geometric entities at asserted c
onnectivities');
#54960=UNCERTAINTY_MEASURE_WITH_UNIT(LENGTH_MEASURE(0.001),#55003,
'DISTANCE_ACCURACY_VALUE',
'Maximum model space distance between geometric entities at asserted c
onnectivities');
#54961=UNCERTAINTY_MEASURE_WITH_UNIT(LENGTH_MEASURE(0.001),#55003,
'DISTANCE_ACCURACY_VALUE',
'Maximum model space distance between geometric entities at asserted c
onnectivities');
#54962=UNCERTAINTY_MEASURE_WITH_UNIT(LENGTH_MEASURE(0.001),#55003,
'DISTANCE_ACCURACY_VALUE',
'Maximum model space distance between geometric entities at asserted c
onnectivities');
#54963=UNCERTAINTY_MEASURE_WITH_UNIT(LENGTH_MEASURE(0.001),#55003,
'DISTANCE_ACCURACY_VALUE',
'Maximum model space distance between geometric entities at asserted c
onnectivities');
#54964=UNCERTAINTY_MEASURE_WITH_UNIT(LENGTH_MEASURE(0.001),#55003,
'DISTANCE_ACCURACY_VALUE',
'Maximum model space distance between geometric entities at asserted c
onnectivities');
#54965=UNCERTAINTY_MEASURE_WITH_UNIT(LENGTH_MEASURE(0.001),#55003,
'DISTANCE_ACCURACY_VALUE',
'Maximum model space distance between geometric entities at asserted c
onnectivities');
#54966=UNCERTAINTY_MEASURE_WITH_UNIT(LENGTH_MEASURE(0.001),#55003,
'DISTANCE_ACCURACY_VALUE',
'Maximum model space distance between geometric entities at asserted c
onnectivities');
#54967=UNCERTAINTY_MEASURE_WITH_UNIT(LENGTH_MEASURE(0.001),#55003,
'DISTANCE_ACCURACY_VALUE',
'Maximum model space distance between geometric entities at asserted c
onnectivities');
#54968=UNCERTAINTY_MEASURE_WITH_UNIT(LENGTH_MEASURE(0.001),#55003,
'DISTANCE_ACCURACY_VALUE',
'Maximum model space distance between geometric entities at asserted c
onnectivities');
#54969=UNCERTAINTY_MEASURE_WITH_UNIT(LENGTH_MEASURE(0.001),#55003,
'DISTANCE_ACCURACY_VALUE',
'Maximum model space distance between geometric entities at asserted c
onnectivities');
#54970=UNCERTAINTY_MEASURE_WITH_UNIT(LENGTH_MEASURE(0.001),#55003,
'DISTANCE_ACCURACY_VALUE',
'Maximum model space distance between geometric entities at asserted c
onnectivities');
#54971=UNCERTAINTY_MEASURE_WITH_UNIT(LENGTH_MEASURE(0.001),#55003,
'DISTANCE_ACCURACY_VALUE',
'Maximum model space distance between geometric entities at asserted c
onnectivities');
#54972=UNCERTAINTY_MEASURE_WITH_UNIT(LENGTH_MEASURE(0.001),#55003,
'DISTANCE_ACCURACY_VALUE',
'Maximum model space distance between geometric entities at asserted c
onnectivities');
#54973=UNCERTAINTY_MEASURE_WITH_UNIT(LENGTH_MEASURE(0.001),#55003,
'DISTANCE_ACCURACY_VALUE',
'Maximum model space distance between geometric entities at asserted c
onnectivities');
#54974=UNCERTAINTY_MEASURE_WITH_UNIT(LENGTH_MEASURE(0.001),#55003,
'DISTANCE_ACCURACY_VALUE',
'Maximum model space distance between geometric entities at asserted c
onnectivities');
#54975=UNCERTAINTY_MEASURE_WITH_UNIT(LENGTH_MEASURE(0.001),#55003,
'DISTANCE_ACCURACY_VALUE',
'Maximum model space distance between geometric entities at asserted c
onnectivities');
#54976=UNCERTAINTY_MEASURE_WITH_UNIT(LENGTH_MEASURE(0.001),#55003,
'DISTANCE_ACCURACY_VALUE',
'Maximum model space distance between geometric entities at asserted c
onnectivities');
#54977=UNCERTAINTY_MEASURE_WITH_UNIT(LENGTH_MEASURE(0.001),#55003,
'DISTANCE_ACCURACY_VALUE',
'Maximum model space distance between geometric entities at asserted c
onnectivities');
#54978=UNCERTAINTY_MEASURE_WITH_UNIT(LENGTH_MEASURE(0.001),#55003,
'DISTANCE_ACCURACY_VALUE',
'Maximum model space distance between geometric entities at asserted c
onnectivities');
#54979=UNCERTAINTY_MEASURE_WITH_UNIT(LENGTH_MEASURE(0.001),#55003,
'DISTANCE_ACCURACY_VALUE',
'Maximum model space distance between geometric entities at asserted c
onnectivities');
#54980=UNCERTAINTY_MEASURE_WITH_UNIT(LENGTH_MEASURE(0.001),#55003,
'DISTANCE_ACCURACY_VALUE',
'Maximum model space distance between geometric entities at asserted c
onnectivities');
#54981=(
GEOMETRIC_REPRESENTATION_CONTEXT(3)
GLOBAL_UNCERTAINTY_ASSIGNED_CONTEXT((#54959))
GLOBAL_UNIT_ASSIGNED_CONTEXT((#55003,#55005,#55006))
REPRESENTATION_CONTEXT('','3D')
);
#54982=(
GEOMETRIC_REPRESENTATION_CONTEXT(3)
GLOBAL_UNCERTAINTY_ASSIGNED_CONTEXT((#54960))
GLOBAL_UNIT_ASSIGNED_CONTEXT((#55003,#55005,#55006))
REPRESENTATION_CONTEXT('','3D')
);
#54983=(
GEOMETRIC_REPRESENTATION_CONTEXT(3)
GLOBAL_UNCERTAINTY_ASSIGNED_CONTEXT((#54961))
GLOBAL_UNIT_ASSIGNED_CONTEXT((#55003,#55005,#55006))
REPRESENTATION_CONTEXT('','3D')
);
#54984=(
GEOMETRIC_REPRESENTATION_CONTEXT(3)
GLOBAL_UNCERTAINTY_ASSIGNED_CONTEXT((#54962))
GLOBAL_UNIT_ASSIGNED_CONTEXT((#55003,#55005,#55006))
REPRESENTATION_CONTEXT('','3D')
);
#54985=(
GEOMETRIC_REPRESENTATION_CONTEXT(3)
GLOBAL_UNCERTAINTY_ASSIGNED_CONTEXT((#54963))
GLOBAL_UNIT_ASSIGNED_CONTEXT((#55003,#55005,#55006))
REPRESENTATION_CONTEXT('','3D')
);
#54986=(
GEOMETRIC_REPRESENTATION_CONTEXT(3)
GLOBAL_UNCERTAINTY_ASSIGNED_CONTEXT((#54964))
GLOBAL_UNIT_ASSIGNED_CONTEXT((#55003,#55005,#55006))
REPRESENTATION_CONTEXT('','3D')
);
#54987=(
GEOMETRIC_REPRESENTATION_CONTEXT(3)
GLOBAL_UNCERTAINTY_ASSIGNED_CONTEXT((#54965))
GLOBAL_UNIT_ASSIGNED_CONTEXT((#55003,#55005,#55006))
REPRESENTATION_CONTEXT('','3D')
);
#54988=(
GEOMETRIC_REPRESENTATION_CONTEXT(3)
GLOBAL_UNCERTAINTY_ASSIGNED_CONTEXT((#54966))
GLOBAL_UNIT_ASSIGNED_CONTEXT((#55003,#55005,#55006))
REPRESENTATION_CONTEXT('','3D')
);
#54989=(
GEOMETRIC_REPRESENTATION_CONTEXT(3)
GLOBAL_UNCERTAINTY_ASSIGNED_CONTEXT((#54967))
GLOBAL_UNIT_ASSIGNED_CONTEXT((#55003,#55005,#55006))
REPRESENTATION_CONTEXT('','3D')
);
#54990=(
GEOMETRIC_REPRESENTATION_CONTEXT(3)
GLOBAL_UNCERTAINTY_ASSIGNED_CONTEXT((#54968))
GLOBAL_UNIT_ASSIGNED_CONTEXT((#55003,#55005,#55006))
REPRESENTATION_CONTEXT('','3D')
);
#54991=(
GEOMETRIC_REPRESENTATION_CONTEXT(3)
GLOBAL_UNCERTAINTY_ASSIGNED_CONTEXT((#54969))
GLOBAL_UNIT_ASSIGNED_CONTEXT((#55003,#55005,#55006))
REPRESENTATION_CONTEXT('','3D')
);
#54992=(
GEOMETRIC_REPRESENTATION_CONTEXT(3)
GLOBAL_UNCERTAINTY_ASSIGNED_CONTEXT((#54970))
GLOBAL_UNIT_ASSIGNED_CONTEXT((#55003,#55005,#55006))
REPRESENTATION_CONTEXT('','3D')
);
#54993=(
GEOMETRIC_REPRESENTATION_CONTEXT(3)
GLOBAL_UNCERTAINTY_ASSIGNED_CONTEXT((#54971))
GLOBAL_UNIT_ASSIGNED_CONTEXT((#55003,#55005,#55006))
REPRESENTATION_CONTEXT('','3D')
);
#54994=(
GEOMETRIC_REPRESENTATION_CONTEXT(3)
GLOBAL_UNCERTAINTY_ASSIGNED_CONTEXT((#54972))
GLOBAL_UNIT_ASSIGNED_CONTEXT((#55003,#55005,#55006))
REPRESENTATION_CONTEXT('','3D')
);
#54995=(
GEOMETRIC_REPRESENTATION_CONTEXT(3)
GLOBAL_UNCERTAINTY_ASSIGNED_CONTEXT((#54973))
GLOBAL_UNIT_ASSIGNED_CONTEXT((#55003,#55005,#55006))
REPRESENTATION_CONTEXT('','3D')
);
#54996=(
GEOMETRIC_REPRESENTATION_CONTEXT(3)
GLOBAL_UNCERTAINTY_ASSIGNED_CONTEXT((#54974))
GLOBAL_UNIT_ASSIGNED_CONTEXT((#55003,#55005,#55006))
REPRESENTATION_CONTEXT('','3D')
);
#54997=(
GEOMETRIC_REPRESENTATION_CONTEXT(3)
GLOBAL_UNCERTAINTY_ASSIGNED_CONTEXT((#54975))
GLOBAL_UNIT_ASSIGNED_CONTEXT((#55003,#55005,#55006))
REPRESENTATION_CONTEXT('','3D')
);
#54998=(
GEOMETRIC_REPRESENTATION_CONTEXT(3)
GLOBAL_UNCERTAINTY_ASSIGNED_CONTEXT((#54976))
GLOBAL_UNIT_ASSIGNED_CONTEXT((#55003,#55005,#55006))
REPRESENTATION_CONTEXT('','3D')
);
#54999=(
GEOMETRIC_REPRESENTATION_CONTEXT(3)
GLOBAL_UNCERTAINTY_ASSIGNED_CONTEXT((#54977))
GLOBAL_UNIT_ASSIGNED_CONTEXT((#55003,#55005,#55006))
REPRESENTATION_CONTEXT('','3D')
);
#55000=(
GEOMETRIC_REPRESENTATION_CONTEXT(3)
GLOBAL_UNCERTAINTY_ASSIGNED_CONTEXT((#54978))
GLOBAL_UNIT_ASSIGNED_CONTEXT((#55003,#55005,#55006))
REPRESENTATION_CONTEXT('','3D')
);
#55001=(
GEOMETRIC_REPRESENTATION_CONTEXT(3)
GLOBAL_UNCERTAINTY_ASSIGNED_CONTEXT((#54979))
GLOBAL_UNIT_ASSIGNED_CONTEXT((#55003,#55005,#55006))
REPRESENTATION_CONTEXT('','3D')
);
#55002=(
GEOMETRIC_REPRESENTATION_CONTEXT(3)
GLOBAL_UNCERTAINTY_ASSIGNED_CONTEXT((#54980))
GLOBAL_UNIT_ASSIGNED_CONTEXT((#55003,#55005,#55006))
REPRESENTATION_CONTEXT('','3D')
);
#55003=(
LENGTH_UNIT()
NAMED_UNIT(*)
SI_UNIT(.CENTI.,.METRE.)
);
#55004=(
LENGTH_UNIT()
NAMED_UNIT(*)
SI_UNIT($,.METRE.)
);
#55005=(
NAMED_UNIT(*)
PLANE_ANGLE_UNIT()
SI_UNIT($,.RADIAN.)
);
#55006=(
NAMED_UNIT(*)
SI_UNIT($,.STERADIAN.)
SOLID_ANGLE_UNIT()
);
#55007=SHAPE_DEFINITION_REPRESENTATION(#55028,#55103);
#55008=SHAPE_DEFINITION_REPRESENTATION(#55029,#55104);
#55009=SHAPE_DEFINITION_REPRESENTATION(#55030,#55105);
#55010=SHAPE_DEFINITION_REPRESENTATION(#55031,#55106);
#55011=SHAPE_DEFINITION_REPRESENTATION(#55032,#55107);
#55012=SHAPE_DEFINITION_REPRESENTATION(#55033,#55108);
#55013=SHAPE_DEFINITION_REPRESENTATION(#55034,#55109);
#55014=SHAPE_DEFINITION_REPRESENTATION(#55035,#55110);
#55015=SHAPE_DEFINITION_REPRESENTATION(#55036,#55111);
#55016=SHAPE_DEFINITION_REPRESENTATION(#55037,#55112);
#55017=SHAPE_DEFINITION_REPRESENTATION(#55038,#55113);
#55018=SHAPE_DEFINITION_REPRESENTATION(#55039,#55114);
#55019=SHAPE_DEFINITION_REPRESENTATION(#55040,#55115);
#55020=SHAPE_DEFINITION_REPRESENTATION(#55041,#55116);
#55021=SHAPE_DEFINITION_REPRESENTATION(#55042,#55117);
#55022=SHAPE_DEFINITION_REPRESENTATION(#55043,#55118);
#55023=SHAPE_DEFINITION_REPRESENTATION(#55044,#55119);
#55024=SHAPE_DEFINITION_REPRESENTATION(#55045,#55120);
#55025=SHAPE_DEFINITION_REPRESENTATION(#55046,#55121);
#55026=SHAPE_DEFINITION_REPRESENTATION(#55047,#55122);
#55027=SHAPE_DEFINITION_REPRESENTATION(#55048,#55123);
#55028=PRODUCT_DEFINITION_SHAPE('',$,#55125);
#55029=PRODUCT_DEFINITION_SHAPE('',$,#55126);
#55030=PRODUCT_DEFINITION_SHAPE('',$,#55127);
#55031=PRODUCT_DEFINITION_SHAPE('',$,#55128);
#55032=PRODUCT_DEFINITION_SHAPE('',$,#55129);
#55033=PRODUCT_DEFINITION_SHAPE('',$,#55130);
#55034=PRODUCT_DEFINITION_SHAPE('',$,#55131);
#55035=PRODUCT_DEFINITION_SHAPE('',$,#55132);
#55036=PRODUCT_DEFINITION_SHAPE('',$,#55133);
#55037=PRODUCT_DEFINITION_SHAPE('',$,#55134);
#55038=PRODUCT_DEFINITION_SHAPE('',$,#55135);
#55039=PRODUCT_DEFINITION_SHAPE('',$,#55136);
#55040=PRODUCT_DEFINITION_SHAPE('',$,#55137);
#55041=PRODUCT_DEFINITION_SHAPE('',$,#55138);
#55042=PRODUCT_DEFINITION_SHAPE('',$,#55139);
#55043=PRODUCT_DEFINITION_SHAPE('',$,#55140);
#55044=PRODUCT_DEFINITION_SHAPE('',$,#55141);
#55045=PRODUCT_DEFINITION_SHAPE('',$,#55142);
#55046=PRODUCT_DEFINITION_SHAPE('',$,#55143);
#55047=PRODUCT_DEFINITION_SHAPE('',$,#55144);
#55048=PRODUCT_DEFINITION_SHAPE('',$,#55145);
#55049=PRODUCT_DEFINITION_SHAPE($,$,#173);
#55050=PRODUCT_DEFINITION_SHAPE($,$,#174);
#55051=PRODUCT_DEFINITION_SHAPE($,$,#175);
#55052=PRODUCT_DEFINITION_SHAPE($,$,#176);
#55053=PRODUCT_DEFINITION_SHAPE($,$,#177);
#55054=PRODUCT_DEFINITION_SHAPE($,$,#178);
#55055=PRODUCT_DEFINITION_SHAPE($,$,#179);
#55056=PRODUCT_DEFINITION_SHAPE($,$,#180);
#55057=PRODUCT_DEFINITION_SHAPE($,$,#181);
#55058=PRODUCT_DEFINITION_SHAPE($,$,#182);
#55059=PRODUCT_DEFINITION_SHAPE($,$,#183);
#55060=PRODUCT_DEFINITION_SHAPE($,$,#184);
#55061=PRODUCT_DEFINITION_SHAPE($,$,#185);
#55062=PRODUCT_DEFINITION_SHAPE($,$,#186);
#55063=PRODUCT_DEFINITION_SHAPE($,$,#187);
#55064=PRODUCT_DEFINITION_SHAPE($,$,#188);
#55065=PRODUCT_DEFINITION_SHAPE($,$,#189);
#55066=PRODUCT_DEFINITION_SHAPE($,$,#190);
#55067=PRODUCT_DEFINITION_SHAPE($,$,#191);
#55068=PRODUCT_DEFINITION_SHAPE($,$,#192);
#55069=PRODUCT_DEFINITION_SHAPE($,$,#193);
#55070=PRODUCT_DEFINITION_SHAPE($,$,#194);
#55071=PRODUCT_DEFINITION_SHAPE($,$,#195);
#55072=PRODUCT_DEFINITION_SHAPE($,$,#196);
#55073=PRODUCT_DEFINITION_SHAPE($,$,#197);
#55074=PRODUCT_DEFINITION_SHAPE($,$,#198);
#55075=PRODUCT_DEFINITION_SHAPE($,$,#199);
#55076=PRODUCT_DEFINITION_SHAPE($,$,#200);
#55077=PRODUCT_DEFINITION_SHAPE($,$,#201);
#55078=PRODUCT_DEFINITION_SHAPE($,$,#202);
#55079=PRODUCT_DEFINITION_SHAPE($,$,#203);
#55080=PRODUCT_DEFINITION_SHAPE($,$,#204);
#55081=PRODUCT_DEFINITION_SHAPE($,$,#205);
#55082=PRODUCT_DEFINITION_SHAPE($,$,#206);
#55083=PRODUCT_DEFINITION_SHAPE($,$,#207);
#55084=PRODUCT_DEFINITION_SHAPE($,$,#208);
#55085=PRODUCT_DEFINITION_SHAPE($,$,#209);
#55086=PRODUCT_DEFINITION_SHAPE($,$,#210);
#55087=PRODUCT_DEFINITION_SHAPE($,$,#211);
#55088=PRODUCT_DEFINITION_SHAPE($,$,#212);
#55089=PRODUCT_DEFINITION_SHAPE($,$,#213);
#55090=PRODUCT_DEFINITION_SHAPE($,$,#214);
#55091=PRODUCT_DEFINITION_SHAPE($,$,#215);
#55092=PRODUCT_DEFINITION_SHAPE($,$,#216);
#55093=PRODUCT_DEFINITION_SHAPE($,$,#217);
#55094=PRODUCT_DEFINITION_SHAPE($,$,#218);
#55095=PRODUCT_DEFINITION_SHAPE($,$,#219);
#55096=PRODUCT_DEFINITION_SHAPE($,$,#220);
#55097=PRODUCT_DEFINITION_SHAPE($,$,#221);
#55098=PRODUCT_DEFINITION_SHAPE($,$,#222);
#55099=PRODUCT_DEFINITION_SHAPE($,$,#223);
#55100=PRODUCT_DEFINITION_SHAPE($,$,#224);
#55101=PRODUCT_DEFINITION_SHAPE($,$,#225);
#55102=PRODUCT_DEFINITION_SHAPE($,$,#226);
#55103=SHAPE_REPRESENTATION('',(#24770,#27142,#27143,#27144,#27145,#27146,
#27147,#27148,#27149,#27150,#27151,#27152,#27153,#27154,#27155,#27156,#27157,
#27158,#27159,#27160,#27161,#27162,#27163,#27164,#27165,#27166,#27167,#27168,
#27169,#27170,#27171,#27172,#27173,#27174,#27175,#27176,#27177,#27178,#27179,
#27180,#27181,#27182,#27183,#27184,#27185,#27186,#27187,#27188,#27189,#27190,
#27191,#27192,#27193,#27194,#27195),#54981);
#55104=SHAPE_REPRESENTATION('',(#24771),#54982);
#55105=SHAPE_REPRESENTATION('',(#24929),#54983);
#55106=SHAPE_REPRESENTATION('',(#25058),#54984);
#55107=SHAPE_REPRESENTATION('',(#25631),#54985);
#55108=SHAPE_REPRESENTATION('',(#25681),#54986);
#55109=SHAPE_REPRESENTATION('',(#25749),#54987);
#55110=SHAPE_REPRESENTATION('',(#25799),#54988);
#55111=SHAPE_REPRESENTATION('',(#25845),#54989);
#55112=SHAPE_REPRESENTATION('',(#25906),#54990);
#55113=SHAPE_REPRESENTATION('',(#25953),#54991);
#55114=SHAPE_REPRESENTATION('',(#26022),#54992);
#55115=SHAPE_REPRESENTATION('',(#26062),#54993);
#55116=SHAPE_REPRESENTATION('',(#26099),#54994);
#55117=SHAPE_REPRESENTATION('',(#26151),#54995);
#55118=SHAPE_REPRESENTATION('',(#26185),#54996);
#55119=SHAPE_REPRESENTATION('',(#26252),#54997);
#55120=SHAPE_REPRESENTATION('',(#26524),#54998);
#55121=SHAPE_REPRESENTATION('',(#26786),#54999);
#55122=SHAPE_REPRESENTATION('',(#27025),#55000);
#55123=SHAPE_REPRESENTATION('',(#27074),#55001);
#55124=PRODUCT_DEFINITION_CONTEXT('part definition',#55189,'design');
#55125=PRODUCT_DEFINITION('2026-10-18-23-35-45-834','MAS-299',#55146,#55124);
#55126=PRODUCT_DEFINITION('2026-10-18-23-35-47-869',
'01_Rear_End_Cap_D95',#55147,#55124);
#55127=PRODUCT_DEFINITION('2026-10-18-23-35-49-944',
'02_Chopper_Enclosure_Guard_Shield_D92',#55148,#55124);
#55128=PRODUCT_DEFINITION('2026-10-18-23-35-54-661',
'03_Isogrid_Motor_Mount_Faceplate',#55149,#55124);
#55129=PRODUCT_DEFINITION('2026-10-18-23-36-09-603',
'04_Beam_Port_Tube_D18',#55150,#55124);
#55130=PRODUCT_DEFINITION('2026-10-18-23-36-10-777',
'05_Port_Clamp_Collar_D31',#55151,#55124);
#55131=PRODUCT_DEFINITION('2026-10-18-23-36-12-808',
'06_Motor_Mount_Bulkhead_Plate',#55152,#55124);
#55132=PRODUCT_DEFINITION('2026-10-18-23-36-18-583',
'07_BLDC_Spindle_Motor_D16x28',#55153,#55124);
#55133=PRODUCT_DEFINITION('2026-10-18-23-36-21-472',
'08_Disc_Aluminium_Hub_Clamp_Adapter',#55154,#55124);
#55134=PRODUCT_DEFINITION('2026-10-18-23-36-24-161',
'09_Disc_Clamp_Ring_D14',#55155,#55124);
#55135=PRODUCT_DEFINITION('2026-10-18-23-36-26-322',
'10_Photo-Etched_Slotted_Chopper_Disc_D47x0.5',#55156,#55124);
#55136=PRODUCT_DEFINITION('2026-10-18-23-36-29-833',
'11_Optoelectronic_Slot_Sensor_PCB',#55157,#55124);
#55137=PRODUCT_DEFINITION('2026-10-18-23-36-34-140',
'12_Sensor_Alignment_Mounting_Bracket',#55158,#55124);
#55138=PRODUCT_DEFINITION('2026-10-18-23-36-38-410',
'13_Motor_Speed_Controller_Board_D76',#55159,#55124);
#55139=PRODUCT_DEFINITION('2026-10-18-23-37-08-575',
'20_ISO_4026_M2x2_Set_Screw',#55160,#55124);
#55140=PRODUCT_DEFINITION('2026-10-18-23-36-48-728',
'14_Hex_Standoff_M2.5_AF5x10_Male-Female',#55161,#55124);
#55141=PRODUCT_DEFINITION('2026-10-18-23-36-52-332',
'15_ISO_4762_M2x12_A2',#55162,#55124);
#55142=PRODUCT_DEFINITION('2026-10-18-23-36-55-856',
'16_ISO_4762_M2x10_A2',#55163,#55124);
#55143=PRODUCT_DEFINITION('2026-10-18-23-36-59-357',
'17_ISO_4762_M2.5x6_A2',#55164,#55124);
#55144=PRODUCT_DEFINITION('2026-10-18-23-37-02-926',
'18_ISO_7045_M1.6x3_A2',#55165,#55124);
#55145=PRODUCT_DEFINITION('2026-10-18-23-37-05-724',
'19_ISO_7045_M1.6x6_A2',#55166,#55124);
#55146=PRODUCT_DEFINITION_FORMATION('',$,#55191);
#55147=PRODUCT_DEFINITION_FORMATION('',$,#55192);
#55148=PRODUCT_DEFINITION_FORMATION('',$,#55193);
#55149=PRODUCT_DEFINITION_FORMATION('',$,#55194);
#55150=PRODUCT_DEFINITION_FORMATION('',$,#55195);
#55151=PRODUCT_DEFINITION_FORMATION('',$,#55196);
#55152=PRODUCT_DEFINITION_FORMATION('',$,#55197);
#55153=PRODUCT_DEFINITION_FORMATION('',$,#55198);
#55154=PRODUCT_DEFINITION_FORMATION('',$,#55199);
#55155=PRODUCT_DEFINITION_FORMATION('',$,#55200);
#55156=PRODUCT_DEFINITION_FORMATION('',$,#55201);
#55157=PRODUCT_DEFINITION_FORMATION('',$,#55202);
#55158=PRODUCT_DEFINITION_FORMATION('',$,#55203);
#55159=PRODUCT_DEFINITION_FORMATION('',$,#55204);
#55160=PRODUCT_DEFINITION_FORMATION('',$,#55205);
#55161=PRODUCT_DEFINITION_FORMATION('',$,#55206);
#55162=PRODUCT_DEFINITION_FORMATION('',$,#55207);
#55163=PRODUCT_DEFINITION_FORMATION('',$,#55208);
#55164=PRODUCT_DEFINITION_FORMATION('',$,#55209);
#55165=PRODUCT_DEFINITION_FORMATION('',$,#55210);
#55166=PRODUCT_DEFINITION_FORMATION('',$,#55211);
#55167=PRODUCT_RELATED_PRODUCT_CATEGORY('MAS-299','MAS-299',(#55191));
#55168=PRODUCT_RELATED_PRODUCT_CATEGORY('01_Rear_End_Cap_D95',
'01_Rear_End_Cap_D95',(#55192));
#55169=PRODUCT_RELATED_PRODUCT_CATEGORY(
'02_Chopper_Enclosure_Guard_Shield_D92',
'02_Chopper_Enclosure_Guard_Shield_D92',(#55193));
#55170=PRODUCT_RELATED_PRODUCT_CATEGORY(
'03_Isogrid_Motor_Mount_Faceplate','03_Isogrid_Motor_Mount_Faceplate',(#55194));
#55171=PRODUCT_RELATED_PRODUCT_CATEGORY('04_Beam_Port_Tube_D18',
'04_Beam_Port_Tube_D18',(#55195));
#55172=PRODUCT_RELATED_PRODUCT_CATEGORY('05_Port_Clamp_Collar_D31',
'05_Port_Clamp_Collar_D31',(#55196));
#55173=PRODUCT_RELATED_PRODUCT_CATEGORY('06_Motor_Mount_Bulkhead_Plate',
'06_Motor_Mount_Bulkhead_Plate',(#55197));
#55174=PRODUCT_RELATED_PRODUCT_CATEGORY('07_BLDC_Spindle_Motor_D16x28',
'07_BLDC_Spindle_Motor_D16x28',(#55198));
#55175=PRODUCT_RELATED_PRODUCT_CATEGORY(
'08_Disc_Aluminium_Hub_Clamp_Adapter',
'08_Disc_Aluminium_Hub_Clamp_Adapter',(#55199));
#55176=PRODUCT_RELATED_PRODUCT_CATEGORY('09_Disc_Clamp_Ring_D14',
'09_Disc_Clamp_Ring_D14',(#55200));
#55177=PRODUCT_RELATED_PRODUCT_CATEGORY(
'10_Photo-Etched_Slotted_Chopper_Disc_D47x0.5',
'10_Photo-Etched_Slotted_Chopper_Disc_D47x0.5',(#55201));
#55178=PRODUCT_RELATED_PRODUCT_CATEGORY(
'11_Optoelectronic_Slot_Sensor_PCB','11_Optoelectronic_Slot_Sensor_PCB',
(#55202));
#55179=PRODUCT_RELATED_PRODUCT_CATEGORY(
'12_Sensor_Alignment_Mounting_Bracket',
'12_Sensor_Alignment_Mounting_Bracket',(#55203));
#55180=PRODUCT_RELATED_PRODUCT_CATEGORY(
'13_Motor_Speed_Controller_Board_D76',
'13_Motor_Speed_Controller_Board_D76',(#55204));
#55181=PRODUCT_RELATED_PRODUCT_CATEGORY('20_ISO_4026_M2x2_Set_Screw',
'20_ISO_4026_M2x2_Set_Screw',(#55205));
#55182=PRODUCT_RELATED_PRODUCT_CATEGORY(
'14_Hex_Standoff_M2.5_AF5x10_Male-Female',
'14_Hex_Standoff_M2.5_AF5x10_Male-Female',(#55206));
#55183=PRODUCT_RELATED_PRODUCT_CATEGORY('15_ISO_4762_M2x12_A2',
'15_ISO_4762_M2x12_A2',(#55207));
#55184=PRODUCT_RELATED_PRODUCT_CATEGORY('16_ISO_4762_M2x10_A2',
'16_ISO_4762_M2x10_A2',(#55208));
#55185=PRODUCT_RELATED_PRODUCT_CATEGORY('17_ISO_4762_M2.5x6_A2',
'17_ISO_4762_M2.5x6_A2',(#55209));
#55186=PRODUCT_RELATED_PRODUCT_CATEGORY('18_ISO_7045_M1.6x3_A2',
'18_ISO_7045_M1.6x3_A2',(#55210));
#55187=PRODUCT_RELATED_PRODUCT_CATEGORY('19_ISO_7045_M1.6x6_A2',
'19_ISO_7045_M1.6x6_A2',(#55211));
#55188=APPLICATION_PROTOCOL_DEFINITION('international standard',
'automotive_design',2009,#55189);
#55189=APPLICATION_CONTEXT(
'Core Data for Automotive Mechanical Design Process');
#55190=PRODUCT_CONTEXT('part definition',#55189,'mechanical');
#55191=PRODUCT('2026-10-18-23-35-45-834','MAS-299',$,(#55190));
#55192=PRODUCT('2026-10-18-23-35-47-869','01_Rear_End_Cap_D95',$,(#55190));
#55193=PRODUCT('2026-10-18-23-35-49-944',
'02_Chopper_Enclosure_Guard_Shield_D92',$,(#55190));
#55194=PRODUCT('2026-10-18-23-35-54-661',
'03_Isogrid_Motor_Mount_Faceplate',$,(#55190));
#55195=PRODUCT('2026-10-18-23-36-09-603','04_Beam_Port_Tube_D18',$,(#55190));
#55196=PRODUCT('2026-10-18-23-36-10-777','05_Port_Clamp_Collar_D31',$,(#55190));
#55197=PRODUCT('2026-10-18-23-36-12-808',
'06_Motor_Mount_Bulkhead_Plate',$,(#55190));
#55198=PRODUCT('2026-10-18-23-36-18-583','07_BLDC_Spindle_Motor_D16x28',
$,(#55190));
#55199=PRODUCT('2026-10-18-23-36-21-472',
'08_Disc_Aluminium_Hub_Clamp_Adapter',$,(#55190));
#55200=PRODUCT('2026-10-18-23-36-24-161','09_Disc_Clamp_Ring_D14',$,(#55190));
#55201=PRODUCT('2026-10-18-23-36-26-322',
'10_Photo-Etched_Slotted_Chopper_Disc_D47x0.5',$,(#55190));
#55202=PRODUCT('2026-10-18-23-36-29-833',
'11_Optoelectronic_Slot_Sensor_PCB',$,(#55190));
#55203=PRODUCT('2026-10-18-23-36-34-140',
'12_Sensor_Alignment_Mounting_Bracket',$,(#55190));
#55204=PRODUCT('2026-10-18-23-36-38-410',
'13_Motor_Speed_Controller_Board_D76',$,(#55190));
#55205=PRODUCT('2026-10-18-23-37-08-575','20_ISO_4026_M2x2_Set_Screw',$,
(#55190));
#55206=PRODUCT('2026-10-18-23-36-48-728',
'14_Hex_Standoff_M2.5_AF5x10_Male-Female',$,(#55190));
#55207=PRODUCT('2026-10-18-23-36-52-332','15_ISO_4762_M2x12_A2',$,(#55190));
#55208=PRODUCT('2026-10-18-23-36-55-856','16_ISO_4762_M2x10_A2',$,(#55190));
#55209=PRODUCT('2026-10-18-23-36-59-357','17_ISO_4762_M2.5x6_A2',$,(#55190));
#55210=PRODUCT('2026-10-18-23-37-02-926','18_ISO_7045_M1.6x3_A2',$,(#55190));
#55211=PRODUCT('2026-10-18-23-37-05-724','19_ISO_7045_M1.6x6_A2',$,(#55190));
#55212=PRESENTATION_STYLE_ASSIGNMENT((#55233));
#55213=PRESENTATION_STYLE_ASSIGNMENT((#55234));
#55214=PRESENTATION_STYLE_ASSIGNMENT((#55235));
#55215=PRESENTATION_STYLE_ASSIGNMENT((#55236));
#55216=PRESENTATION_STYLE_ASSIGNMENT((#55237));
#55217=PRESENTATION_STYLE_ASSIGNMENT((#55238));
#55218=PRESENTATION_STYLE_ASSIGNMENT((#55239));
#55219=PRESENTATION_STYLE_ASSIGNMENT((#55240));
#55220=PRESENTATION_STYLE_ASSIGNMENT((#55241));
#55221=PRESENTATION_STYLE_ASSIGNMENT((#55242));
#55222=PRESENTATION_STYLE_ASSIGNMENT((#55243));
#55223=PRESENTATION_STYLE_ASSIGNMENT((#55244));
#55224=PRESENTATION_STYLE_ASSIGNMENT((#55245));
#55225=PRESENTATION_STYLE_ASSIGNMENT((#55246));
#55226=PRESENTATION_STYLE_ASSIGNMENT((#55247));
#55227=PRESENTATION_STYLE_ASSIGNMENT((#55248));
#55228=PRESENTATION_STYLE_ASSIGNMENT((#55249));
#55229=PRESENTATION_STYLE_ASSIGNMENT((#55250));
#55230=PRESENTATION_STYLE_ASSIGNMENT((#55251));
#55231=PRESENTATION_STYLE_ASSIGNMENT((#55252));
#55232=PRESENTATION_STYLE_ASSIGNMENT((#55253));
#55233=SURFACE_STYLE_USAGE(.BOTH.,#55254);
#55234=SURFACE_STYLE_USAGE(.BOTH.,#55255);
#55235=SURFACE_STYLE_USAGE(.BOTH.,#55256);
#55236=SURFACE_STYLE_USAGE(.BOTH.,#55257);
#55237=SURFACE_STYLE_USAGE(.BOTH.,#55258);
#55238=SURFACE_STYLE_USAGE(.BOTH.,#55259);
#55239=SURFACE_STYLE_USAGE(.BOTH.,#55260);
#55240=SURFACE_STYLE_USAGE(.BOTH.,#55261);
#55241=SURFACE_STYLE_USAGE(.BOTH.,#55262);
#55242=SURFACE_STYLE_USAGE(.BOTH.,#55263);
#55243=SURFACE_STYLE_USAGE(.BOTH.,#55264);
#55244=SURFACE_STYLE_USAGE(.BOTH.,#55265);
#55245=SURFACE_STYLE_USAGE(.BOTH.,#55266);
#55246=SURFACE_STYLE_USAGE(.BOTH.,#55267);
#55247=SURFACE_STYLE_USAGE(.BOTH.,#55268);
#55248=SURFACE_STYLE_USAGE(.BOTH.,#55269);
#55249=SURFACE_STYLE_USAGE(.BOTH.,#55270);
#55250=SURFACE_STYLE_USAGE(.BOTH.,#55271);
#55251=SURFACE_STYLE_USAGE(.BOTH.,#55272);
#55252=SURFACE_STYLE_USAGE(.BOTH.,#55273);
#55253=SURFACE_STYLE_USAGE(.BOTH.,#55274);
#55254=SURFACE_SIDE_STYLE('',(#55275));
#55255=SURFACE_SIDE_STYLE('',(#55276));
#55256=SURFACE_SIDE_STYLE('',(#55277));
#55257=SURFACE_SIDE_STYLE('',(#55278));
#55258=SURFACE_SIDE_STYLE('',(#55279));
#55259=SURFACE_SIDE_STYLE('',(#55280));
#55260=SURFACE_SIDE_STYLE('',(#55281));
#55261=SURFACE_SIDE_STYLE('',(#55282));
#55262=SURFACE_SIDE_STYLE('',(#55283));
#55263=SURFACE_SIDE_STYLE('',(#55284));
#55264=SURFACE_SIDE_STYLE('',(#55285));
#55265=SURFACE_SIDE_STYLE('',(#55286));
#55266=SURFACE_SIDE_STYLE('',(#55287));
#55267=SURFACE_SIDE_STYLE('',(#55288));
#55268=SURFACE_SIDE_STYLE('',(#55289));
#55269=SURFACE_SIDE_STYLE('',(#55290));
#55270=SURFACE_SIDE_STYLE('',(#55291));
#55271=SURFACE_SIDE_STYLE('',(#55292));
#55272=SURFACE_SIDE_STYLE('',(#55293));
#55273=SURFACE_SIDE_STYLE('',(#55294));
#55274=SURFACE_SIDE_STYLE('',(#55295));
#55275=SURFACE_STYLE_FILL_AREA(#55296);
#55276=SURFACE_STYLE_FILL_AREA(#55297);
#55277=SURFACE_STYLE_FILL_AREA(#55298);
#55278=SURFACE_STYLE_FILL_AREA(#55299);
#55279=SURFACE_STYLE_FILL_AREA(#55300);
#55280=SURFACE_STYLE_FILL_AREA(#55301);
#55281=SURFACE_STYLE_FILL_AREA(#55302);
#55282=SURFACE_STYLE_FILL_AREA(#55303);
#55283=SURFACE_STYLE_FILL_AREA(#55304);
#55284=SURFACE_STYLE_FILL_AREA(#55305);
#55285=SURFACE_STYLE_FILL_AREA(#55306);
#55286=SURFACE_STYLE_FILL_AREA(#55307);
#55287=SURFACE_STYLE_FILL_AREA(#55308);
#55288=SURFACE_STYLE_FILL_AREA(#55309);
#55289=SURFACE_STYLE_FILL_AREA(#55310);
#55290=SURFACE_STYLE_FILL_AREA(#55311);
#55291=SURFACE_STYLE_FILL_AREA(#55312);
#55292=SURFACE_STYLE_FILL_AREA(#55313);
#55293=SURFACE_STYLE_FILL_AREA(#55314);
#55294=SURFACE_STYLE_FILL_AREA(#55315);
#55295=SURFACE_STYLE_FILL_AREA(#55316);
#55296=FILL_AREA_STYLE('Steel - Satin',(#55317));
#55297=FILL_AREA_STYLE('MAS299_01',(#55318));
#55298=FILL_AREA_STYLE('MAS299_02',(#55319));
#55299=FILL_AREA_STYLE('MAS299_03',(#55320));
#55300=FILL_AREA_STYLE('MAS299_04',(#55321));
#55301=FILL_AREA_STYLE('MAS299_05',(#55322));
#55302=FILL_AREA_STYLE('MAS299_06',(#55323));
#55303=FILL_AREA_STYLE('MAS299_07',(#55324));
#55304=FILL_AREA_STYLE('MAS299_08',(#55325));
#55305=FILL_AREA_STYLE('MAS299_09',(#55326));
#55306=FILL_AREA_STYLE('MAS299_10',(#55327));
#55307=FILL_AREA_STYLE('MAS299_11',(#55328));
#55308=FILL_AREA_STYLE('MAS299_12',(#55329));
#55309=FILL_AREA_STYLE('MAS299_13',(#55330));
#55310=FILL_AREA_STYLE('MAS299_20',(#55331));
#55311=FILL_AREA_STYLE('MAS299_14',(#55332));
#55312=FILL_AREA_STYLE('MAS299_15',(#55333));
#55313=FILL_AREA_STYLE('MAS299_16',(#55334));
#55314=FILL_AREA_STYLE('MAS299_17',(#55335));
#55315=FILL_AREA_STYLE('MAS299_18',(#55336));
#55316=FILL_AREA_STYLE('MAS299_19',(#55337));
#55317=FILL_AREA_STYLE_COLOUR('Steel - Satin',#55338);
#55318=FILL_AREA_STYLE_COLOUR('MAS299_01',#55339);
#55319=FILL_AREA_STYLE_COLOUR('MAS299_02',#55340);
#55320=FILL_AREA_STYLE_COLOUR('MAS299_03',#55341);
#55321=FILL_AREA_STYLE_COLOUR('MAS299_04',#55342);
#55322=FILL_AREA_STYLE_COLOUR('MAS299_05',#55343);
#55323=FILL_AREA_STYLE_COLOUR('MAS299_06',#55344);
#55324=FILL_AREA_STYLE_COLOUR('MAS299_07',#55345);
#55325=FILL_AREA_STYLE_COLOUR('MAS299_08',#55346);
#55326=FILL_AREA_STYLE_COLOUR('MAS299_09',#55347);
#55327=FILL_AREA_STYLE_COLOUR('MAS299_10',#55348);
#55328=FILL_AREA_STYLE_COLOUR('MAS299_11',#55349);
#55329=FILL_AREA_STYLE_COLOUR('MAS299_12',#55350);
#55330=FILL_AREA_STYLE_COLOUR('MAS299_13',#55351);
#55331=FILL_AREA_STYLE_COLOUR('MAS299_20',#55352);
#55332=FILL_AREA_STYLE_COLOUR('MAS299_14',#55353);
#55333=FILL_AREA_STYLE_COLOUR('MAS299_15',#55354);
#55334=FILL_AREA_STYLE_COLOUR('MAS299_16',#55355);
#55335=FILL_AREA_STYLE_COLOUR('MAS299_17',#55356);
#55336=FILL_AREA_STYLE_COLOUR('MAS299_18',#55357);
#55337=FILL_AREA_STYLE_COLOUR('MAS299_19',#55358);
#55338=COLOUR_RGB('Steel - Satin',0.627450980392157,0.627450980392157,0.627450980392157);
#55339=COLOUR_RGB('MAS299_01',0.109803921568627,0.109803921568627,0.117647058823529);
#55340=COLOUR_RGB('MAS299_02',0.0941176470588235,0.0941176470588235,0.101960784313725);
#55341=COLOUR_RGB('MAS299_03',0.713725490196078,0.705882352941177,0.682352941176471);
#55342=COLOUR_RGB('MAS299_04',0.101960784313725,0.101960784313725,0.109803921568627);
#55343=COLOUR_RGB('MAS299_05',0.12156862745098,0.12156862745098,0.133333333333333);
#55344=COLOUR_RGB('MAS299_06',0.690196078431373,0.705882352941177,0.729411764705882);
#55345=COLOUR_RGB('MAS299_07',0.768627450980392,0.780392156862745,0.8);
#55346=COLOUR_RGB('MAS299_08',0.823529411764706,0.835294117647059,0.854901960784314);
#55347=COLOUR_RGB('MAS299_09',0.807843137254902,0.819607843137255,0.83921568627451);
#55348=COLOUR_RGB('MAS299_10',0.149019607843137,0.149019607843137,0.164705882352941);
#55349=COLOUR_RGB('MAS299_11',0.133333333333333,0.133333333333333,0.149019607843137);
#55350=COLOUR_RGB('MAS299_12',0.705882352941177,0.72156862745098,0.745098039215686);
#55351=COLOUR_RGB('MAS299_13',0.117647058823529,0.411764705882353,0.243137254901961);
#55352=COLOUR_RGB('MAS299_20',0.8,0.811764705882353,0.831372549019608);
#55353=COLOUR_RGB('MAS299_14',0.83921568627451,0.698039215686274,0.4);
#55354=COLOUR_RGB('MAS299_15',0.776470588235294,0.792156862745098,0.815686274509804);
#55355=COLOUR_RGB('MAS299_16',0.784313725490196,0.8,0.823529411764706);
#55356=COLOUR_RGB('MAS299_17',0.768627450980392,0.784313725490196,0.807843137254902);
#55357=COLOUR_RGB('MAS299_18',0.792156862745098,0.807843137254902,0.827450980392157);
#55358=COLOUR_RGB('MAS299_19',0.780392156862745,0.796078431372549,0.819607843137255);
#55359=COLOUR_RGB('Dark Blue',0.08,0.2,0.34);
#55360=FILL_AREA_STYLE_COLOUR('',#55359);
#55361=FILL_AREA_STYLE('',(#55360));
#55362=SURFACE_STYLE_FILL_AREA(#55361);
#55363=SURFACE_SIDE_STYLE('',(#55362));
#55364=SURFACE_STYLE_USAGE(.BOTH.,#55363);
#55365=PRESENTATION_STYLE_ASSIGNMENT((#55364));
#55366=COLOUR_RGB('Light Blue',0.38,0.62,0.78);
#55367=FILL_AREA_STYLE_COLOUR('',#55366);
#55368=FILL_AREA_STYLE('',(#55367));
#55369=SURFACE_STYLE_FILL_AREA(#55368);
#55370=SURFACE_SIDE_STYLE('',(#55369));
#55371=SURFACE_STYLE_USAGE(.BOTH.,#55370);
#55372=PRESENTATION_STYLE_ASSIGNMENT((#55371));
#55373=COLOUR_RGB('Sky Blue',0.24,0.69,0.87);
#55374=FILL_AREA_STYLE_COLOUR('',#55373);
#55375=FILL_AREA_STYLE('',(#55374));
#55376=SURFACE_STYLE_FILL_AREA(#55375);
#55377=SURFACE_SIDE_STYLE('',(#55376));
#55378=SURFACE_STYLE_USAGE(.BOTH.,#55377);
#55379=PRESENTATION_STYLE_ASSIGNMENT((#55378));
#55380=COLOUR_RGB('Grey',0.48,0.52,0.57);
#55381=FILL_AREA_STYLE_COLOUR('',#55380);
#55382=FILL_AREA_STYLE('',(#55381));
#55383=SURFACE_STYLE_FILL_AREA(#55382);
#55384=SURFACE_SIDE_STYLE('',(#55383));
#55385=SURFACE_STYLE_USAGE(.BOTH.,#55384);
#55386=PRESENTATION_STYLE_ASSIGNMENT((#55385));
#55387=COLOUR_RGB('Black',0.12,0.14,0.17);
#55388=FILL_AREA_STYLE_COLOUR('',#55387);
#55389=FILL_AREA_STYLE('',(#55388));
#55390=SURFACE_STYLE_FILL_AREA(#55389);
#55391=SURFACE_SIDE_STYLE('',(#55390));
#55392=SURFACE_STYLE_USAGE(.BOTH.,#55391);
#55393=PRESENTATION_STYLE_ASSIGNMENT((#55392));
#55394=COLOUR_RGB('Off White',0.89,0.88,0.83);
#55395=FILL_AREA_STYLE_COLOUR('',#55394);
#55396=FILL_AREA_STYLE('',(#55395));
#55397=SURFACE_STYLE_FILL_AREA(#55396);
#55398=SURFACE_SIDE_STYLE('',(#55397));
#55399=SURFACE_STYLE_USAGE(.BOTH.,#55398);
#55400=PRESENTATION_STYLE_ASSIGNMENT((#55399));
ENDSEC;
END-ISO-10303-21;
